#64843 = EDGE_CURVE ( 'NONE', #94991, #6037, #15133, .T. ) ;
#64844 = ORIENTED_EDGE ( 'NONE', *, *, #90348, .F. ) ;
#64845 = VECTOR ( 'NONE', #107102, 1000.000000000000000 ) ;
#64846 = ORIENTED_EDGE ( 'NONE', *, *, #10381, .F. ) ;
#64847 = CARTESIAN_POINT ( 'NONE',  ( 6.049999999999935874, 2.500000000000000000, -6.741600689897077281 ) ) ;
#64848 = CARTESIAN_POINT ( 'NONE',  ( -5.400000000000019895, 2.500000000000000000, 4.230127018922196669 ) ) ;
#64849 = CARTESIAN_POINT ( 'NONE',  ( 4.599999999999938360, 2.500000000000000000, -0.5928203230275541635 ) ) ;
#64850 = CARTESIAN_POINT ( 'NONE',  ( 13.54999999999989768, 2.500000000000000000, -2.511473670974877948 ) ) ;
#64851 = ORIENTED_EDGE ( 'NONE', *, *, #110774, .T. ) ;
#64852 = DIRECTION ( 'NONE',  ( 0.000000000000000000, 0.000000000000000000, 1.000000000000000000 ) ) ;
#64854 = CIRCLE ( 'NONE', #25149, 0.06509327318403745899 ) ;
#64853 = CIRCLE ( 'NONE', #127564, 0.1000000000000000056 ) ;
#64855 = LINE ( 'NONE', #5285, #124731 ) ;
#64856 = ORIENTED_EDGE ( 'NONE', *, *, #124648, .T. ) ;
#64857 = CARTESIAN_POINT ( 'NONE',  ( -13.54999999999998828, 12.50000000000000000, 1.818653347947325472 ) ) ;
#64858 = ORIENTED_EDGE ( 'NONE', *, *, #119965, .F. ) ;
#64859 = FACE_BOUND ( 'NONE', #45914, .T. ) ;
#64860 = FACE_OUTER_BOUND ( 'NONE', #36533, .T. ) ;
#64861 = ORIENTED_EDGE ( 'NONE', *, *, #867, .T. ) ;
#64862 = LINE ( 'NONE', #15094, #111230 ) ;
#64863 = DIRECTION ( 'NONE',  ( 0.000000000000000000, -0.9999939076577903929, 0.003490651415223739937 ) ) ;
#64864 = ORIENTED_EDGE ( 'NONE', *, *, #799, .T. ) ;
#64865 = ORIENTED_EDGE ( 'NONE', *, *, #127445, .T. ) ;
#64866 = CARTESIAN_POINT ( 'NONE',  ( 187.0052083336747444, -6.551208109652278289, 3.782341765624995134 ) ) ;
#64867 = DIRECTION ( 'NONE',  ( 0.000000000000000000, 0.000000000000000000, -1.000000000000000000 ) ) ;
#64868 = CARTESIAN_POINT ( 'NONE',  ( 13.74999999999989342, 12.50000000000000000, -1.472243186433550122 ) ) ;
#64869 = LINE ( 'NONE', #25587, #99637 ) ;
#64870 = CARTESIAN_POINT ( 'NONE',  ( -5.600000000000020073, 2.500000000000000000, 4.676537180435972552 ) ) ;
#64871 = PLANE ( 'NONE',  #64124 ) ;
#64872 = LINE ( 'NONE', #55070, #25481 ) ;
#64873 = AXIS2_PLACEMENT_3D ( 'NONE', #63495, #23562, #34699 ) ;
#64874 = EDGE_CURVE ( 'NONE', #80227, #109551, #3790, .T. ) ;
#64875 = AXIS2_PLACEMENT_3D ( 'NONE', #43083, #12289, #82994 ) ;
#64876 = ORIENTED_EDGE ( 'NONE', *, *, #43106, .T. ) ;
#64877 = ORIENTED_EDGE ( 'NONE', *, *, #91366, .F. ) ;
#64878 = CARTESIAN_POINT ( 'NONE',  ( 8.949999999999915801, 2.500000000000000000, -1.818653347947326138 ) ) ;
#64879 = LINE ( 'NONE', #34155, #126982 ) ;
#64880 = DIRECTION ( 'NONE',  ( 0.000000000000000000, 0.000000000000000000, 1.000000000000000000 ) ) ;
#64881 = CARTESIAN_POINT ( 'NONE',  ( 14.54999999999989591, 12.50000000000000000, 2.165063509461097713 ) ) ;
#64883 = VERTEX_POINT ( 'NONE', #113093 ) ;
#64882 = ORIENTED_EDGE ( 'NONE', *, *, #100325, .T. ) ;
#64884 = EDGE_CURVE ( 'NONE', #27262, #80417, #33273, .T. ) ;
#64885 = FACE_BOUND ( 'NONE', #44666, .T. ) ;
#64886 = ORIENTED_EDGE ( 'NONE', *, *, #96394, .T. ) ;
#64887 = EDGE_CURVE ( 'NONE', #14356, #73692, #27656, .T. ) ;
#64888 = FACE_OUTER_BOUND ( 'NONE', #43030, .T. ) ;
#64889 = DIRECTION ( 'NONE',  ( -0.000000000000000000, -1.000000000000000000, -0.000000000000000000 ) ) ;
#64890 = AXIS2_PLACEMENT_3D ( 'NONE', #66607, #97999, #37172 ) ;
#64891 = VERTEX_POINT ( 'NONE', #61442 ) ;
#64892 = CARTESIAN_POINT ( 'NONE',  ( -10.45000000000000107, 12.50000000000000000, 2.165063509461097713 ) ) ;
#64893 = FACE_OUTER_BOUND ( 'NONE', #82943, .T. ) ;
#64894 = CARTESIAN_POINT ( 'NONE',  ( 0.000000000000000000, 0.000000000000000000, -5.000000000000004441 ) ) ;
#64895 = CARTESIAN_POINT ( 'NONE',  ( 3.549999999999944755, 2.500000000000000000, -2.411473670974877859 ) ) ;
#64896 = EDGE_CURVE ( 'NONE', #17226, #39251, #123546, .T. ) ;
#64897 = CARTESIAN_POINT ( 'NONE',  ( 8.749999999999918288, 12.50000000000000000, -1.472243186433550122 ) ) ;
#64898 = DIRECTION ( 'NONE',  ( -0.000000000000000000, 1.000000000000000000, -0.000000000000000000 ) ) ;
#64899 = CARTESIAN_POINT ( 'NONE',  ( -3.300000000000027800, 2.500000000000000000, -2.276824562219559311E-15 ) ) ;
#64900 = DIRECTION ( 'NONE',  ( 0.000000000000000000, 0.000000000000000000, 1.000000000000000000 ) ) ;
#64901 = ADVANCED_FACE ( 'NONE', ( #52893 ), #56903, .T. ) ;
#64902 = FACE_OUTER_BOUND ( 'NONE', #126896, .T. ) ;
#64903 = AXIS2_PLACEMENT_3D ( 'NONE', #39424, #51163, #58408 ) ;
#64904 = VERTEX_POINT ( 'NONE', #31335 ) ;
#64905 = VERTEX_POINT ( 'NONE', #121617 ) ;
#64906 = CONICAL_SURFACE ( 'NONE', #87880, 0.09999999999999982514, 0.003490658503988666988 ) ;
#64907 = ORIENTED_EDGE ( 'NONE', *, *, #32846, .F. ) ;
#64908 = LINE ( 'NONE', #27548, #5298 ) ;
#64909 = EDGE_LOOP ( 'NONE', ( #96370, #54818 ) ) ;
#64910 = LINE ( 'NONE', #1006, #22695 ) ;
#64912 = ORIENTED_EDGE ( 'NONE', *, *, #51996, .F. ) ;
#64911 = ORIENTED_EDGE ( 'NONE', *, *, #29954, .F. ) ;
#64913 = ORIENTED_EDGE ( 'NONE', *, *, #123464, .F. ) ;
#64914 = DIRECTION ( 'NONE',  ( 0.000000000000000000, 0.000000000000000000, 1.000000000000000000 ) ) ;
#64915 = AXIS2_PLACEMENT_3D ( 'NONE', #39294, #79823, #29445 ) ;
#64916 = CARTESIAN_POINT ( 'NONE',  ( -11.89999999999999680, 2.500000000000000000, -4.676537180435976104 ) ) ;
#64917 = SURFACE_SIDE_STYLE ('',( #54460 ) ) ;
#64918 = CARTESIAN_POINT ( 'NONE',  ( 43.31340625576489600, -2.029328411527076437, -5.113049425671298387 ) ) ;
#64919 = CIRCLE ( 'NONE', #94171, 0.1000000000000002554 ) ;
#64920 = DIRECTION ( 'NONE',  ( 0.000000000000000000, 0.000000000000000000, -1.000000000000000000 ) ) ;
#64921 = CARTESIAN_POINT ( 'NONE',  ( -11.25000000000000000, 2.500000000000000000, -2.857883832488649745 ) ) ;
#64922 = VERTEX_POINT ( 'NONE', #112468 ) ;
#64923 = DIRECTION ( 'NONE',  ( 0.000000000000000000, 0.000000000000000000, -1.000000000000000000 ) ) ;
#64924 = EDGE_LOOP ( 'NONE', ( #53988, #53907, #69953, #32467 ) ) ;
#64925 = EDGE_LOOP ( 'NONE', ( #129563, #6172 ) ) ;
#64926 = VERTEX_POINT ( 'NONE', #23417 ) ;
#64927 = DIRECTION ( 'NONE',  ( 0.000000000000000000, 0.000000000000000000, 1.000000000000000000 ) ) ;
#64928 = ORIENTED_EDGE ( 'NONE', *, *, #126863, .T. ) ;
#64929 = ORIENTED_EDGE ( 'NONE', *, *, #18938, .T. ) ;
#64930 = ORIENTED_EDGE ( 'NONE', *, *, #85385, .T. ) ;
#64931 = FILL_AREA_STYLE ('',( #64299 ) ) ;
#64932 = CARTESIAN_POINT ( 'NONE',  ( 6.849999999999930367, 2.500000000000000000, -6.741600689897078169 ) ) ;
#64933 = DIRECTION ( 'NONE',  ( 0.000000000000000000, 1.000000000000000000, 0.000000000000000000 ) ) ;
#64934 = LINE ( 'NONE', #55773, #365 ) ;
#64935 = CARTESIAN_POINT ( 'NONE',  ( -10.00000000000000533, 12.50000000000000000, 0.6928203230275494784 ) ) ;
#64937 = EDGE_CURVE ( 'NONE', #86749, #92915, #44406, .T. ) ;
#64936 = CIRCLE ( 'NONE', #58696, 0.1000000000000000472 ) ;
#64938 = CARTESIAN_POINT ( 'NONE',  ( -1.850000000000033840, 2.500000000000000000, 6.941600689897073018 ) ) ;
#64939 = VERTEX_POINT ( 'NONE', #120988 ) ;
#64940 = CONICAL_SURFACE ( 'NONE', #8493, 0.1000000000000002554, 0.003490658503988666988 ) ;
#64941 = EDGE_CURVE ( 'NONE', #102506, #59130, #54854, .T. ) ;
#64942 = CIRCLE ( 'NONE', #41977, 0.09999999999999982514 ) ;
#64943 = EDGE_CURVE ( 'NONE', #45085, #33480, #121669, .T. ) ;
#64944 = DIRECTION ( 'NONE',  ( 0.000000000000000000, 0.000000000000000000, 1.000000000000000000 ) ) ;
#64945 = ORIENTED_EDGE ( 'NONE', *, *, #11975, .F. ) ;
#64946 = DIRECTION ( 'NONE',  ( 0.000000000000000000, 0.000000000000000000, 1.000000000000000000 ) ) ;
#64947 = AXIS2_PLACEMENT_3D ( 'NONE', #38118, #55819, #87200 ) ;
#64948 = ORIENTED_EDGE ( 'NONE', *, *, #70364, .F. ) ;
#64949 = DIRECTION ( 'NONE',  ( 0.000000000000000000, 0.000000000000000000, 1.000000000000000000 ) ) ;
#64950 = ADVANCED_FACE ( 'NONE', ( #1209 ), #125865, .T. ) ;
#64951 = EDGE_LOOP ( 'NONE', ( #57013, #78483, #101159, #72125 ) ) ;
#64952 = CONICAL_SURFACE ( 'NONE', #54571, 0.09999999999999982514, 0.003490658503988666988 ) ;
#64953 = ORIENTED_EDGE ( 'NONE', *, *, #117045, .F. ) ;
#64954 = DIRECTION ( 'NONE',  ( 0.000000000000000000, -0.000000000000000000, 1.000000000000000000 ) ) ;
#64955 = FACE_OUTER_BOUND ( 'NONE', #85402, .T. ) ;
#64956 = EDGE_CURVE ( 'NONE', #124385, #40490, #117537, .T. ) ;
#64957 = ADVANCED_FACE ( 'NONE', ( #2480 ), #469, .T. ) ;
#64958 = LINE ( 'NONE', #75423, #38433 ) ;
#64959 = FACE_OUTER_BOUND ( 'NONE', #90982, .T. ) ;
#64960 = ORIENTED_EDGE ( 'NONE', *, *, #8325, .F. ) ;
#64961 = CARTESIAN_POINT ( 'NONE',  ( -9.800000000000006040, 2.500000000000000000, -4.676537180435974328 ) ) ;
#64962 = CARTESIAN_POINT ( 'NONE',  ( 2.500000000000002220, 0.5000000000000002220, -9.999999999999998224 ) ) ;
#64963 = FACE_OUTER_BOUND ( 'NONE', #4561, .T. ) ;
#64964 = DIRECTION ( 'NONE',  ( 0.000000000000000000, -0.9999939076577903929, 0.003490651415223739937 ) ) ;
#64965 = EDGE_CURVE ( 'NONE', #14028, #107104, #107086, .T. ) ;
#64966 = DIRECTION ( 'NONE',  ( 0.000000000000000000, 1.000000000000000000, 0.000000000000000000 ) ) ;
#64967 = EDGE_LOOP ( 'NONE', ( #72702, #70287, #3530, #59994 ) ) ;
#64968 = EDGE_LOOP ( 'NONE', ( #53917, #51008, #57279, #18437 ) ) ;
#64969 = UNCERTAINTY_MEASURE_WITH_UNIT (LENGTH_MEASURE( 1.000000000000000082E-05 ), #129393, 'distance_accuracy_value', 'NONE');
#64970 = ORIENTED_EDGE ( 'NONE', *, *, #69506, .T. ) ;
#64971 = CARTESIAN_POINT ( 'NONE',  ( 6.849999999999927702, 2.500000000000000000, 2.511473670974873507 ) ) ;
#64972 = AXIS2_PLACEMENT_3D ( 'NONE', #81236, #84, #72703 ) ;
#64973 = DIRECTION ( 'NONE',  ( -0.000000000000000000, 1.000000000000000000, -0.000000000000000000 ) ) ;
#64974 = CIRCLE ( 'NONE', #75442, 0.06509327318403745899 ) ;
#64975 = CARTESIAN_POINT ( 'NONE',  ( 184.9218750003414016, 0.000000000000000000, 7.564683531250000925 ) ) ;
#64976 = DIRECTION ( 'NONE',  ( 0.000000000000000000, 0.000000000000000000, -1.000000000000000000 ) ) ;
#64977 = CARTESIAN_POINT ( 'NONE',  ( 11.89999999999990798, 12.50000000000000000, -3.983716857408426293 ) ) ;
#64978 = FACE_OUTER_BOUND ( 'NONE', #51757, .T. ) ;
#64979 = DIRECTION ( 'NONE',  ( 0.000000000000000000, -0.9999939076577903929, 0.003490651415223739937 ) ) ;
#64980 = ORIENTED_EDGE ( 'NONE', *, *, #16257, .T. ) ;
#64981 = CIRCLE ( 'NONE', #90106, 0.06509327318403745899 ) ;
#64982 = FACE_OUTER_BOUND ( 'NONE', #85317, .T. ) ;
#64983 = FACE_OUTER_BOUND ( 'NONE', #24952, .T. ) ;
#64984 = ORIENTED_EDGE ( 'NONE', *, *, #106983, .F. ) ;
#64985 = FACE_OUTER_BOUND ( 'NONE', #5619, .T. ) ;
#64986 = AXIS2_PLACEMENT_3D ( 'NONE', #58886, #73214, #62757 ) ;
#64987 = AXIS2_PLACEMENT_3D ( 'NONE', #52147, #2368, #52781 ) ;
#64988 = ADVANCED_FACE ( 'NONE', ( #35199 ), #21417, .T. ) ;
#64989 = ORIENTED_EDGE ( 'NONE', *, *, #33724, .T. ) ;
#64990 = DIRECTION ( 'NONE',  ( -0.000000000000000000, -1.000000000000000000, -0.000000000000000000 ) ) ;
#64991 = ORIENTED_EDGE ( 'NONE', *, *, #10660, .T. ) ;
#64992 = CARTESIAN_POINT ( 'NONE',  ( -4.150000000000024336, 2.500000000000000000, 2.065063509461097624 ) ) ;
#64993 = DIRECTION ( 'NONE',  ( -0.000000000000000000, -1.000000000000000000, -0.000000000000000000 ) ) ;
#64994 = FACE_OUTER_BOUND ( 'NONE', #21079, .T. ) ;
#64995 = AXIS2_PLACEMENT_3D ( 'NONE', #26069, #44412, #56780 ) ;
#64996 = VERTEX_POINT ( 'NONE', #115662 ) ;
#64997 = DIRECTION ( 'NONE',  ( -0.000000000000000000, -1.000000000000000000, -0.000000000000000000 ) ) ;
#64998 = DIRECTION ( 'NONE',  ( 0.000000000000000000, 1.000000000000000000, 0.000000000000000000 ) ) ;
#64999 = AXIS2_PLACEMENT_3D ( 'NONE', #32398, #63107, #72303 ) ;
#65000 = ORIENTED_EDGE ( 'NONE', *, *, #21037, .T. ) ;
#65001 = PLANE ( 'NONE',  #28549 ) ;
#65002 = VERTEX_POINT ( 'NONE', #65921 ) ;
#65003 = VERTEX_POINT ( 'NONE', #5706 ) ;
#65004 = DIRECTION ( 'NONE',  ( 0.000000000000000000, -0.000000000000000000, 1.000000000000000000 ) ) ;
#65005 = LINE ( 'NONE', #65663, #41677 ) ;
#65006 = ORIENTED_EDGE ( 'NONE', *, *, #37211, .F. ) ;
#65007 = DIRECTION ( 'NONE',  ( -0.000000000000000000, 1.000000000000000000, -0.000000000000000000 ) ) ;
#65008 = LINE ( 'NONE', #36231, #21367 ) ;
#65009 = EDGE_LOOP ( 'NONE', ( #81546, #4011, #36181, #62247 ) ) ;
#65010 = DIRECTION ( 'NONE',  ( 0.000000000000000000, 0.000000000000000000, 1.000000000000000000 ) ) ;
#65011 = FACE_OUTER_BOUND ( 'NONE', #110996, .T. ) ;
#65012 = CIRCLE ( 'NONE', #50460, 0.06509327318403745899 ) ;
#65013 = FACE_OUTER_BOUND ( 'NONE', #41719, .T. ) ;
#65014 = DIRECTION ( 'NONE',  ( 0.000000000000000000, 0.000000000000000000, 1.000000000000000000 ) ) ;
#65015 = AXIS2_PLACEMENT_3D ( 'NONE', #7315, #119217, #127119 ) ;
#65016 = AXIS2_PLACEMENT_3D ( 'NONE', #37593, #108247, #106947 ) ;
#65017 = FACE_OUTER_BOUND ( 'NONE', #112124, .T. ) ;
#65018 = CARTESIAN_POINT ( 'NONE',  ( 185.0312500006828031, 9.429780353434619030E-16, -7.700000000000000178 ) ) ;
#65019 = ADVANCED_FACE ( 'NONE', ( #14237 ), #115381, .T. ) ;
#65020 = ADVANCED_FACE ( 'NONE', ( #16158 ), #103927, .T. ) ;
#65021 = CIRCLE ( 'NONE', #14843, 0.09999999999999982514 ) ;
#65022 = ORIENTED_EDGE ( 'NONE', *, *, #124663, .T. ) ;
#65023 = VERTEX_POINT ( 'NONE', #114376 ) ;
#65024 = ORIENTED_EDGE ( 'NONE', *, *, #3809, .T. ) ;
#65025 = ORIENTED_EDGE ( 'NONE', *, *, #13371, .F. ) ;
#65026 = DIRECTION ( 'NONE',  ( 0.000000000000000000, -1.000000000000000000, -0.000000000000000000 ) ) ;
#65027 = DIRECTION ( 'NONE',  ( -4.274815082592931898E-19, -0.9999939076577903929, -0.003490651415223739937 ) ) ;
#65028 = CIRCLE ( 'NONE', #35813, 2.000000000000000000 ) ;
#65029 = DIRECTION ( 'NONE',  ( -4.274815082592931898E-19, -0.9999939076577903929, -0.003490651415223739937 ) ) ;
#65030 = VERTEX_POINT ( 'NONE', #45660 ) ;
#65031 = EDGE_CURVE ( 'NONE', #120113, #51434, #94570, .T. ) ;
#65032 = FACE_BOUND ( 'NONE', #115837, .T. ) ;
#65033 = EDGE_CURVE ( 'NONE', #103864, #35250, #73639, .T. ) ;
#65034 = FACE_OUTER_BOUND ( 'NONE', #111113, .T. ) ;
#65035 = DIRECTION ( 'NONE',  ( 0.000000000000000000, 0.000000000000000000, 1.000000000000000000 ) ) ;
#65036 = PLANE ( 'NONE',  #67927 ) ;
#65037 = DIRECTION ( 'NONE',  ( 0.000000000000000000, 1.000000000000000000, 0.000000000000000000 ) ) ;
#65038 = PLANE ( 'NONE',  #80537 ) ;
#65039 = ADVANCED_FACE ( 'NONE', ( #66561 ), #55473, .T. ) ;
#65040 = FACE_OUTER_BOUND ( 'NONE', #59898, .T. ) ;
#65041 = EDGE_CURVE ( 'NONE', #124608, #46240, #31893, .T. ) ;
#65042 = CARTESIAN_POINT ( 'NONE',  ( -11.84999999999999787, 2.500000000000000000, -6.841600689897074261 ) ) ;
#65043 = CARTESIAN_POINT ( 'NONE',  ( 3.749999999999942268, 12.50000000000000000, -1.407149913249512663 ) ) ;
#65044 = EDGE_CURVE ( 'NONE', #28259, #46373, #17179, .T. ) ;
#65045 = DIRECTION ( 'NONE',  ( 0.000000000000000000, 0.000000000000000000, 1.000000000000000000 ) ) ;
#65046 = ADVANCED_FACE ( 'NONE', ( #26658 ), #75692, .T. ) ;
#65047 = ADVANCED_FACE ( 'NONE', ( #94103 ), #38147, .T. ) ;
#65048 = DIRECTION ( 'NONE',  ( 0.000000000000000000, 0.000000000000000000, 1.000000000000000000 ) ) ;
#65049 = ORIENTED_EDGE ( 'NONE', *, *, #114417, .F. ) ;
#65050 = ORIENTED_EDGE ( 'NONE', *, *, #98337, .F. ) ;
#65051 = ORIENTED_EDGE ( 'NONE', *, *, #32295, .T. ) ;
#65052 = EDGE_LOOP ( 'NONE', ( #17328, #33323, #114125, #14162 ) ) ;
#65053 = DIRECTION ( 'NONE',  ( 0.000000000000000000, 0.000000000000000000, 1.000000000000000000 ) ) ;
#65054 = ORIENTED_EDGE ( 'NONE', *, *, #85283, .F. ) ;
#65055 = CARTESIAN_POINT ( 'NONE',  ( -3.950000000000028155, 12.50000000000000000, -6.841600689897077814 ) ) ;
#65056 = ORIENTED_EDGE ( 'NONE', *, *, #93158, .F. ) ;
#65057 = EDGE_CURVE ( 'NONE', #112512, #97470, #86191, .T. ) ;
#65058 = ORIENTED_EDGE ( 'NONE', *, *, #57081, .F. ) ;
#65059 = DIRECTION ( 'NONE',  ( 0.000000000000000000, 0.000000000000000000, 1.000000000000000000 ) ) ;
#65060 = AXIS2_PLACEMENT_3D ( 'NONE', #13110, #53064, #23592 ) ;
#65061 = CIRCLE ( 'NONE', #75530, 0.1000000000000002554 ) ;
#65062 = DIRECTION ( 'NONE',  ( 0.000000000000000000, 0.000000000000000000, 1.000000000000000000 ) ) ;
#65063 = DIRECTION ( 'NONE',  ( -4.274815082592931898E-19, -0.9999939076577903929, -0.003490651415223739937 ) ) ;
#65064 = DIRECTION ( 'NONE',  ( 0.000000000000000000, 0.000000000000000000, 1.000000000000000000 ) ) ;
#65065 = CARTESIAN_POINT ( 'NONE',  ( -11.24999999999996447, 12.50000000000000000, -6.430097255199260786 ) ) ;
#65066 = ORIENTED_EDGE ( 'NONE', *, *, #13359, .T. ) ;
#65067 = CONICAL_SURFACE ( 'NONE', #12744, 0.1000000000000002554, 0.003490658503988666988 ) ;
#65068 = AXIS2_PLACEMENT_3D ( 'NONE', #64786, #94250, #86354 ) ;
#65069 = ORIENTED_EDGE ( 'NONE', *, *, #14254, .T. ) ;
#65070 = EDGE_LOOP ( 'NONE', ( #6144, #87032, #58163, #33549 ) ) ;
#65072 = ORIENTED_EDGE ( 'NONE', *, *, #46925, .F. ) ;
#65071 = DIRECTION ( 'NONE',  ( -0.000000000000000000, -1.000000000000000000, -0.000000000000000000 ) ) ;
#65073 = DIRECTION ( 'NONE',  ( 0.000000000000000000, 0.000000000000000000, 1.000000000000000000 ) ) ;
#65074 =( BOUNDED_CURVE ( )  B_SPLINE_CURVE ( 2, ( #59757, #8039, #60398, #38160, #117995, #119942, #9985, #144, #40095, #29619, #28994, #28347, #108173, #99010, #18512, #129145, #58457, #9338, #39474, #30292, #79381, #100307, #98349, #119285, #4018, #70836, #100928, #21746, #72774, #21086, #1445, #43328, #63604, #43965, #33508, #110751, #61678, #61009, #83868, #11910, #12547, #121868, #53137, #52476, #93069, #73405, #11263, #92400, #113331, #30931, #2729, #23671, #32225, #72135, #41398, #42695, #82603, #112058, #51853, #103525, #13837, #51215, #2081, #111386, #91124, #101592, #91764, #22402, #81309, #3381, #53771, #121224, #42026, #93700, #31563, #62320, #83249, #122520, #123166, #71470, #81931, #102239, #32870, #62947, #112703 ),
 .UNSPECIFIED., .F., .F. ) 
 B_SPLINE_CURVE_WITH_KNOTS ( ( 3, 2, 2, 2, 2, 2, 2, 2, 2, 2, 2, 2, 2, 2, 2, 2, 2, 2, 2, 2, 2, 2, 2, 2, 2, 2, 2, 2, 2, 2, 2, 2, 2, 2, 2, 2, 2, 2, 2, 2, 2, 2, 3 ),
 ( 0.000000000000000000, 0.02380952380952380820, 0.04761904761904761640, 0.07142857142857142461, 0.09523809523809523281, 0.1190476190476190410, 0.1428571428571428492, 0.1666666666666666574, 0.1904761904761904656, 0.2142857142857142738, 0.2380952380952380820, 0.2619047619047619180, 0.2857142857142856984, 0.3095238095238095344, 0.3333333333333333148, 0.3571428571428571508, 0.3809523809523809312, 0.4047619047619047672, 0.4285714285714285476, 0.4523809523809523836, 0.4761904761904761640, 0.5000000000000000000, 0.5238095238095238360, 0.5476190476190476719, 0.5714285714285713969, 0.5952380952380952328, 0.6190476190476190688, 0.6428571428571429047, 0.6666666666666666297, 0.6904761904761904656, 0.7142857142857143016, 0.7380952380952381375, 0.7619047619047618625, 0.7857142857142856984, 0.8095238095238095344, 0.8333333333333333703, 0.8571428571428570953, 0.8809523809523809312, 0.9047619047619047672, 0.9285714285714286031, 0.9523809523809523281, 0.9761904761904761640, 1.000000000000000000 ),
 .UNSPECIFIED. ) 
 CURVE ( )  GEOMETRIC_REPRESENTATION_ITEM ( )  RATIONAL_B_SPLINE_CURVE ( ( 1.000000000000000000, 0.8660254037844387076, 1.000000000000000000, 0.8660254037844387076, 1.000000000000000000, 0.8660254037844387076, 1.000000000000000000, 0.8660254037844387076, 1.000000000000000000, 0.8660254037844387076, 1.000000000000000000, 0.8660254037844387076, 1.000000000000000000, 0.8660254037844387076, 1.000000000000000000, 0.8660254037844387076, 1.000000000000000000, 0.8660254037844387076, 1.000000000000000000, 0.8660254037844387076, 1.000000000000000000, 0.8660254037844387076, 1.000000000000000000, 0.8660254037844387076, 1.000000000000000000, 0.8660254037844387076, 1.000000000000000000, 0.8660254037844387076, 1.000000000000000000, 0.8660254037844387076, 1.000000000000000000, 0.8660254037844387076, 1.000000000000000000, 0.8660254037844387076, 1.000000000000000000, 0.8660254037844387076, 1.000000000000000000, 0.8660254037844387076, 1.000000000000000000, 0.8660254037844387076, 1.000000000000000000, 0.8660254037844387076, 1.000000000000000000, 0.8660254037844387076, 1.000000000000000000, 0.8660254037844387076, 1.000000000000000000, 0.8660254037844387076, 1.000000000000000000, 0.8660254037844387076, 1.000000000000000000, 0.8660254037844387076, 1.000000000000000000, 0.8660254037844387076, 1.000000000000000000, 0.8660254037844387076, 1.000000000000000000, 0.8660254037844387076, 1.000000000000000000, 0.8660254037844387076, 1.000000000000000000, 0.8660254037844387076, 1.000000000000000000, 0.8660254037844387076, 1.000000000000000000, 0.8660254037844387076, 1.000000000000000000, 0.8660254037844387076, 1.000000000000000000, 0.8660254037844387076, 1.000000000000000000, 0.8660254037844387076, 1.000000000000000000, 0.8660254037844387076, 1.000000000000000000, 0.8660254037844387076, 1.000000000000000000, 0.8660254037844387076, 1.000000000000000000, 0.8660254037844387076, 1.000000000000000000, 0.8660254037844387076, 1.000000000000000000, 0.8660254037844387076, 1.000000000000000000 ) ) 
 REPRESENTATION_ITEM ( '' )  );
#65075 = ORIENTED_EDGE ( 'NONE', *, *, #8066, .T. ) ;
#65076 = VERTEX_POINT ( 'NONE', #86854 ) ;
#65077 = VECTOR ( 'NONE', #44390, 1000.000000000000000 ) ;
#65078 = FACE_OUTER_BOUND ( 'NONE', #81454, .T. ) ;
#65079 = AXIS2_PLACEMENT_3D ( 'NONE', #16699, #76294, #116203 ) ;
#65080 = CARTESIAN_POINT ( 'NONE',  ( -8.150000000000009237, 12.50000000000000000, 6.841600689897072485 ) ) ;
#65081 = FACE_OUTER_BOUND ( 'NONE', #62897, .T. ) ;
#65082 = CARTESIAN_POINT ( 'NONE',  ( -0.6500000000000403233, 2.500000000000000000, 1.818653347947321475 ) ) ;
#65083 = AXIS2_PLACEMENT_3D ( 'NONE', #102504, #11538, #61944 ) ;
#65084 = DIRECTION ( 'NONE',  ( -0.000000000000000000, 1.000000000000000000, -0.000000000000000000 ) ) ;
#65085 = EDGE_CURVE ( 'NONE', #88607, #106514, #109138, .T. ) ;
#65086 = CONICAL_SURFACE ( 'NONE', #104792, 0.1000000000000000472, 0.003490658503988666988 ) ;
#65087 = VERTEX_POINT ( 'NONE', #84275 ) ;
#65088 = EDGE_CURVE ( 'NONE', #46379, #69366, #34563, .T. ) ;
#65089 = DIRECTION ( 'NONE',  ( -0.000000000000000000, -1.000000000000000000, -0.000000000000000000 ) ) ;
#65090 = ORIENTED_EDGE ( 'NONE', *, *, #48109, .F. ) ;
#65092 = EDGE_CURVE ( 'NONE', #11512, #107667, #64638, .T. ) ;
#65091 = CARTESIAN_POINT ( 'NONE',  ( 2.899999999999945732, 2.500000000000000000, -4.430127018922202176 ) ) ;
#65093 = VERTEX_POINT ( 'NONE', #94738 ) ;
#65094 = FACE_OUTER_BOUND ( 'NONE', #73151, .T. ) ;
#65095 = VECTOR ( 'NONE', #56082, 1000.000000000000000 ) ;
#65096 = DIRECTION ( 'NONE',  ( 0.000000000000000000, -0.000000000000000000, 1.000000000000000000 ) ) ;
#65097 = CARTESIAN_POINT ( 'NONE',  ( -8.550000000000013145, 2.500000000000000000, -6.841600689897073373 ) ) ;
#65098 = EDGE_CURVE ( 'NONE', #60150, #97364, #48721, .T. ) ;
#65099 = CARTESIAN_POINT ( 'NONE',  ( 4.999999999999935163, 2.500000000000000000, 0.6928203230275494784 ) ) ;
#65100 = EDGE_LOOP ( 'NONE', ( #119220, #57955, #114407, #128121 ) ) ;
#65101 = EDGE_CURVE ( 'NONE', #84066, #99278, #100915, .T. ) ;
#65102 = DIRECTION ( 'NONE',  ( -0.000000000000000000, -1.000000000000000000, -0.000000000000000000 ) ) ;
#65103 = ADVANCED_FACE ( 'NONE', ( #118898 ), #27766, .T. ) ;
#65104 = ADVANCED_FACE ( 'NONE', ( #39077 ), #90446, .T. ) ;
#65105 = DIRECTION ( 'NONE',  ( 0.000000000000000000, -0.000000000000000000, 1.000000000000000000 ) ) ;
#65106 = ORIENTED_EDGE ( 'NONE', *, *, #9825, .F. ) ;
#65107 = ORIENTED_EDGE ( 'NONE', *, *, #70254, .T. ) ;
#65108 = ORIENTED_EDGE ( 'NONE', *, *, #59030, .T. ) ;
#65109 = DIRECTION ( 'NONE',  ( 0.000000000000000000, 1.000000000000000000, 0.000000000000000000 ) ) ;
#65110 = DIRECTION ( 'NONE',  ( 0.000000000000000000, 1.000000000000000000, 0.000000000000000000 ) ) ;
#65111 = CARTESIAN_POINT ( 'NONE',  ( 185.6927083336747160, 6.551208109652275624, -3.782341765624998686 ) ) ;
#65112 = DIRECTION ( 'NONE',  ( 0.000000000000000000, 0.000000000000000000, -1.000000000000000000 ) ) ;
#65113 = ADVANCED_FACE ( 'NONE', ( #28592 ), #88794, .T. ) ;
#65114 = FACE_OUTER_BOUND ( 'NONE', #11969, .T. ) ;
#65115 = DIRECTION ( 'NONE',  ( -0.000000000000000000, 1.000000000000000000, -0.000000000000000000 ) ) ;
#65116 = CIRCLE ( 'NONE', #127821, 0.1000000000000002554 ) ;
#65117 = AXIS2_PLACEMENT_3D ( 'NONE', #96040, #5072, #6336 ) ;
#65118 = CONICAL_SURFACE ( 'NONE', #102775, 0.1000000000000002554, 0.003490658503988666988 ) ;
#65119 = ORIENTED_EDGE ( 'NONE', *, *, #27273, .F. ) ;
#65120 = FACE_OUTER_BOUND ( 'NONE', #28626, .T. ) ;
#65121 = AXIS2_PLACEMENT_3D ( 'NONE', #76361, #58655, #107085 ) ;
#65122 = ORIENTED_EDGE ( 'NONE', *, *, #6599, .F. ) ;
#65123 = CIRCLE ( 'NONE', #40111, 0.06509327318403745899 ) ;
#65124 = CARTESIAN_POINT ( 'NONE',  ( 7.699999999999925571, 2.500000000000000000, 3.883716857408420431 ) ) ;
#65125 = EDGE_CURVE ( 'NONE', #17389, #104949, #19350, .T. ) ;
#65126 = CARTESIAN_POINT ( 'NONE',  ( 5.449999999999936229, 2.500000000000000000, -2.065063509461102065 ) ) ;
#65127 = DIRECTION ( 'NONE',  ( 0.000000000000000000, 0.000000000000000000, -1.000000000000000000 ) ) ;
#65128 = ORIENTED_EDGE ( 'NONE', *, *, #38799, .T. ) ;
#65129 = CIRCLE ( 'NONE', #23369, 0.06509327318403745899 ) ;
#65130 = CARTESIAN_POINT ( 'NONE',  ( -11.84999999999999787, 2.500000000000000000, -1.718653347947321830 ) ) ;
#65131 = CARTESIAN_POINT ( 'NONE',  ( 1.449999999999952216, 2.500000000000000000, -2.511473670974877948 ) ) ;
#65132 = VERTEX_POINT ( 'NONE', #58059 ) ;
#65133 = CARTESIAN_POINT ( 'NONE',  ( -15.79999999999998117, 12.50000000000000000, -0.06509327318403743123 ) ) ;
#65134 = ADVANCED_FACE ( 'NONE', ( #127439 ), #128128, .T. ) ;
#65135 = ORIENTED_EDGE ( 'NONE', *, *, #106873, .F. ) ;
#65136 = VERTEX_POINT ( 'NONE', #118250 ) ;
#65137 = DIRECTION ( 'NONE',  ( 0.000000000000000000, 0.000000000000000000, 1.000000000000000000 ) ) ;
#65138 = VERTEX_POINT ( 'NONE', #68502 ) ;
#65139 = DIRECTION ( 'NONE',  ( 0.000000000000000000, -0.000000000000000000, 1.000000000000000000 ) ) ;
#65140 = DIRECTION ( 'NONE',  ( 0.000000000000000000, 0.000000000000000000, -1.000000000000000000 ) ) ;
#65141 = LINE ( 'NONE', #27814, #96082 ) ;
#65142 = AXIS2_PLACEMENT_3D ( 'NONE', #34577, #25356, #83026 ) ;
#65143 = ORIENTED_EDGE ( 'NONE', *, *, #867, .F. ) ;
#65144 = AXIS2_PLACEMENT_3D ( 'NONE', #32950, #82686, #24395 ) ;
#65145 = FACE_BOUND ( 'NONE', #25145, .T. ) ;
#65147 = ORIENTED_EDGE ( 'NONE', *, *, #82727, .T. ) ;
#65146 = CARTESIAN_POINT ( 'NONE',  ( -7.300000000000016698, 2.500000000000000000, -4.776537180435978414 ) ) ;
#65148 = CARTESIAN_POINT ( 'NONE',  ( 7.699999999999925571, 2.500000000000000000, -4.676537180435978769 ) ) ;
#65149 = EDGE_CURVE ( 'NONE', #15822, #16690, #121853, .T. ) ;
#65150 = DIRECTION ( 'NONE',  ( 0.000000000000000000, 0.000000000000000000, 1.000000000000000000 ) ) ;
#65151 = EDGE_LOOP ( 'NONE', ( #35630, #40820 ) ) ;
#65152 = AXIS2_PLACEMENT_3D ( 'NONE', #72989, #25824, #104382 ) ;
#65153 = VECTOR ( 'NONE', #99325, 1000.000000000000000 ) ;
#65154 = ORIENTED_EDGE ( 'NONE', *, *, #30584, .F. ) ;
#65155 = CONICAL_SURFACE ( 'NONE', #8730, 0.1000000000000002554, 0.003490658503988666988 ) ;
#65156 = VERTEX_POINT ( 'NONE', #69799 ) ;
#65157 = CARTESIAN_POINT ( 'NONE',  ( -3.550000000000028244, 12.50000000000000000, -1.753560074763288679 ) ) ;
#65158 = FACE_OUTER_BOUND ( 'NONE', #50418, .T. ) ;
#65159 = DIRECTION ( 'NONE',  ( -0.000000000000000000, 1.000000000000000000, -0.000000000000000000 ) ) ;
#65160 = FACE_BOUND ( 'NONE', #96811, .T. ) ;
#65161 = ORIENTED_EDGE ( 'NONE', *, *, #80300, .F. ) ;
#65162 = CARTESIAN_POINT ( 'NONE',  ( 186.0677083336747444, -4.367472073101514418, -7.564683531250002702 ) ) ;
#65163 = CARTESIAN_POINT ( 'NONE',  ( -4.600000000000025402, 12.50000000000000000, 4.395220292106234439 ) ) ;
#65164 = CARTESIAN_POINT ( 'NONE',  ( -1.450000000000036371, 12.50000000000000000, 6.776507416713035248 ) ) ;
#65165 = AXIS2_PLACEMENT_3D ( 'NONE', #118778, #29130, #69023 ) ;
#65166 = AXIS2_PLACEMENT_3D ( 'NONE', #25743, #44095, #104311 ) ;
#65167 = LINE ( 'NONE', #56004, #63794 ) ;
#65168 = AXIS2_PLACEMENT_3D ( 'NONE', #76149, #56491, #57146 ) ;
#65169 = VECTOR ( 'NONE', #51283, 1000.000000000000000 ) ;
#65170 = CIRCLE ( 'NONE', #86099, 0.06509327318403745899 ) ;
#65171 = DIRECTION ( 'NONE',  ( 0.000000000000000000, 0.000000000000000000, 1.000000000000000000 ) ) ;
#65172 = DIRECTION ( 'NONE',  ( -0.000000000000000000, -1.000000000000000000, -0.000000000000000000 ) ) ;
#65173 = DIRECTION ( 'NONE',  ( -0.000000000000000000, -1.000000000000000000, -0.000000000000000000 ) ) ;
#65174 = CARTESIAN_POINT ( 'NONE',  ( 0.6499999999999543920, 2.500000000000000000, 6.048780366869521252 ) ) ;
#65175 = DIRECTION ( 'NONE',  ( 0.000000000000000000, 0.000000000000000000, 1.000000000000000000 ) ) ;
#65176 = EDGE_CURVE ( 'NONE', #30638, #61247, #65419, .T. ) ;
#65177 = VERTEX_POINT ( 'NONE', #88114 ) ;
#65178 = AXIS2_PLACEMENT_3D ( 'NONE', #120589, #21092, #112063 ) ;
#65179 = ORIENTED_EDGE ( 'NONE', *, *, #62771, .T. ) ;
#65180 = ORIENTED_EDGE ( 'NONE', *, *, #127946, .T. ) ;
#65181 = ORIENTED_EDGE ( 'NONE', *, *, #105170, .F. ) ;
#65182 = EDGE_LOOP ( 'NONE', ( #43005, #118966 ) ) ;
#65183 = CARTESIAN_POINT ( 'NONE',  ( 0.5999999999999560130, 12.50000000000000000, -3.918623584224389056 ) ) ;
#65184 = CARTESIAN_POINT ( 'NONE',  ( 7.949999999999922018, 2.500000000000000000, -2.165063509461101710 ) ) ;
#65185 = ORIENTED_EDGE ( 'NONE', *, *, #4742, .F. ) ;
#65186 = FACE_BOUND ( 'NONE', #63732, .T. ) ;
#65187 = DIRECTION ( 'NONE',  ( 0.000000000000000000, 0.000000000000000000, 1.000000000000000000 ) ) ;
#65188 = DIRECTION ( 'NONE',  ( 0.000000000000000000, 0.000000000000000000, 1.000000000000000000 ) ) ;
#65189 = VERTEX_POINT ( 'NONE', #108426 ) ;
#65190 = ADVANCED_FACE ( 'NONE', ( #109729 ), #59080, .T. ) ;
#65191 = CARTESIAN_POINT ( 'NONE',  ( -13.29999999999998828, 12.50000000000000000, 4.330127018922196314 ) ) ;
#65192 = ADVANCED_FACE ( 'NONE', ( #107128 ), #15228, .T. ) ;
#65193 = DIRECTION ( 'NONE',  ( -0.000000000000000000, -1.000000000000000000, -0.000000000000000000 ) ) ;
#65194 = ADVANCED_FACE ( 'NONE', ( #20067 ), #37761, .T. ) ;
#65195 = LINE ( 'NONE', #94671, #85136 ) ;
#65196 = ADVANCED_FACE ( 'NONE', ( #39726 ), #25608, .T. ) ;
#65197 = ORIENTED_EDGE ( 'NONE', *, *, #54598, .F. ) ;
#65198 = FACE_OUTER_BOUND ( 'NONE', #43457, .T. ) ;
#65199 = ORIENTED_EDGE ( 'NONE', *, *, #29947, .F. ) ;
#65200 = EDGE_CURVE ( 'NONE', #128448, #110183, #79998, .T. ) ;
#65201 = EDGE_LOOP ( 'NONE', ( #120507, #124427 ) ) ;
#65202 = CONICAL_SURFACE ( 'NONE', #2506, 0.1000000000000002554, 0.003490658503988666988 ) ;
#65203 = ORIENTED_EDGE ( 'NONE', *, *, #9284, .F. ) ;
#65204 = CIRCLE ( 'NONE', #92405, 0.06509327318403745899 ) ;
#65205 = CARTESIAN_POINT ( 'NONE',  ( 2.049999999999950084, 12.50000000000000000, -2.165063509461101710 ) ) ;
#65206 = CIRCLE ( 'NONE', #54746, 0.06509327318403745899 ) ;
#65207 = DIRECTION ( 'NONE',  ( -4.274815082592931898E-19, -0.9999939076577903929, -0.003490651415223739937 ) ) ;
#65208 = DIRECTION ( 'NONE',  ( 0.000000000000000000, -1.846105847067148515E-16, -1.000000000000000000 ) ) ;
#65209 = ORIENTED_EDGE ( 'NONE', *, *, #122767, .F. ) ;
#65210 = EDGE_CURVE ( 'NONE', #80531, #125538, #117627, .T. ) ;
#65211 = CARTESIAN_POINT ( 'NONE',  ( 13.39473262194674774, 2.500000000000000000, -7.044698189560237189 ) ) ;
#65212 = EDGE_CURVE ( 'NONE', #78931, #36319, #17280, .T. ) ;
#65213 = DIRECTION ( 'NONE',  ( -0.000000000000000000, -1.000000000000000000, -0.000000000000000000 ) ) ;
#65215 = ADVANCED_FACE ( 'NONE', ( #12154 ), #32485, .T. ) ;
#65214 = TOROIDAL_SURFACE ( 'NONE', #96604, 4.500000000000003553, 0.5000000000000000000 ) ;
#65216 = VECTOR ( 'NONE', #26829, 1000.000000000000000 ) ;
#65217 = CIRCLE ( 'NONE', #117428, 0.06509327318403745899 ) ;
#65218 = FACE_OUTER_BOUND ( 'NONE', #75385, .T. ) ;
#65219 = CARTESIAN_POINT ( 'NONE',  ( 187.1927083336747160, 6.551208109652275624, -3.782341765624998686 ) ) ;
#65220 = DIRECTION ( 'NONE',  ( 0.000000000000000000, 1.000000000000000000, 0.000000000000000000 ) ) ;
#65221 = AXIS2_PLACEMENT_3D ( 'NONE', #114183, #23879, #103727 ) ;
#65222 = AXIS2_PLACEMENT_3D ( 'NONE', #85280, #106219, #104904 ) ;
#65223 = PLANE ( 'NONE',  #93406 ) ;
#65224 = ADVANCED_FACE ( 'NONE', ( #52099 ), #33119, .T. ) ;
#65225 = ORIENTED_EDGE ( 'NONE', *, *, #38522, .T. ) ;
#65226 = CARTESIAN_POINT ( 'NONE',  ( 5.849999999999933031, 12.50000000000000000, -1.472243186433550122 ) ) ;
#65227 = AXIS2_PLACEMENT_3D ( 'NONE', #21496, #11012, #93461 ) ;
#65228 = ORIENTED_EDGE ( 'NONE', *, *, #81147, .F. ) ;
#65229 = ORIENTED_EDGE ( 'NONE', *, *, #38145, .T. ) ;
#65230 = PLANE ( 'NONE',  #24176 ) ;
#65231 = DIRECTION ( 'NONE',  ( -0.000000000000000000, -1.000000000000000000, -0.000000000000000000 ) ) ;
#65232 = CARTESIAN_POINT ( 'NONE',  ( -9.150000000000009237, 2.500000000000000000, 1.472243186433545459 ) ) ;
#65233 = CARTESIAN_POINT ( 'NONE',  ( 12.29999999999990479, 12.50000000000000000, 4.611443907251934426 ) ) ;
#65234 = CARTESIAN_POINT ( 'NONE',  ( 4.349999999999936584, 2.500000000000000000, 6.248780366869520542 ) ) ;
#65235 = ORIENTED_EDGE ( 'NONE', *, *, #99264, .T. ) ;
#65236 = VERTEX_POINT ( 'NONE', #21336 ) ;
#65237 = DIRECTION ( 'NONE',  ( 0.000000000000000000, 0.000000000000000000, -1.000000000000000000 ) ) ;
#65238 = CARTESIAN_POINT ( 'NONE',  ( 8.099999999999921485, 2.500000000000000000, 0.3464101615137735735 ) ) ;
#65239 = FACE_OUTER_BOUND ( 'NONE', #14534, .T. ) ;
#65240 = ORIENTED_EDGE ( 'NONE', *, *, #33586, .T. ) ;
#65241 = ORIENTED_EDGE ( 'NONE', *, *, #41637, .T. ) ;
#65242 = LINE ( 'NONE', #114355, #8088 ) ;
#65244 = EDGE_LOOP ( 'NONE', ( #92003, #81114 ) ) ;
#65243 = AXIS2_PLACEMENT_3D ( 'NONE', #16178, #16812, #35845 ) ;
#65245 = FACE_OUTER_BOUND ( 'NONE', #61304, .T. ) ;
#65246 = FACE_OUTER_BOUND ( 'NONE', #30287, .T. ) ;
#65247 = VERTEX_POINT ( 'NONE', #61277 ) ;
#65248 = LINE ( 'NONE', #67165, #102538 ) ;
#65249 = CARTESIAN_POINT ( 'NONE',  ( -5.000000000000022204, 2.500000000000000000, 3.637306695894644726 ) ) ;
#65250 = FACE_OUTER_BOUND ( 'NONE', #72966, .T. ) ;
#65252 = AXIS2_PLACEMENT_3D ( 'NONE', #9632, #99951, #10281 ) ;
#65251 = FACE_OUTER_BOUND ( 'NONE', #88076, .T. ) ;
#65253 = ORIENTED_EDGE ( 'NONE', *, *, #61499, .F. ) ;
#65254 = AXIS2_PLACEMENT_3D ( 'NONE', #81386, #31629, #71540 ) ;
#65255 = ADVANCED_FACE ( 'NONE', ( #60642 ), #98776, .T. ) ;
#65256 = VECTOR ( 'NONE', #63038, 1000.000000000000000 ) ;
#65257 = FACE_OUTER_BOUND ( 'NONE', #91695, .T. ) ;
#65258 = AXIS2_PLACEMENT_3D ( 'NONE', #47290, #54037, #27002 ) ;
#65260 = EDGE_CURVE ( 'NONE', #121148, #24001, #121762, .T. ) ;
#65259 = DIRECTION ( 'NONE',  ( 0.000000000000000000, 0.000000000000000000, -1.000000000000000000 ) ) ;
#65261 = ORIENTED_EDGE ( 'NONE', *, *, #59904, .F. ) ;
#65262 = ORIENTED_EDGE ( 'NONE', *, *, #11742, .T. ) ;
#65263 = CARTESIAN_POINT ( 'NONE',  ( -5.600000000000020073, 12.50000000000000000, 0.3464101615137736845 ) ) ;
#65264 = PLANE ( 'NONE',  #103448 ) ;
#65265 = FACE_OUTER_BOUND ( 'NONE', #10870, .T. ) ;
#65266 = DIRECTION ( 'NONE',  ( -0.000000000000000000, 1.000000000000000000, -0.000000000000000000 ) ) ;
#65267 = CONICAL_SURFACE ( 'NONE', #82005, 0.1000000000000002554, 0.003490658503988666988 ) ;
#65268 = LINE ( 'NONE', #95392, #113801 ) ;
#65269 = EDGE_CURVE ( 'NONE', #54407, #14513, #105127, .T. ) ;
#65270 = DIRECTION ( 'NONE',  ( 0.000000000000000000, 0.000000000000000000, 1.000000000000000000 ) ) ;
#65271 = CIRCLE ( 'NONE', #52754, 0.06509327318403745899 ) ;
#65272 = DIRECTION ( 'NONE',  ( -4.274815082592931898E-19, -0.9999939076577903929, -0.003490651415223739937 ) ) ;
#65273 = VECTOR ( 'NONE', #32771, 1000.000000000000000 ) ;
#65274 = DIRECTION ( 'NONE',  ( -0.000000000000000000, -1.000000000000000000, -0.000000000000000000 ) ) ;
#65275 = CIRCLE ( 'NONE', #25556, 0.06509327318403745899 ) ;
#65276 = CARTESIAN_POINT ( 'NONE',  ( 8.149999999999923972, 2.500000000000000000, 1.718653347947321386 ) ) ;
#65277 = CIRCLE ( 'NONE', #10880, 0.1000000000000000056 ) ;
#65278 = CARTESIAN_POINT ( 'NONE',  ( 4.599999999999938360, 2.500000000000000000, -0.6928203230275541413 ) ) ;
#65279 = AXIS2_PLACEMENT_3D ( 'NONE', #57636, #68732, #98832 ) ;
#65280 = CARTESIAN_POINT ( 'NONE',  ( 12.09999999999990550, 2.500000000000000000, 5.122947341949749323 ) ) ;
#65281 = VERTEX_POINT ( 'NONE', #112309 ) ;
#65282 = AXIS2_PLACEMENT_3D ( 'NONE', #56191, #35916, #43831 ) ;
#65283 = ORIENTED_EDGE ( 'NONE', *, *, #39284, .T. ) ;
#65284 = ORIENTED_EDGE ( 'NONE', *, *, #36588, .F. ) ;
#65285 = DIRECTION ( 'NONE',  ( 0.000000000000000000, 0.000000000000000000, 1.000000000000000000 ) ) ;
#65286 = DIRECTION ( 'NONE',  ( 0.000000000000000000, 1.000000000000000000, 0.000000000000000000 ) ) ;
#65287 = DIRECTION ( 'NONE',  ( 0.000000000000000000, 1.000000000000000000, 0.000000000000000000 ) ) ;
#65288 = ORIENTED_EDGE ( 'NONE', *, *, #51657, .T. ) ;
#65289 = CARTESIAN_POINT ( 'NONE',  ( 18.09027855933934603, -2.526462839860887488, -2.685672775344543961 ) ) ;
#65290 = CARTESIAN_POINT ( 'NONE',  ( 11.44999999999990870, 12.50000000000000000, 6.906693963081109722 ) ) ;
#65292 = ORIENTED_EDGE ( 'NONE', *, *, #109740, .F. ) ;
#65291 = DIRECTION ( 'NONE',  ( 0.000000000000000000, 0.000000000000000000, -1.000000000000000000 ) ) ;
#65293 = DIRECTION ( 'NONE',  ( -0.000000000000000000, -1.000000000000000000, -0.000000000000000000 ) ) ;
#65294 = EDGE_LOOP ( 'NONE', ( #56545, #55188, #126323, #54785 ) ) ;
#65295 = ORIENTED_EDGE ( 'NONE', *, *, #19444, .T. ) ;
#65296 = VERTEX_POINT ( 'NONE', #31184 ) ;
#65297 = CIRCLE ( 'NONE', #73709, 0.06509327318403745899 ) ;
#65298 = ORIENTED_EDGE ( 'NONE', *, *, #87831, .F. ) ;
#65299 = CARTESIAN_POINT ( 'NONE',  ( 5.449999999999936229, 2.500000000000000000, -2.265063509461101798 ) ) ;
#65300 = AXIS2_PLACEMENT_3D ( 'NONE', #4512, #53012, #3264 ) ;
#65301 = CIRCLE ( 'NONE', #40289, 0.09999999999999999167 ) ;
#65302 = DIRECTION ( 'NONE',  ( 0.000000000000000000, 0.000000000000000000, 1.000000000000000000 ) ) ;
#65303 = CARTESIAN_POINT ( 'NONE',  ( 5.599999999999933031, 12.50000000000000000, -0.3464101615137783474 ) ) ;
#65304 = CARTESIAN_POINT ( 'NONE',  ( 3.549999999999944755, 12.50000000000000000, -6.841600689897077814 ) ) ;
#65306 = VERTEX_POINT ( 'NONE', #92016 ) ;
#65305 = CONICAL_SURFACE ( 'NONE', #38136, 0.1000000000000002554, 0.003490658503988666988 ) ;
#65307 = CIRCLE ( 'NONE', #111270, 0.09999999999999982514 ) ;
#65308 = AXIS2_PLACEMENT_3D ( 'NONE', #91654, #82497, #81824 ) ;
#65309 = DIRECTION ( 'NONE',  ( 0.000000000000000000, 0.000000000000000000, 1.000000000000000000 ) ) ;
#65312 = ORIENTED_EDGE ( 'NONE', *, *, #99833, .T. ) ;
#65311 = EDGE_CURVE ( 'NONE', #27245, #125732, #75787, .T. ) ;
#65310 = CIRCLE ( 'NONE', #46531, 0.1000000000000000056 ) ;
#65313 = CARTESIAN_POINT ( 'NONE',  ( 87.50000000000001421, -3.974992050023849810, -6.359987280038161828 ) ) ;
#65314 = DIRECTION ( 'NONE',  ( -0.000000000000000000, -1.000000000000000000, -0.000000000000000000 ) ) ;
#65315 = VECTOR ( 'NONE', #24850, 1000.000000000000000 ) ;
#65316 = CARTESIAN_POINT ( 'NONE',  ( 8.349999999999919709, 12.50000000000000000, 6.560283801567334372 ) ) ;
#65317 = CARTESIAN_POINT ( 'NONE',  ( 17.29982614914667849, -2.489966891809442195, 2.989943721779569241 ) ) ;
#65318 = EDGE_CURVE ( 'NONE', #24755, #115443, #41656, .T. ) ;
#65319 = AXIS2_PLACEMENT_3D ( 'NONE', #70447, #11520, #2998 ) ;
#65320 = ORIENTED_EDGE ( 'NONE', *, *, #15271, .T. ) ;
#65321 = ORIENTED_EDGE ( 'NONE', *, *, #13755, .T. ) ;
#65322 = ORIENTED_EDGE ( 'NONE', *, *, #72214, .T. ) ;
#65323 = CARTESIAN_POINT ( 'NONE',  ( -5.000000000000022204, 2.500000000000000000, 3.737306695894644371 ) ) ;
#65324 = PLANE ( 'NONE',  #39445 ) ;
#65325 = EDGE_CURVE ( 'NONE', #93435, #65003, #13083, .T. ) ;
#65326 = CARTESIAN_POINT ( 'NONE',  ( 10.19999999999991225, 12.50000000000000000, 3.983716857408420076 ) ) ;
#65327 = FACE_BOUND ( 'NONE', #64112, .T. ) ;
#65328 = LINE ( 'NONE', #85623, #26406 ) ;
#65329 = DIRECTION ( 'NONE',  ( 0.000000000000000000, 1.000000000000000000, 0.000000000000000000 ) ) ;
#65330 = DIRECTION ( 'NONE',  ( -0.000000000000000000, -1.000000000000000000, -0.000000000000000000 ) ) ;
#65331 = CARTESIAN_POINT ( 'NONE',  ( -13.14999999999999147, 2.500000000000000000, -1.918653347947324006 ) ) ;
#65332 = AXIS2_PLACEMENT_3D ( 'NONE', #55978, #76277, #67066 ) ;
#65333 = CARTESIAN_POINT ( 'NONE',  ( 187.3802083336747444, 4.367472073101515306, 7.564683531250000925 ) ) ;
#65334 = CARTESIAN_POINT ( 'NONE',  ( 14.79999999999989235, 12.50000000000000000, 0.4115034346978109769 ) ) ;
#65335 = LINE ( 'NONE', #66630, #78451 ) ;
#65336 = AXIS2_PLACEMENT_3D ( 'NONE', #106358, #115512, #27788 ) ;
#65337 = CIRCLE ( 'NONE', #96730, 0.06509327318403745899 ) ;
#65338 = VECTOR ( 'NONE', #2742, 1000.000000000000000 ) ;
#65339 = DIRECTION ( 'NONE',  ( 0.000000000000000000, 0.000000000000000000, 1.000000000000000000 ) ) ;
#65340 = EDGE_CURVE ( 'NONE', #46062, #29998, #100539, .T. ) ;
#65341 = ORIENTED_EDGE ( 'NONE', *, *, #22528, .T. ) ;
#65342 = ORIENTED_EDGE ( 'NONE', *, *, #122220, .F. ) ;
#65343 = ORIENTED_EDGE ( 'NONE', *, *, #52322, .F. ) ;
#65344 = ORIENTED_EDGE ( 'NONE', *, *, #121057, .F. ) ;
#65345 = DIRECTION ( 'NONE',  ( 0.000000000000000000, 1.000000000000000000, 0.000000000000000000 ) ) ;
#65346 = FACE_BOUND ( 'NONE', #82000, .T. ) ;
#65347 = CIRCLE ( 'NONE', #52743, 0.06509327318403745899 ) ;
#65348 = CARTESIAN_POINT ( 'NONE',  ( -13.29999999999999005, 12.50000000000000000, 1.843143693225357538E-15 ) ) ;
#65350 = EDGE_CURVE ( 'NONE', #7100, #60983, #109234, .T. ) ;
#65349 = AXIS2_PLACEMENT_3D ( 'NONE', #53797, #24985, #112733 ) ;
#65351 = ORIENTED_EDGE ( 'NONE', *, *, #55916, .T. ) ;
#65352 = EDGE_CURVE ( 'NONE', #60457, #26852, #86243, .T. ) ;
#65353 = CARTESIAN_POINT ( 'NONE',  ( 43.31961220463728068, 2.029667686321675824, 5.113275312219439428 ) ) ;
#65354 = EDGE_CURVE ( 'NONE', #42353, #40264, #40355, .T. ) ;
#65355 = CARTESIAN_POINT ( 'NONE',  ( -9.999999999999969802, 12.50000000000000000, 4.330127018922196314 ) ) ;
#65356 = EDGE_CURVE ( 'NONE', #120673, #9996, #12789, .T. ) ;
#65357 = ADVANCED_FACE ( 'NONE', ( #1054 ), #107181, .T. ) ;
#65358 = ORIENTED_EDGE ( 'NONE', *, *, #110647, .T. ) ;
#65359 = CARTESIAN_POINT ( 'NONE',  ( 5.849999999999934808, 2.500000000000000000, -5.702370205355749455 ) ) ;
#65360 = DIRECTION ( 'NONE',  ( -4.274815082592931898E-19, -0.9999939076577903929, -0.003490651415223739937 ) ) ;
#65361 = AXIS2_PLACEMENT_3D ( 'NONE', #75980, #28833, #119774 ) ;
#65362 = AXIS2_PLACEMENT_3D ( 'NONE', #18890, #128886, #107922 ) ;
#65363 = AXIS2_PLACEMENT_3D ( 'NONE', #117089, #27424, #7793 ) ;
#65364 = CIRCLE ( 'NONE', #92567, 0.06509327318403745899 ) ;
#65365 = ADVANCED_FACE ( 'NONE', ( #80271 ), #67448, .T. ) ;
#65366 = ORIENTED_EDGE ( 'NONE', *, *, #21182, .T. ) ;
#65367 = FACE_OUTER_BOUND ( 'NONE', #48200, .T. ) ;
#65368 = EDGE_CURVE ( 'NONE', #111104, #17511, #123911, .T. ) ;
#65369 = LINE ( 'NONE', #105310, #1545 ) ;
#65370 = VECTOR ( 'NONE', #123622, 1000.000000000000000 ) ;
#65371 = ADVANCED_FACE ( 'NONE', ( #110988 ), #23660, .T. ) ;
#65372 = EDGE_LOOP ( 'NONE', ( #4731, #61921, #125451, #38658 ) ) ;
#65373 = DIRECTION ( 'NONE',  ( -0.000000000000000000, 1.000000000000000000, -0.000000000000000000 ) ) ;
#65374 = EDGE_CURVE ( 'NONE', #91777, #41716, #98866, .T. ) ;
#65375 = CIRCLE ( 'NONE', #92579, 0.06509327318403745899 ) ;
#65376 = CARTESIAN_POINT ( 'NONE',  ( 11.64999999999990798, 12.50000000000000000, 7.122917578226811486 ) ) ;
#65377 = CARTESIAN_POINT ( 'NONE',  ( -10.85000000000000142, 2.500000000000000000, -2.165063509461097713 ) ) ;
#65378 = ORIENTED_EDGE ( 'NONE', *, *, #10791, .F. ) ;
#65379 = VERTEX_POINT ( 'NONE', #76724 ) ;
#65380 = CARTESIAN_POINT ( 'NONE',  ( 5.649999999999936406, 2.500000000000000000, -6.148780366869526226 ) ) ;
#65381 = EDGE_CURVE ( 'NONE', #78182, #126113, #34134, .T. ) ;
#65383 = EDGE_CURVE ( 'NONE', #59971, #84059, #103082, .T. ) ;
#65382 = VERTEX_POINT ( 'NONE', #125185 ) ;
#65384 = CARTESIAN_POINT ( 'NONE',  ( 13.94999999999989448, 2.500000000000000000, -2.511473670974877948 ) ) ;
#65385 = DIRECTION ( 'NONE',  ( 0.000000000000000000, 1.000000000000000000, 0.000000000000000000 ) ) ;
#65386 = EDGE_LOOP ( 'NONE', ( #78873, #9570, #92639, #105057 ) ) ;
#65387 = LINE ( 'NONE', #6438, #58055 ) ;
#65388 = CARTESIAN_POINT ( 'NONE',  ( -9.200000000000009948, 2.500000000000000000, -4.330127018922197202 ) ) ;
#65389 = CARTESIAN_POINT ( 'NONE',  ( -4.550000000000026468, 12.50000000000000000, -6.495190528383302464 ) ) ;
#65390 = AXIS2_PLACEMENT_3D ( 'NONE', #63498, #112604, #62850 ) ;
#65391 = CARTESIAN_POINT ( 'NONE',  ( 8.749999999999920064, 2.500000000000000000, -2.857883832488653741 ) ) ;
#65392 = AXIS2_PLACEMENT_3D ( 'NONE', #108605, #28774, #7818 ) ;
#65393 = CARTESIAN_POINT ( 'NONE',  ( 6.249999999999930722, 12.50000000000000000, -1.472243186433550122 ) ) ;
#65394 = ORIENTED_EDGE ( 'NONE', *, *, #37784, .F. ) ;
#65395 = EDGE_LOOP ( 'NONE', ( #31144, #32101 ) ) ;
#65396 = CARTESIAN_POINT ( 'NONE',  ( 7.899999999999924860, 2.500000000000000000, -4.330127018922201643 ) ) ;
#65397 = AXIS2_PLACEMENT_3D ( 'NONE', #26684, #96689, #56758 ) ;
#65398 = CARTESIAN_POINT ( 'NONE',  ( 19.09982477502536113, -0.5559300837585569033, 4.454172625795894014 ) ) ;
#65399 = CIRCLE ( 'NONE', #109319, 0.1000000000000002554 ) ;
#65401 = DIRECTION ( 'NONE',  ( -0.000000000000000000, 1.000000000000000000, -0.000000000000000000 ) ) ;
#65400 = VECTOR ( 'NONE', #68987, 1000.000000000000000 ) ;
#65403 = ORIENTED_EDGE ( 'NONE', *, *, #102791, .T. ) ;
#65402 = ORIENTED_EDGE ( 'NONE', *, *, #110090, .F. ) ;
#65404 = VERTEX_POINT ( 'NONE', #56428 ) ;
#65405 = DIRECTION ( 'NONE',  ( 0.000000000000000000, 0.000000000000000000, 1.000000000000000000 ) ) ;
#65406 = DIRECTION ( 'NONE',  ( -0.000000000000000000, -1.000000000000000000, -0.000000000000000000 ) ) ;
#65407 = CIRCLE ( 'NONE', #98852, 0.09999999999999982514 ) ;
#65409 = LINE ( 'NONE', #45792, #110448 ) ;
#65408 = CONICAL_SURFACE ( 'NONE', #84288, 0.1000000000000002554, 0.003490658503988666988 ) ;
#65410 = CIRCLE ( 'NONE', #36190, 0.06509327318403745899 ) ;
#65411 = CARTESIAN_POINT ( 'NONE',  ( 2.899999999999945732, 2.500000000000000000, -4.330127018922201643 ) ) ;
#65412 = CARTESIAN_POINT ( 'NONE',  ( -6.250000000000017764, 2.500000000000000000, 2.857883832488649301 ) ) ;
#65413 = CARTESIAN_POINT ( 'NONE',  ( 184.5000000000000000, 9.429780353434619030E-16, 7.699999999999999289 ) ) ;
#65414 = CIRCLE ( 'NONE', #121758, 0.1000000000000002554 ) ;
#65415 = DIRECTION ( 'NONE',  ( -0.000000000000000000, -1.000000000000000000, -0.000000000000000000 ) ) ;
#65416 = FACE_OUTER_BOUND ( 'NONE', #125707, .T. ) ;
#65417 = AXIS2_PLACEMENT_3D ( 'NONE', #63333, #101333, #111114 ) ;
#65418 = DIRECTION ( 'NONE',  ( -4.274815082592931898E-19, -0.9999939076577903929, -0.003490651415223739937 ) ) ;
#65419 = CIRCLE ( 'NONE', #8886, 0.06509327318403745899 ) ;
#65420 = ORIENTED_EDGE ( 'NONE', *, *, #62783, .F. ) ;
#65421 = EDGE_CURVE ( 'NONE', #65795, #117086, #4864, .T. ) ;
#65422 = ADVANCED_FACE ( 'NONE', ( #68178 ), #6906, .T. ) ;
#65423 = CARTESIAN_POINT ( 'NONE',  ( -0.8000000000000376810, 2.500000000000000000, -4.230127018922201998 ) ) ;
#65424 = VERTEX_POINT ( 'NONE', #116640 ) ;
#65425 = ORIENTED_EDGE ( 'NONE', *, *, #37059, .T. ) ;
#65426 = DIRECTION ( 'NONE',  ( 0.000000000000000000, 0.000000000000000000, 1.000000000000000000 ) ) ;
#65427 = CARTESIAN_POINT ( 'NONE',  ( 8.099999999999923261, 12.50000000000000000, -4.676537180435978769 ) ) ;
#65428 = DIRECTION ( 'NONE',  ( 0.000000000000000000, 0.000000000000000000, 1.000000000000000000 ) ) ;
#65429 = AXIS2_PLACEMENT_3D ( 'NONE', #10580, #39452, #50518 ) ;
#65430 = DIRECTION ( 'NONE',  ( -0.000000000000000000, 1.000000000000000000, -0.000000000000000000 ) ) ;
#65431 = CARTESIAN_POINT ( 'NONE',  ( -10.65000000000000213, 12.50000000000000000, 1.883746621131358934 ) ) ;
#65432 = DIRECTION ( 'NONE',  ( 0.000000000000000000, -0.000000000000000000, 1.000000000000000000 ) ) ;
#65433 = DIRECTION ( 'NONE',  ( 0.000000000000000000, 0.000000000000000000, 1.000000000000000000 ) ) ;
#65434 = ORIENTED_EDGE ( 'NONE', *, *, #78900, .F. ) ;
#65435 = CARTESIAN_POINT ( 'NONE',  ( -1.650000000000034772, 2.500000000000000000, 5.802370205355744659 ) ) ;
#65436 = CIRCLE ( 'NONE', #40328, 0.1000000000000002554 ) ;
#65437 = CARTESIAN_POINT ( 'NONE',  ( -7.100000000000017408, 2.500000000000000000, 0.6928203230275494784 ) ) ;
#65438 = VERTEX_POINT ( 'NONE', #108110 ) ;
#65439 = CONICAL_SURFACE ( 'NONE', #54977, 0.09999999999999982514, 0.003490658503988666988 ) ;
#65440 = ORIENTED_EDGE ( 'NONE', *, *, #101270, .T. ) ;
#65441 = ORIENTED_EDGE ( 'NONE', *, *, #55319, .F. ) ;
#65442 = VERTEX_POINT ( 'NONE', #86538 ) ;
#65443 = CONICAL_SURFACE ( 'NONE', #61263, 0.09999999999999999167, 0.003490658503988666988 ) ;
#65444 = DIRECTION ( 'NONE',  ( 0.000000000000000000, 1.000000000000000000, 0.000000000000000000 ) ) ;
#65445 = DIRECTION ( 'NONE',  ( -0.000000000000000000, -1.000000000000000000, -0.000000000000000000 ) ) ;
#65446 = AXIS2_PLACEMENT_3D ( 'NONE', #45649, #124198, #126780 ) ;
#65447 = AXIS2_PLACEMENT_3D ( 'NONE', #29500, #20324, #81176 ) ;
#65448 = LINE ( 'NONE', #105385, #86136 ) ;
#65449 = CARTESIAN_POINT ( 'NONE',  ( -3.350000000000028955, 12.50000000000000000, -2.165063509461101710 ) ) ;
#65450 = CARTESIAN_POINT ( 'NONE',  ( 10.39999999999991331, 12.50000000000000000, -2.385244779468109755E-15 ) ) ;
#65451 = EDGE_LOOP ( 'NONE', ( #70241, #23678, #66662, #69218 ) ) ;
#65452 = CARTESIAN_POINT ( 'NONE',  ( 2.899999999999946620, 12.50000000000000000, -5.088040615133791356 ) ) ;
#65453 = CARTESIAN_POINT ( 'NONE',  ( -3.749999999999991118, 2.500000000000000000, 2.165063509461097713 ) ) ;
#65454 = CIRCLE ( 'NONE', #42208, 0.1000000000000002554 ) ;
#65455 = DIRECTION ( 'NONE',  ( -0.000000000000000000, 1.000000000000000000, -0.000000000000000000 ) ) ;
#65456 = EDGE_CURVE ( 'NONE', #117955, #30611, #6652, .T. ) ;
#65457 = VERTEX_POINT ( 'NONE', #36811 ) ;
#65458 = CIRCLE ( 'NONE', #94809, 0.06509327318403745899 ) ;
#65459 = CIRCLE ( 'NONE', #55107, 0.1000000000000002554 ) ;
#65460 = AXIS2_PLACEMENT_3D ( 'NONE', #122889, #11635, #50931 ) ;
#65461 = ORIENTED_EDGE ( 'NONE', *, *, #44535, .F. ) ;
#65462 = EDGE_LOOP ( 'NONE', ( #65515, #68371 ) ) ;
#65463 = CARTESIAN_POINT ( 'NONE',  ( -3.750000000000027978, 2.500000000000000000, 7.288010851410849256 ) ) ;
#65464 = CIRCLE ( 'NONE', #52963, 0.06509327318403745899 ) ;
#65465 = CARTESIAN_POINT ( 'NONE',  ( 0.4499999999999569344, 2.500000000000000000, -2.165063509461101710 ) ) ;
#65466 = FACE_OUTER_BOUND ( 'NONE', #74177, .T. ) ;
#65467 = CIRCLE ( 'NONE', #121625, 0.06509327318403745899 ) ;
#65469 = ORIENTED_EDGE ( 'NONE', *, *, #82750, .F. ) ;
#65468 = EDGE_CURVE ( 'NONE', #125450, #120640, #46650, .T. ) ;
#65470 = DIRECTION ( 'NONE',  ( 0.000000000000000000, 0.000000000000000000, 1.000000000000000000 ) ) ;
#65471 = CARTESIAN_POINT ( 'NONE',  ( -9.600000000000006750, 2.500000000000000000, 4.922947341949748257 ) ) ;
#65472 = DIRECTION ( 'NONE',  ( 0.000000000000000000, 1.000000000000000000, 0.000000000000000000 ) ) ;
#65473 = DIRECTION ( 'NONE',  ( -0.000000000000000000, 1.000000000000000000, -0.000000000000000000 ) ) ;
#65474 = EDGE_CURVE ( 'NONE', #60587, #102800, #50855, .T. ) ;
#65475 = CARTESIAN_POINT ( 'NONE',  ( -3.550000000000031797, 12.50000000000000000, -6.148780366869526226 ) ) ;
#65476 = ORIENTED_EDGE ( 'NONE', *, *, #71560, .F. ) ;
#65477 = DIRECTION ( 'NONE',  ( 0.000000000000000000, 0.000000000000000000, 1.000000000000000000 ) ) ;
#65478 = EDGE_LOOP ( 'NONE', ( #65378, #284, #50462, #61048 ) ) ;
#65479 = VERTEX_POINT ( 'NONE', #75422 ) ;
#65480 = CONICAL_SURFACE ( 'NONE', #4837, 0.09999999999999982514, 0.003490658503988666988 ) ;
#65481 = ORIENTED_EDGE ( 'NONE', *, *, #56849, .T. ) ;
#65482 = AXIS2_PLACEMENT_3D ( 'NONE', #40622, #32729, #92928 ) ;
#65483 = EDGE_CURVE ( 'NONE', #17533, #117178, #99509, .T. ) ;
#65484 = DIRECTION ( 'NONE',  ( 0.000000000000000000, 0.000000000000000000, -1.000000000000000000 ) ) ;
#65485 = FACE_BOUND ( 'NONE', #8722, .T. ) ;
#65486 = CARTESIAN_POINT ( 'NONE',  ( 4.599999999999939249, 2.500000000000000000, -3.737306695894649700 ) ) ;
#65487 = FACE_OUTER_BOUND ( 'NONE', #109839, .T. ) ;
#65488 = DIRECTION ( 'NONE',  ( -4.274815082592931898E-19, -0.9999939076577903929, -0.003490651415223739937 ) ) ;
#65489 = AXIS2_PLACEMENT_3D ( 'NONE', #37838, #108510, #116390 ) ;
#65490 = AXIS2_PLACEMENT_3D ( 'NONE', #82697, #102326, #92490 ) ;
#65491 = ORIENTED_EDGE ( 'NONE', *, *, #3758, .T. ) ;
#65492 = DIRECTION ( 'NONE',  ( 0.000000000000000000, 1.000000000000000000, 0.000000000000000000 ) ) ;
#65493 = CARTESIAN_POINT ( 'NONE',  ( 13.74999999999993072, 2.500000000000000000, -2.265063509461101798 ) ) ;
#65494 = DIRECTION ( 'NONE',  ( -0.000000000000000000, -1.000000000000000000, -0.000000000000000000 ) ) ;
#65495 = CARTESIAN_POINT ( 'NONE',  ( 7.099999999999926814, 12.50000000000000000, -0.6928203230275541413 ) ) ;
#65496 = ORIENTED_EDGE ( 'NONE', *, *, #73953, .T. ) ;
#65498 = CARTESIAN_POINT ( 'NONE',  ( 175.5000000000000000, 0.000000000000000000, -2.500000000000000000 ) ) ;
#65497 = AXIS2_PLACEMENT_3D ( 'NONE', #73350, #92343, #23616 ) ;
#65499 = AXIS2_PLACEMENT_3D ( 'NONE', #120631, #88593, #40141 ) ;
#65500 = AXIS2_PLACEMENT_3D ( 'NONE', #122034, #121372, #12065 ) ;
#65501 = FACE_OUTER_BOUND ( 'NONE', #95545, .T. ) ;
#65502 = VECTOR ( 'NONE', #42398, 1000.000000000000000 ) ;
#65503 = VERTEX_POINT ( 'NONE', #57069 ) ;
#65504 = CONICAL_SURFACE ( 'NONE', #44588, 0.1000000000000002554, 0.003490658503988666988 ) ;
#65505 = DIRECTION ( 'NONE',  ( -4.274815082592931898E-19, -0.9999939076577903929, -0.003490651415223739937 ) ) ;
#65506 = ORIENTED_EDGE ( 'NONE', *, *, #39437, .F. ) ;
#65507 = FACE_BOUND ( 'NONE', #70545, .T. ) ;
#65508 = AXIS2_PLACEMENT_3D ( 'NONE', #39406, #41331, #111310 ) ;
#65509 = DIRECTION ( 'NONE',  ( 0.000000000000000000, 0.000000000000000000, -1.000000000000000000 ) ) ;
#65510 = ADVANCED_FACE ( 'NONE', ( #97648 ), #42462, .T. ) ;
#65511 = VERTEX_POINT ( 'NONE', #27600 ) ;
#65512 = CARTESIAN_POINT ( 'NONE',  ( 9.599999999999914380, 12.50000000000000000, 3.637306695894644726 ) ) ;
#65513 = DIRECTION ( 'NONE',  ( 0.000000000000000000, 0.000000000000000000, 1.000000000000000000 ) ) ;
#65514 = EDGE_LOOP ( 'NONE', ( #12394, #115274 ) ) ;
#65515 = ORIENTED_EDGE ( 'NONE', *, *, #116206, .F. ) ;
#65516 = EDGE_CURVE ( 'NONE', #49071, #104330, #97005, .T. ) ;
#65517 = CARTESIAN_POINT ( 'NONE',  ( 185.9635416670080872, -4.367472073101519747, 7.564683531249999149 ) ) ;
#65518 = EDGE_CURVE ( 'NONE', #55213, #23957, #57107, .T. ) ;
#65519 = ORIENTED_EDGE ( 'NONE', *, *, #20204, .F. ) ;
#65520 = CARTESIAN_POINT ( 'NONE',  ( 185.2552083336747444, 6.551208109652275624, -3.782341765624998686 ) ) ;
#65521 = LINE ( 'NONE', #15769, #21932 ) ;
#65522 = FACE_OUTER_BOUND ( 'NONE', #36960, .T. ) ;
#65523 = DIRECTION ( 'NONE',  ( -4.274815082592931898E-19, -0.9999939076577903929, -0.003490651415223739937 ) ) ;
#65524 = ADVANCED_FACE ( 'NONE', ( #95728 ), #127129, .T. ) ;
#65525 = ADVANCED_FACE ( 'NONE', ( #105547 ), #15856, .T. ) ;
#65526 = DIRECTION ( 'NONE',  ( 0.000000000000000000, 1.000000000000000000, 0.000000000000000000 ) ) ;
#65527 = ADVANCED_FACE ( 'NONE', ( #76083 ), #73834, .T. ) ;
#65528 = AXIS2_PLACEMENT_3D ( 'NONE', #112061, #82609, #70201 ) ;
#65529 = AXIS2_PLACEMENT_3D ( 'NONE', #106384, #44904, #65150 ) ;
#65530 = ORIENTED_EDGE ( 'NONE', *, *, #57183, .F. ) ;
#65531 = ORIENTED_EDGE ( 'NONE', *, *, #106005, .F. ) ;
#65532 = FACE_OUTER_BOUND ( 'NONE', #123982, .T. ) ;
#65533 = EDGE_CURVE ( 'NONE', #43052, #74901, #115582, .T. ) ;
#65534 = DIRECTION ( 'NONE',  ( -4.274815082592931898E-19, -0.9999939076577903929, -0.003490651415223739937 ) ) ;
#65535 = CARTESIAN_POINT ( 'NONE',  ( -7.900000000000011013, 2.500000000000000000, 4.330127018922196314 ) ) ;
#65536 = DIRECTION ( 'NONE',  ( -0.000000000000000000, 1.000000000000000000, -0.000000000000000000 ) ) ;
#65538 = VERTEX_POINT ( 'NONE', #118569 ) ;
#65537 = ORIENTED_EDGE ( 'NONE', *, *, #117578, .T. ) ;
#65539 = FACE_BOUND ( 'NONE', #30419, .T. ) ;
#65540 = ORIENTED_EDGE ( 'NONE', *, *, #9480, .F. ) ;
#65541 = CIRCLE ( 'NONE', #67584, 0.06509327318403745899 ) ;
#65542 = DIRECTION ( 'NONE',  ( -0.000000000000000000, -1.000000000000000000, -0.000000000000000000 ) ) ;
#65543 = DIRECTION ( 'NONE',  ( 0.000000000000000000, -0.9999939076577903929, 0.003490651415223739937 ) ) ;
#65544 = AXIS2_PLACEMENT_3D ( 'NONE', #51455, #100525, #2312 ) ;
#65545 = EDGE_CURVE ( 'NONE', #72858, #102123, #28928, .T. ) ;
#65546 = ORIENTED_EDGE ( 'NONE', *, *, #58044, .F. ) ;
#65547 = PLANE ( 'NONE',  #24210 ) ;
#65548 = DIRECTION ( 'NONE',  ( -4.274815082592931898E-19, -0.9999939076577903929, -0.003490651415223739937 ) ) ;
#65549 = AXIS2_PLACEMENT_3D ( 'NONE', #68528, #58084, #106045 ) ;
#65550 = LINE ( 'NONE', #123813, #22136 ) ;
#65551 = DIRECTION ( 'NONE',  ( 0.000000000000000000, 0.000000000000000000, -1.000000000000000000 ) ) ;
#65552 = DIRECTION ( 'NONE',  ( -0.000000000000000000, 1.000000000000000000, -0.000000000000000000 ) ) ;
#65553 = CARTESIAN_POINT ( 'NONE',  ( -9.550000000000002487, 2.500000000000000000, 6.495190528383297135 ) ) ;
#65554 = CARTESIAN_POINT ( 'NONE',  ( 186.3593750003414016, 0.000000000000000000, 7.564683531250000925 ) ) ;
#65555 = FACE_OUTER_BOUND ( 'NONE', #63706, .T. ) ;
#65556 = DIRECTION ( 'NONE',  ( 0.000000000000000000, 1.000000000000000000, 0.000000000000000000 ) ) ;
#65557 = EDGE_LOOP ( 'NONE', ( #55635, #80282 ) ) ;
#65558 = ORIENTED_EDGE ( 'NONE', *, *, #43878, .F. ) ;
#65559 = CARTESIAN_POINT ( 'NONE',  ( -12.49999999999999289, 2.500000000000000000, 3.537306695894645081 ) ) ;
#65561 = EDGE_LOOP ( 'NONE', ( #86771, #28666, #33601, #92035 ) ) ;
#65560 = AXIS2_PLACEMENT_3D ( 'NONE', #963, #40923, #80829 ) ;
#65562 = CONICAL_SURFACE ( 'NONE', #113687, 0.1000000000000002554, 0.003490658503988666988 ) ;
#65563 = DIRECTION ( 'NONE',  ( 0.000000000000000000, -0.9999939076577903929, 0.003490651415223739937 ) ) ;
#65565 = VERTEX_POINT ( 'NONE', #728 ) ;
#65564 = VERTEX_POINT ( 'NONE', #120518 ) ;
#65566 = EDGE_LOOP ( 'NONE', ( #42195, #105537 ) ) ;
#65567 = AXIS2_PLACEMENT_3D ( 'NONE', #28516, #118819, #108348 ) ;
#65568 = CARTESIAN_POINT ( 'NONE',  ( 12.09999999999990550, 12.50000000000000000, 5.022947341949748790 ) ) ;
#65569 = CONICAL_SURFACE ( 'NONE', #88544, 0.09999999999999982514, 0.003490658503988666988 ) ;
#65570 = PLANE ( 'NONE',  #853 ) ;
#65571 = CARTESIAN_POINT ( 'NONE',  ( 5.599999999999931255, 2.500000000000000000, 4.676537180435972552 ) ) ;
#65572 = DIRECTION ( 'NONE',  ( 0.000000000000000000, 0.000000000000000000, 1.000000000000000000 ) ) ;
#65573 = PLANE ( 'NONE',  #12031 ) ;
#65574 = ORIENTED_EDGE ( 'NONE', *, *, #102644, .T. ) ;
#65575 = DIRECTION ( 'NONE',  ( -0.000000000000000000, -1.000000000000000000, -0.000000000000000000 ) ) ;
#65576 = ORIENTED_EDGE ( 'NONE', *, *, #101620, .F. ) ;
#65577 = VERTEX_POINT ( 'NONE', #48559 ) ;
#65578 = ORIENTED_EDGE ( 'NONE', *, *, #87524, .T. ) ;
#65579 = EDGE_CURVE ( 'NONE', #93847, #87716, #75889, .T. ) ;
#65580 = VERTEX_POINT ( 'NONE', #81241 ) ;
#65581 = DIRECTION ( 'NONE',  ( 0.000000000000000000, 0.000000000000000000, -1.000000000000000000 ) ) ;
#65582 = AXIS2_PLACEMENT_3D ( 'NONE', #51602, #33870, #31959 ) ;
#65583 = CIRCLE ( 'NONE', #9150, 0.1000000000000002554 ) ;
#65584 = ORIENTED_EDGE ( 'NONE', *, *, #66726, .F. ) ;
#65585 = ORIENTED_EDGE ( 'NONE', *, *, #73783, .T. ) ;
#65586 = FACE_OUTER_BOUND ( 'NONE', #61873, .T. ) ;
#65587 = ADVANCED_FACE ( 'NONE', ( #30864 ), #109398, .T. ) ;
#65588 = CARTESIAN_POINT ( 'NONE',  ( 0.6499999999999561684, 2.500000000000000000, 1.918653347947321564 ) ) ;
#65589 = CIRCLE ( 'NONE', #111559, 0.06509327318403745899 ) ;
#65590 = FACE_OUTER_BOUND ( 'NONE', #20786, .T. ) ;
#65592 = DIRECTION ( 'NONE',  ( 0.000000000000000000, 0.000000000000000000, 1.000000000000000000 ) ) ;
#65591 = CIRCLE ( 'NONE', #124177, 0.1000000000000000472 ) ;
#65593 = CARTESIAN_POINT ( 'NONE',  ( -4.800000000000028244, 12.50000000000000000, -4.048810130592463530 ) ) ;
#65594 = AXIS2_PLACEMENT_3D ( 'NONE', #109399, #97006, #98285 ) ;
#65595 = CARTESIAN_POINT ( 'NONE',  ( -1.450000000000035927, 2.500000000000000000, -1.918653347947326004 ) ) ;
#65596 = ORIENTED_EDGE ( 'NONE', *, *, #39230, .T. ) ;
#65597 = DIRECTION ( 'NONE',  ( 0.000000000000000000, 0.000000000000000000, -1.000000000000000000 ) ) ;
#65598 = VECTOR ( 'NONE', #3189, 1000.000000000000000 ) ;
#65600 = ORIENTED_EDGE ( 'NONE', *, *, #113424, .F. ) ;
#65599 = CIRCLE ( 'NONE', #25893, 0.1000000000000000472 ) ;
#65601 = DIRECTION ( 'NONE',  ( -4.274815082592931898E-19, -0.9999939076577903929, -0.003490651415223739937 ) ) ;
#65602 = EDGE_LOOP ( 'NONE', ( #92384, #29594 ) ) ;
#65603 = PLANE ( 'NONE',  #104643 ) ;
#65604 = ORIENTED_EDGE ( 'NONE', *, *, #15385, .T. ) ;
#65605 = AXIS2_PLACEMENT_3D ( 'NONE', #79300, #40016, #60928 ) ;
#65606 = ORIENTED_EDGE ( 'NONE', *, *, #50425, .T. ) ;
#65607 = CARTESIAN_POINT ( 'NONE',  ( -0.8500000000000386136, 2.500000000000000000, 2.757883832488649656 ) ) ;
#65608 = DIRECTION ( 'NONE',  ( 0.000000000000000000, 0.000000000000000000, -1.000000000000000000 ) ) ;
#65609 = DIRECTION ( 'NONE',  ( 0.000000000000000000, 0.000000000000000000, 1.000000000000000000 ) ) ;
#65610 = CARTESIAN_POINT ( 'NONE',  ( -13.14999999999999147, 2.500000000000000000, 2.511473670974877503 ) ) ;
#65611 = CARTESIAN_POINT ( 'NONE',  ( -13.29999999999999005, 2.500000000000000000, -4.430127018922199511 ) ) ;
#65612 = ORIENTED_EDGE ( 'NONE', *, *, #28602, .T. ) ;
#65613 = CARTESIAN_POINT ( 'NONE',  ( -1.250000000000035749, 2.500000000000000000, -2.957883832488653830 ) ) ;
#65614 = CARTESIAN_POINT ( 'NONE',  ( 6.049999999999934097, 2.500000000000000000, -2.511473670974877948 ) ) ;
#65615 = FACE_OUTER_BOUND ( 'NONE', #41756, .T. ) ;
#65616 = DIRECTION ( 'NONE',  ( 0.000000000000000000, 0.000000000000000000, -1.000000000000000000 ) ) ;
#65617 = AXIS2_PLACEMENT_3D ( 'NONE', #129117, #108788, #8645 ) ;
#65618 = CARTESIAN_POINT ( 'NONE',  ( -10.40000000000000213, 2.500000000000000000, 4.330127018922196314 ) ) ;
#65619 = ADVANCED_FACE ( 'NONE', ( #59019 ), #666, .T. ) ;
#65620 = EDGE_LOOP ( 'NONE', ( #35308, #67285 ) ) ;
#65621 = EDGE_LOOP ( 'NONE', ( #67465, #84148 ) ) ;
#65622 = ORIENTED_EDGE ( 'NONE', *, *, #64965, .T. ) ;
#65623 = AXIS2_PLACEMENT_3D ( 'NONE', #13188, #95001, #115915 ) ;
#65624 = DIRECTION ( 'NONE',  ( -0.000000000000000000, 1.000000000000000000, -0.000000000000000000 ) ) ;
#65626 = EDGE_CURVE ( 'NONE', #32850, #56986, #82159, .T. ) ;
#65625 = DIRECTION ( 'NONE',  ( 0.000000000000000000, 0.000000000000000000, -1.000000000000000000 ) ) ;
#65627 = CIRCLE ( 'NONE', #99094, 0.06509327318403743123 ) ;
#65628 = EDGE_CURVE ( 'NONE', #35861, #121566, #119223, .T. ) ;
#65629 = CARTESIAN_POINT ( 'NONE',  ( 187.3750000000000000, 8.891194145520236347, 5.444286225454521982E-16 ) ) ;
#65630 = PLANE ( 'NONE',  #92892 ) ;
#65631 = CARTESIAN_POINT ( 'NONE',  ( -9.200000000000006395, 12.50000000000000000, -0.06509327318403980434 ) ) ;
#65632 = DIRECTION ( 'NONE',  ( 0.000000000000000000, 1.000000000000000000, 0.000000000000000000 ) ) ;
#65633 = EDGE_CURVE ( 'NONE', #73190, #60441, #21677, .T. ) ;
#65634 = DIRECTION ( 'NONE',  ( -1.000000000000000000, -0.000000000000000000, -0.000000000000000000 ) ) ;
#65635 = ORIENTED_EDGE ( 'NONE', *, *, #46632, .T. ) ;
#65636 = AXIS2_PLACEMENT_3D ( 'NONE', #15966, #44154, #83454 ) ;
#65637 = VECTOR ( 'NONE', #20730, 1000.000000000000000 ) ;
#65638 = DIRECTION ( 'NONE',  ( 0.000000000000000000, 0.000000000000000000, -1.000000000000000000 ) ) ;
#65639 = CARTESIAN_POINT ( 'NONE',  ( 8.099999999999923261, 2.500000000000000000, 4.776537180435972196 ) ) ;
#65640 = EDGE_CURVE ( 'NONE', #7221, #36118, #92619, .T. ) ;
#65641 = ORIENTED_EDGE ( 'NONE', *, *, #110875, .F. ) ;
#65642 = EDGE_CURVE ( 'NONE', #74504, #59695, #27867, .T. ) ;
#65643 = DIRECTION ( 'NONE',  ( 0.000000000000000000, 1.000000000000000000, 0.000000000000000000 ) ) ;
#65644 = DIRECTION ( 'NONE',  ( 0.000000000000000000, 0.000000000000000000, -1.000000000000000000 ) ) ;
#65645 = DIRECTION ( 'NONE',  ( 0.000000000000000000, 0.000000000000000000, 1.000000000000000000 ) ) ;
#65646 = ORIENTED_EDGE ( 'NONE', *, *, #76209, .F. ) ;
#65647 = VECTOR ( 'NONE', #28323, 1000.000000000000000 ) ;
#65648 = AXIS2_PLACEMENT_3D ( 'NONE', #33994, #32724, #73911 ) ;
#65649 = LINE ( 'NONE', #28313, #59450 ) ;
#65650 = B_SPLINE_CURVE_WITH_KNOTS ( 'NONE', 3,
 ( #4364, #84232, #34524, #113712, #124824, #52856, #2444, #44981, #52217, #24048 ),
 .UNSPECIFIED., .F., .F.,
 ( 4, 2, 2, 2, 4 ),
 ( 1.339801017408199283E-15, 0.001880205780637580646, 0.003760411561273821219, 0.005640617341910062442, 0.007520823122546303231 ),
 .UNSPECIFIED. ) ;
#65652 = ORIENTED_EDGE ( 'NONE', *, *, #85886, .T. ) ;
#65651 = AXIS2_PLACEMENT_3D ( 'NONE', #75505, #105631, #74879 ) ;
#65653 = LINE ( 'NONE', #96388, #73053 ) ;
#65654 = DIRECTION ( 'NONE',  ( 0.000000000000000000, -0.9999939076577903929, 0.003490651415223739937 ) ) ;
#65655 = VERTEX_POINT ( 'NONE', #70768 ) ;
#65656 = DIRECTION ( 'NONE',  ( 0.000000000000000000, 1.000000000000000000, 0.000000000000000000 ) ) ;
#65657 = CARTESIAN_POINT ( 'NONE',  ( -2.950000000000030376, 2.500000000000000000, 6.495190528383297135 ) ) ;
#65658 = ORIENTED_EDGE ( 'NONE', *, *, #108769, .F. ) ;
#65659 = CARTESIAN_POINT ( 'NONE',  ( -5.850000000000018296, 2.500000000000000000, 7.088010851410848190 ) ) ;
#65660 = ORIENTED_EDGE ( 'NONE', *, *, #15713, .T. ) ;
#65661 = ORIENTED_EDGE ( 'NONE', *, *, #95416, .F. ) ;
#65662 = CARTESIAN_POINT ( 'NONE',  ( 3.749999999999940492, 2.500000000000000000, 2.957883832488649389 ) ) ;
#65663 = CARTESIAN_POINT ( 'NONE',  ( 11.84999999999990372, 2.500000000000000000, 1.918653347947321564 ) ) ;
#65664 = AXIS2_PLACEMENT_3D ( 'NONE', #35829, #14861, #94737 ) ;
#65665 = AXIS2_PLACEMENT_3D ( 'NONE', #99895, #10220, #90052 ) ;
#65666 = VERTEX_POINT ( 'NONE', #110684 ) ;
#65667 = DIRECTION ( 'NONE',  ( 0.000000000000000000, 1.000000000000000000, 0.000000000000000000 ) ) ;
#65668 = DIRECTION ( 'NONE',  ( 0.000000000000000000, 0.000000000000000000, -1.000000000000000000 ) ) ;
#65669 = ORIENTED_EDGE ( 'NONE', *, *, #16984, .F. ) ;
#65670 = EDGE_CURVE ( 'NONE', #126920, #56076, #78041, .T. ) ;
#65671 = CARTESIAN_POINT ( 'NONE',  ( 8.149999999999923972, 2.500000000000000000, 1.818653347947321475 ) ) ;
#65672 = DIRECTION ( 'NONE',  ( 0.000000000000000000, 0.000000000000000000, -1.000000000000000000 ) ) ;
#65673 = CIRCLE ( 'NONE', #88668, 0.09999999999999982514 ) ;
#65674 = VECTOR ( 'NONE', #111067, 1000.000000000000000 ) ;
#65675 = CIRCLE ( 'NONE', #99054, 0.06509327318403745899 ) ;
#65676 = EDGE_CURVE ( 'NONE', #24152, #79929, #21606, .T. ) ;
#65677 = DIRECTION ( 'NONE',  ( 0.000000000000000000, -0.000000000000000000, 1.000000000000000000 ) ) ;
#65678 = LINE ( 'NONE', #125878, #78057 ) ;
#65679 = ADVANCED_FACE ( 'NONE', ( #40030 ), #48812, .T. ) ;
#65680 = CARTESIAN_POINT ( 'NONE',  ( 13.14999999999989733, 2.500000000000000000, -2.411473670974877859 ) ) ;
#65681 = DIRECTION ( 'NONE',  ( 0.000000000000000000, 0.000000000000000000, -1.000000000000000000 ) ) ;
#65682 = EDGE_CURVE ( 'NONE', #77485, #59628, #9082, .T. ) ;
#65683 = EDGE_CURVE ( 'NONE', #63939, #7340, #8977, .T. ) ;
#65684 = CIRCLE ( 'NONE', #11401, 0.06509327318403745899 ) ;
#65685 = AXIS2_PLACEMENT_3D ( 'NONE', #40094, #57804, #80011 ) ;
#65686 = VERTEX_POINT ( 'NONE', #88460 ) ;
#65687 = VERTEX_POINT ( 'NONE', #128429 ) ;
#65689 = ORIENTED_EDGE ( 'NONE', *, *, #25472, .T. ) ;
#65688 = EDGE_CURVE ( 'NONE', #91704, #41081, #38763, .T. ) ;
#65690 = VERTEX_POINT ( 'NONE', #4570 ) ;
#65691 = CARTESIAN_POINT ( 'NONE',  ( 4.599999999999936584, 12.50000000000000000, 4.265033745738159077 ) ) ;
#65692 = CARTESIAN_POINT ( 'NONE',  ( -7.100000000000017408, 2.500000000000000000, 0.6928203230275494784 ) ) ;
#65693 = CIRCLE ( 'NONE', #120086, 0.1000000000000002554 ) ;
#65694 = CARTESIAN_POINT ( 'NONE',  ( 9.999999999999911182, 2.500000000000000000, -3.637306695894650055 ) ) ;
#65695 = EDGE_LOOP ( 'NONE', ( #73721, #1416 ) ) ;
#65696 = FACE_BOUND ( 'NONE', #113856, .T. ) ;
#65697 = LINE ( 'NONE', #85966, #96009 ) ;
#65698 = FACE_OUTER_BOUND ( 'NONE', #110980, .T. ) ;
#65699 = EDGE_CURVE ( 'NONE', #12208, #21956, #102789, .T. ) ;
#65700 = DIRECTION ( 'NONE',  ( -0.000000000000000000, 1.000000000000000000, -0.000000000000000000 ) ) ;
#65701 = EDGE_CURVE ( 'NONE', #49033, #34747, #81861, .T. ) ;
#65702 = FACE_OUTER_BOUND ( 'NONE', #58367, .T. ) ;
#65703 = CARTESIAN_POINT ( 'NONE',  ( 0.6499999999999566125, 2.500000000000000000, -6.048780366869526581 ) ) ;
#65704 = CARTESIAN_POINT ( 'NONE',  ( -0.4500000000000402012, 2.500000000000000000, 6.495190528383297135 ) ) ;
#65705 = FACE_OUTER_BOUND ( 'NONE', #118834, .T. ) ;
#65706 = DIRECTION ( 'NONE',  ( 0.000000000000000000, 0.000000000000000000, 1.000000000000000000 ) ) ;
#65707 = CARTESIAN_POINT ( 'NONE',  ( 6.449999999999930012, 2.500000000000000000, 6.841600689897072485 ) ) ;
#65708 = CIRCLE ( 'NONE', #117935, 0.1000000000000000472 ) ;
#65709 = CARTESIAN_POINT ( 'NONE',  ( -7.900000000000014566, 12.50000000000000000, -3.702399969078687292 ) ) ;
#65710 = EDGE_LOOP ( 'NONE', ( #1328, #61412 ) ) ;
#65711 = VERTEX_POINT ( 'NONE', #34076 ) ;
#65712 = ORIENTED_EDGE ( 'NONE', *, *, #26804, .T. ) ;
#65713 = EDGE_LOOP ( 'NONE', ( #89784, #117437, #60032, #98612 ) ) ;
#65714 = CARTESIAN_POINT ( 'NONE',  ( -9.150000000000009237, 12.50000000000000000, -2.165063509461101710 ) ) ;
#65715 = VERTEX_POINT ( 'NONE', #124389 ) ;
#65716 = FACE_OUTER_BOUND ( 'NONE', #18734, .T. ) ;
#65717 = ORIENTED_EDGE ( 'NONE', *, *, #71860, .T. ) ;
#65718 = EDGE_CURVE ( 'NONE', #107053, #63043, #456, .T. ) ;
#65719 = ORIENTED_EDGE ( 'NONE', *, *, #7723, .T. ) ;
#65720 = CARTESIAN_POINT ( 'NONE',  ( -5.850000000000021849, 2.500000000000000000, -2.857883832488653741 ) ) ;
#65721 = VECTOR ( 'NONE', #51680, 1000.000000000000000 ) ;
#65722 = FACE_OUTER_BOUND ( 'NONE', #100672, .T. ) ;
#65723 = CARTESIAN_POINT ( 'NONE',  ( -10.00000000000000533, 2.500000000000000000, 5.122947341949749323 ) ) ;
#65724 = DIRECTION ( 'NONE',  ( 0.000000000000000000, 0.000000000000000000, -1.000000000000000000 ) ) ;
#65725 = FACE_OUTER_BOUND ( 'NONE', #88962, .T. ) ;
#65726 = ORIENTED_EDGE ( 'NONE', *, *, #17925, .T. ) ;
#65727 = ORIENTED_EDGE ( 'NONE', *, *, #52677, .T. ) ;
#65728 = CIRCLE ( 'NONE', #67785, 0.06509327318403745899 ) ;
#65729 = ORIENTED_EDGE ( 'NONE', *, *, #118604, .F. ) ;
#65730 = EDGE_LOOP ( 'NONE', ( #75130, #53837 ) ) ;
#65731 = DIRECTION ( 'NONE',  ( -0.000000000000000000, 1.000000000000000000, -0.000000000000000000 ) ) ;
#65732 = EDGE_LOOP ( 'NONE', ( #29905, #19041 ) ) ;
#65733 = ORIENTED_EDGE ( 'NONE', *, *, #50090, .F. ) ;
#65734 = DIRECTION ( 'NONE',  ( 0.000000000000000000, 0.000000000000000000, 1.000000000000000000 ) ) ;
#65735 = EDGE_CURVE ( 'NONE', #108831, #53510, #50658, .T. ) ;
#65737 = CIRCLE ( 'NONE', #74060, 0.06509327318403745899 ) ;
#65736 = DIRECTION ( 'NONE',  ( -1.000000000000000000, 0.000000000000000000, 0.000000000000000000 ) ) ;
#65738 = DIRECTION ( 'NONE',  ( 0.000000000000000000, -0.000000000000000000, 1.000000000000000000 ) ) ;
#65739 = VECTOR ( 'NONE', #76971, 1000.000000000000000 ) ;
#65740 = DIRECTION ( 'NONE',  ( -0.000000000000000000, 1.000000000000000000, -0.000000000000000000 ) ) ;
#65741 = DIRECTION ( 'NONE',  ( 0.000000000000000000, -0.9999939076577903929, 0.003490651415223739937 ) ) ;
#65742 = DIRECTION ( 'NONE',  ( 0.000000000000000000, 1.000000000000000000, -1.224646799147353207E-16 ) ) ;
#65743 = ORIENTED_EDGE ( 'NONE', *, *, #86142, .T. ) ;
#65744 = AXIS2_PLACEMENT_3D ( 'NONE', #75016, #26560, #95940 ) ;
#65745 = FACE_OUTER_BOUND ( 'NONE', #68572, .T. ) ;
#65746 = ORIENTED_EDGE ( 'NONE', *, *, #91933, .F. ) ;
#65747 = DIRECTION ( 'NONE',  ( 0.000000000000000000, 0.000000000000000000, 1.000000000000000000 ) ) ;
#65748 = ORIENTED_EDGE ( 'NONE', *, *, #49141, .F. ) ;
#65749 = DIRECTION ( 'NONE',  ( 0.000000000000000000, -0.000000000000000000, 1.000000000000000000 ) ) ;
#65750 = CARTESIAN_POINT ( 'NONE',  ( 11.64999999999990798, 12.50000000000000000, -2.857883832488653741 ) ) ;
#65751 = ORIENTED_EDGE ( 'NONE', *, *, #34227, .T. ) ;
#65752 = DIRECTION ( 'NONE',  ( -0.000000000000000000, -1.000000000000000000, -0.000000000000000000 ) ) ;
#65753 = CARTESIAN_POINT ( 'NONE',  ( -1.850000000000033396, 2.500000000000000000, -1.818653347947325916 ) ) ;
#65754 = ORIENTED_EDGE ( 'NONE', *, *, #80592, .F. ) ;
#65755 = DIRECTION ( 'NONE',  ( 0.000000000000000000, 0.000000000000000000, 1.000000000000000000 ) ) ;
#65757 = DIRECTION ( 'NONE',  ( 0.000000000000000000, 1.000000000000000000, 0.000000000000000000 ) ) ;
#65756 = AXIS2_PLACEMENT_3D ( 'NONE', #89437, #48224, #129395 ) ;
#65758 = EDGE_LOOP ( 'NONE', ( #81921, #69246, #44149, #12260 ) ) ;
#65759 = CONICAL_SURFACE ( 'NONE', #17727, 0.1000000000000002554, 0.003490658503988666988 ) ;
#65760 = CIRCLE ( 'NONE', #51207, 0.09999999999999982514 ) ;
#65761 = ORIENTED_EDGE ( 'NONE', *, *, #67403, .F. ) ;
#65762 = DIRECTION ( 'NONE',  ( 0.000000000000000000, -0.9999939076577903929, 0.003490651415223739937 ) ) ;
#65763 = CARTESIAN_POINT ( 'NONE',  ( -3.950000000000024603, 2.500000000000000000, -2.611473670974877592 ) ) ;
#65764 = CARTESIAN_POINT ( 'NONE',  ( 187.2968750003414300, 8.734944146203032389, 5.348610694689227483E-16 ) ) ;
#65765 = CARTESIAN_POINT ( 'NONE',  ( 0.000000000000000000, 0.000000000000000000, 6.000000000000005329 ) ) ;
#65766 = CIRCLE ( 'NONE', #9339, 0.06509327318403745899 ) ;
#65767 = CARTESIAN_POINT ( 'NONE',  ( 12.09999999999990550, 12.50000000000000000, -5.088040615133791356 ) ) ;
#65768 = CIRCLE ( 'NONE', #95308, 0.06509327318403743123 ) ;
#65769 = CIRCLE ( 'NONE', #76155, 0.09999999999999982514 ) ;
#65770 = DIRECTION ( 'NONE',  ( 0.000000000000000000, 0.000000000000000000, 1.000000000000000000 ) ) ;
#65771 = VECTOR ( 'NONE', #69982, 1000.000000000000000 ) ;
#65772 = EDGE_CURVE ( 'NONE', #65023, #14140, #73628, .T. ) ;
#65773 = EDGE_LOOP ( 'NONE', ( #104865, #92647 ) ) ;
#65774 = VECTOR ( 'NONE', #84920, 1000.000000000000000 ) ;
#65775 = CARTESIAN_POINT ( 'NONE',  ( 76.44832593087598127, 3.583109180387994641, -6.086770968619237721 ) ) ;
#65777 = ADVANCED_FACE ( 'NONE', ( #111991 ), #6705, .T. ) ;
#65776 = AXIS2_PLACEMENT_3D ( 'NONE', #110604, #2561, #32068 ) ;
#65778 = ORIENTED_EDGE ( 'NONE', *, *, #68618, .F. ) ;
#65779 = CIRCLE ( 'NONE', #122239, 3.000000000000000000 ) ;
#65780 = EDGE_CURVE ( 'NONE', #115619, #48060, #115682, .T. ) ;
#65781 = DIRECTION ( 'NONE',  ( 0.000000000000000000, -0.9999939076577903929, 0.003490651415223739937 ) ) ;
#65782 = DIRECTION ( 'NONE',  ( -0.000000000000000000, -0.000000000000000000, -1.000000000000000000 ) ) ;
#65783 = CARTESIAN_POINT ( 'NONE',  ( 5.599999999999931255, 2.500000000000000000, 4.576537180435972019 ) ) ;
#65784 = EDGE_CURVE ( 'NONE', #31107, #57789, #111184, .T. ) ;
#65785 = ORIENTED_EDGE ( 'NONE', *, *, #28178, .F. ) ;
#65786 = DIRECTION ( 'NONE',  ( -0.000000000000000000, 1.000000000000000000, -0.000000000000000000 ) ) ;
#65787 = CARTESIAN_POINT ( 'NONE',  ( 6.249999999999967137, 2.500000000000000000, 6.395190528383296602 ) ) ;
#65788 = EDGE_CURVE ( 'NONE', #59434, #74772, #98665, .T. ) ;
#65789 = EDGE_CURVE ( 'NONE', #103313, #62839, #74631, .T. ) ;
#65790 = EDGE_CURVE ( 'NONE', #75929, #126716, #109124, .T. ) ;
#65791 = EDGE_CURVE ( 'NONE', #20224, #116295, #92710, .T. ) ;
#65792 = VERTEX_POINT ( 'NONE', #24248 ) ;
#65793 = CARTESIAN_POINT ( 'NONE',  ( 5.849999999999933920, 2.500000000000000000, 5.802370205355744659 ) ) ;
#65794 = ORIENTED_EDGE ( 'NONE', *, *, #99411, .T. ) ;
#65795 = VERTEX_POINT ( 'NONE', #53066 ) ;
#65796 = CARTESIAN_POINT ( 'NONE',  ( -4.600000000000024514, 2.500000000000000000, 0.6928203230275494784 ) ) ;
#65797 = EDGE_CURVE ( 'NONE', #39483, #36299, #92997, .T. ) ;
#65798 = ORIENTED_EDGE ( 'NONE', *, *, #118861, .T. ) ;
#65799 = DIRECTION ( 'NONE',  ( 0.000000000000000000, -0.9999939076577903929, 0.003490651415223739937 ) ) ;
#65800 = CARTESIAN_POINT ( 'NONE',  ( -8.350000000000008527, 2.500000000000000000, 7.288010851410849256 ) ) ;
#65801 = CIRCLE ( 'NONE', #86737, 0.1000000000000002554 ) ;
#65802 = CARTESIAN_POINT ( 'NONE',  ( -7.500000000000001776, 2.500000000000000000, 1.734723475976807094E-15 ) ) ;
#65803 = AXIS2_PLACEMENT_3D ( 'NONE', #1117, #71146, #31243 ) ;
#65804 = ORIENTED_EDGE ( 'NONE', *, *, #128347, .T. ) ;
#65805 = FACE_BOUND ( 'NONE', #90017, .T. ) ;
#65807 = VERTEX_POINT ( 'NONE', #103457 ) ;
#65806 = DIRECTION ( 'NONE',  ( -0.000000000000000000, -1.000000000000000000, -0.000000000000000000 ) ) ;
#65808 = CARTESIAN_POINT ( 'NONE',  ( 175.5000000000000000, 0.000000000000000000, 2.000000000000000000 ) ) ;
#65809 = CARTESIAN_POINT ( 'NONE',  ( 1.649999999999951061, 2.500000000000000000, -6.595190528383302109 ) ) ;
#65810 = EDGE_LOOP ( 'NONE', ( #10655, #52644, #112805, #34401 ) ) ;
#65811 = AXIS2_PLACEMENT_3D ( 'NONE', #87851, #38126, #117962 ) ;
#65812 = ORIENTED_EDGE ( 'NONE', *, *, #106401, .T. ) ;
#65813 = CONICAL_SURFACE ( 'NONE', #9407, 0.1000000000000002554, 0.003490658503988666988 ) ;
#65814 = EDGE_LOOP ( 'NONE', ( #93252, #37701, #43753, #67512 ) ) ;
#65815 = CARTESIAN_POINT ( 'NONE',  ( -8.550000000000014921, 2.500000000000000000, -6.148780366869520897 ) ) ;
#65816 = CARTESIAN_POINT ( 'NONE',  ( 4.849235612604186230, 2.499999999999999112, 8.943930330504295867 ) ) ;
#65817 = DIRECTION ( 'NONE',  ( 0.000000000000000000, 0.000000000000000000, 1.000000000000000000 ) ) ;
#65818 = EDGE_CURVE ( 'NONE', #117733, #102950, #38050, .T. ) ;
#65819 = FACE_BOUND ( 'NONE', #30590, .T. ) ;
#65820 = ORIENTED_EDGE ( 'NONE', *, *, #17935, .T. ) ;
#65821 = CARTESIAN_POINT ( 'NONE',  ( 186.1093750003413732, 9.264065473108010111E-16, -7.564683531250000925 ) ) ;
#65822 = CARTESIAN_POINT ( 'NONE',  ( 6.849999999999929479, 2.500000000000000000, -1.818653347947326138 ) ) ;
#65823 = DIRECTION ( 'NONE',  ( 0.000000000000000000, -0.9999939076577903929, 0.003490651415223739937 ) ) ;
#65825 = CONICAL_SURFACE ( 'NONE', #21945, 0.09999999999999982514, 0.003490658503988666988 ) ;
#65824 = DIRECTION ( 'NONE',  ( 0.000000000000000000, 1.000000000000000000, 0.000000000000000000 ) ) ;
#65826 = VECTOR ( 'NONE', #122693, 1000.000000000000000 ) ;
#65827 = LINE ( 'NONE', #6248, #69504 ) ;
#65828 = CARTESIAN_POINT ( 'NONE',  ( -7.700000000000010836, 2.500000000000000000, 4.083716857408421497 ) ) ;
#65829 = EDGE_CURVE ( 'NONE', #240, #59971, #29728, .T. ) ;
#65830 = DIRECTION ( 'NONE',  ( 0.000000000000000000, -0.000000000000000000, 1.000000000000000000 ) ) ;
#65831 = DIRECTION ( 'NONE',  ( -0.000000000000000000, -1.000000000000000000, -0.000000000000000000 ) ) ;
#65832 = EDGE_CURVE ( 'NONE', #109827, #84019, #2827, .T. ) ;
#65833 = DIRECTION ( 'NONE',  ( 0.000000000000000000, 1.000000000000000000, 0.000000000000000000 ) ) ;
#65834 = EDGE_CURVE ( 'NONE', #1184, #12403, #75681, .T. ) ;
#65835 = ORIENTED_EDGE ( 'NONE', *, *, #47010, .F. ) ;
#65836 = ORIENTED_EDGE ( 'NONE', *, *, #68744, .T. ) ;
#65837 = ORIENTED_EDGE ( 'NONE', *, *, #38903, .F. ) ;
#65838 = ORIENTED_EDGE ( 'NONE', *, *, #45035, .T. ) ;
#65839 = ORIENTED_EDGE ( 'NONE', *, *, #35063, .F. ) ;
#65840 = LINE ( 'NONE', #36411, #4569 ) ;
#65841 = LINE ( 'NONE', #16722, #88542 ) ;
#65843 = EDGE_CURVE ( 'NONE', #121535, #60091, #107076, .T. ) ;
#65842 = EDGE_LOOP ( 'NONE', ( #99702, #80801, #82707, #86091 ) ) ;
#65844 = FACE_BOUND ( 'NONE', #117063, .T. ) ;
#65845 = AXIS2_PLACEMENT_3D ( 'NONE', #60910, #92299, #2620 ) ;
#65846 = DIRECTION ( 'NONE',  ( -0.000000000000000000, 1.000000000000000000, -0.000000000000000000 ) ) ;
#65847 = EDGE_CURVE ( 'NONE', #4275, #42483, #2651, .T. ) ;
#65848 = EDGE_CURVE ( 'NONE', #63445, #74853, #67346, .T. ) ;
#65849 = EDGE_CURVE ( 'NONE', #51178, #90407, #42259, .T. ) ;
#65850 = CONICAL_SURFACE ( 'NONE', #120244, 0.1000000000000002554, 0.003490658503988666988 ) ;
#65851 = DIRECTION ( 'NONE',  ( 0.000000000000000000, 1.000000000000000000, 0.000000000000000000 ) ) ;
#65852 = VECTOR ( 'NONE', #7491, 1000.000000000000000 ) ;
#65853 = CIRCLE ( 'NONE', #103519, 0.06509327318403745899 ) ;
#65854 = DIRECTION ( 'NONE',  ( 0.000000000000000000, 0.000000000000000000, 1.000000000000000000 ) ) ;
#65855 = DIRECTION ( 'NONE',  ( 0.000000000000000000, 0.000000000000000000, -1.000000000000000000 ) ) ;
#65856 = CARTESIAN_POINT ( 'NONE',  ( 5.399999999999932854, 12.50000000000000000, 3.637306695894644726 ) ) ;
#65857 = ORIENTED_EDGE ( 'NONE', *, *, #119176, .F. ) ;
#65858 = CARTESIAN_POINT ( 'NONE',  ( -0.6000000000000323963, 2.500000000000000000, -0.3464101615137759604 ) ) ;
#65859 = EDGE_CURVE ( 'NONE', #69451, #114181, #15028, .T. ) ;
#65860 = VECTOR ( 'NONE', #121945, 1000.000000000000000 ) ;
#65861 = ORIENTED_EDGE ( 'NONE', *, *, #72836, .F. ) ;
#65862 = CIRCLE ( 'NONE', #36554, 0.06509327318403745899 ) ;
#65863 = CONICAL_SURFACE ( 'NONE', #90912, 0.1000000000000002554, 0.003490658503988666988 ) ;
#65864 = ORIENTED_EDGE ( 'NONE', *, *, #84111, .T. ) ;
#65865 = EDGE_LOOP ( 'NONE', ( #100056, #54942 ) ) ;
#65866 = CARTESIAN_POINT ( 'NONE',  ( -5.000000000000026645, 12.50000000000000000, -3.637306695894650055 ) ) ;
#65867 = VECTOR ( 'NONE', #126162, 1000.000000000000000 ) ;
#65868 = FACE_OUTER_BOUND ( 'NONE', #105657, .T. ) ;
#65869 = DIRECTION ( 'NONE',  ( 0.000000000000000000, 0.000000000000000000, -1.000000000000000000 ) ) ;
#65870 = VERTEX_POINT ( 'NONE', #57589 ) ;
#65871 = CARTESIAN_POINT ( 'NONE',  ( 14.38463633656722607, 2.500000000000127454, -7.683002074691031247 ) ) ;
#65872 = AXIS2_PLACEMENT_3D ( 'NONE', #85412, #124703, #24561 ) ;
#65873 = VECTOR ( 'NONE', #14648, 1000.000000000000000 ) ;
#65874 = PLANE ( 'NONE',  #82513 ) ;
#65875 = DIRECTION ( 'NONE',  ( 0.000000000000000000, 0.000000000000000000, 1.000000000000000000 ) ) ;
#65876 = CARTESIAN_POINT ( 'NONE',  ( 185.2812500006828031, 0.000000000000000000, 7.700000000000000178 ) ) ;
#65878 = VECTOR ( 'NONE', #123877, 1000.000000000000000 ) ;
#65877 = CARTESIAN_POINT ( 'NONE',  ( -10.65000000000000391, 2.500000000000000000, -1.818653347947322141 ) ) ;
#65879 = CARTESIAN_POINT ( 'NONE',  ( -12.49999999999999289, 2.500000000000000000, 3.737306695894644371 ) ) ;
#65880 = EDGE_LOOP ( 'NONE', ( #117429, #60252, #39720, #101765 ) ) ;
#65881 = DIRECTION ( 'NONE',  ( 0.000000000000000000, 1.000000000000000000, 0.000000000000000000 ) ) ;
#65882 = ORIENTED_EDGE ( 'NONE', *, *, #89004, .T. ) ;
#65883 = VERTEX_POINT ( 'NONE', #106031 ) ;
#65884 = LINE ( 'NONE', #84884, #69706 ) ;
#65885 = FACE_OUTER_BOUND ( 'NONE', #9978, .T. ) ;
#65886 = CARTESIAN_POINT ( 'NONE',  ( 5.849999999999933920, 2.500000000000000000, -2.957883832488653830 ) ) ;
#65887 = CIRCLE ( 'NONE', #74216, 0.1000000000000002554 ) ;
#65888 = EDGE_LOOP ( 'NONE', ( #35509, #110766 ) ) ;
#65889 = ORIENTED_EDGE ( 'NONE', *, *, #97382, .F. ) ;
#65890 = CARTESIAN_POINT ( 'NONE',  ( 133.2169897921533845, 0.5000000000000000000, -2.337293474289257933 ) ) ;
#65891 = ADVANCED_FACE ( 'NONE', ( #45830 ), #125649, .T. ) ;
#65892 = DIRECTION ( 'NONE',  ( 0.000000000000000000, 0.000000000000000000, -1.000000000000000000 ) ) ;
#65893 = DIRECTION ( 'NONE',  ( 0.000000000000000000, 1.000000000000000000, 0.000000000000000000 ) ) ;
#65894 = EDGE_LOOP ( 'NONE', ( #5387, #114053 ) ) ;
#65895 = ORIENTED_EDGE ( 'NONE', *, *, #109737, .T. ) ;
#65896 = DIRECTION ( 'NONE',  ( 0.000000000000000000, 0.000000000000000000, 1.000000000000000000 ) ) ;
#65897 = CONICAL_SURFACE ( 'NONE', #49207, 0.1000000000000002554, 0.003490658503988666988 ) ;
#65898 = CIRCLE ( 'NONE', #61727, 0.1000000000000000472 ) ;
#65899 = ORIENTED_EDGE ( 'NONE', *, *, #62821, .T. ) ;
#65901 = VECTOR ( 'NONE', #123459, 1000.000000000000000 ) ;
#65900 = DIRECTION ( 'NONE',  ( -0.000000000000000000, -1.000000000000000000, -0.000000000000000000 ) ) ;
#65902 = DIRECTION ( 'NONE',  ( 0.000000000000000000, 0.000000000000000000, 1.000000000000000000 ) ) ;
#65903 = VERTEX_POINT ( 'NONE', #96841 ) ;
#65904 = FACE_OUTER_BOUND ( 'NONE', #95739, .T. ) ;
#65905 = DIRECTION ( 'NONE',  ( -0.000000000000000000, 1.000000000000000000, -0.000000000000000000 ) ) ;
#65906 = FACE_OUTER_BOUND ( 'NONE', #23046, .T. ) ;
#65907 = ADVANCED_FACE ( 'NONE', ( #27449 ), #56892, .T. ) ;
#65908 = FACE_OUTER_BOUND ( 'NONE', #72306, .T. ) ;
#65909 = EDGE_LOOP ( 'NONE', ( #28652, #117612 ) ) ;
#65910 = AXIS2_PLACEMENT_3D ( 'NONE', #63571, #34110, #51823 ) ;
#65911 = CARTESIAN_POINT ( 'NONE',  ( -8.950000000000009948, 2.500000000000000000, -6.841600689897072485 ) ) ;
#65913 = AXIS2_PLACEMENT_3D ( 'NONE', #2407, #10935, #90814 ) ;
#65912 = DIRECTION ( 'NONE',  ( 0.000000000000000000, 1.000000000000000000, 0.000000000000000000 ) ) ;
#65914 = ORIENTED_EDGE ( 'NONE', *, *, #3891, .F. ) ;
#65915 = ORIENTED_EDGE ( 'NONE', *, *, #32128, .F. ) ;
#65916 = CARTESIAN_POINT ( 'NONE',  ( 185.5468750003414300, -8.734944146203032389, -1.604583208406768146E-15 ) ) ;
#65917 = DIRECTION ( 'NONE',  ( 0.000000000000000000, 0.000000000000000000, -1.000000000000000000 ) ) ;
#65918 = LINE ( 'NONE', #25341, #105428 ) ;
#65919 = DIRECTION ( 'NONE',  ( 0.000000000000000000, 0.000000000000000000, 1.000000000000000000 ) ) ;
#65920 = DIRECTION ( 'NONE',  ( 0.000000000000000000, 0.000000000000000000, -1.000000000000000000 ) ) ;
#65921 = CARTESIAN_POINT ( 'NONE',  ( -2.050000000000032685, 12.50000000000000000, -6.560283801567339701 ) ) ;
#65922 = AXIS2_PLACEMENT_3D ( 'NONE', #41555, #81468, #82101 ) ;
#65923 = AXIS2_PLACEMENT_3D ( 'NONE', #34336, #93883, #66341 ) ;
#65924 = CARTESIAN_POINT ( 'NONE',  ( -8.350000000000012079, 2.500000000000000000, 2.857883832488649301 ) ) ;
#65925 = FACE_OUTER_BOUND ( 'NONE', #82570, .T. ) ;
#65926 = CARTESIAN_POINT ( 'NONE',  ( -11.24999999999999822, 2.500000000000000000, 1.472243186433545459 ) ) ;
#65927 = DIRECTION ( 'NONE',  ( 1.000000000000000000, 0.000000000000000000, 0.000000000000000000 ) ) ;
#65928 = EDGE_LOOP ( 'NONE', ( #58768, #75160, #9540, #6092 ) ) ;
#65929 = EDGE_CURVE ( 'NONE', #60457, #38221, #47763, .T. ) ;
#65931 = EDGE_LOOP ( 'NONE', ( #80713, #100716 ) ) ;
#65930 = VECTOR ( 'NONE', #61389, 1000.000000000000000 ) ;
#65932 = DIRECTION ( 'NONE',  ( -0.000000000000000000, -1.000000000000000000, -0.000000000000000000 ) ) ;
#65933 = ORIENTED_EDGE ( 'NONE', *, *, #109566, .T. ) ;
#65934 = FACE_OUTER_BOUND ( 'NONE', #99161, .T. ) ;
#65935 = AXIS2_PLACEMENT_3D ( 'NONE', #49027, #8422, #48361 ) ;
#65936 = DIRECTION ( 'NONE',  ( -0.000000000000000000, -1.000000000000000000, -0.000000000000000000 ) ) ;
#65937 = DIRECTION ( 'NONE',  ( -4.274815082592931898E-19, -0.9999939076577903929, -0.003490651415223739937 ) ) ;
#65938 = ADVANCED_FACE ( 'NONE', ( #35365 ), #27647, .T. ) ;
#65939 = ORIENTED_EDGE ( 'NONE', *, *, #129076, .F. ) ;
#65940 = DIRECTION ( 'NONE',  ( -0.000000000000000000, -1.000000000000000000, -0.000000000000000000 ) ) ;
#65941 = AXIS2_PLACEMENT_3D ( 'NONE', #54189, #64002, #42441 ) ;
#65942 = CIRCLE ( 'NONE', #63895, 0.09999999999999982514 ) ;
#65943 = CARTESIAN_POINT ( 'NONE',  ( 8.349999999999919709, 2.500000000000000000, -2.165063509461101710 ) ) ;
#65945 = ORIENTED_EDGE ( 'NONE', *, *, #67483, .T. ) ;
#65944 = DIRECTION ( 'NONE',  ( 0.000000000000000000, 1.000000000000000000, 0.000000000000000000 ) ) ;
#65946 = EDGE_CURVE ( 'NONE', #82878, #22551, #58982, .T. ) ;
#65947 = EDGE_CURVE ( 'NONE', #110204, #90702, #47123, .T. ) ;
#65948 = EDGE_CURVE ( 'NONE', #38247, #37082, #63178, .T. ) ;
#65949 = EDGE_CURVE ( 'NONE', #104107, #107896, #52710, .T. ) ;
#65950 = EDGE_CURVE ( 'NONE', #76636, #116200, #19245, .T. ) ;
#65951 = DIRECTION ( 'NONE',  ( -0.000000000000000000, 1.000000000000000000, -0.000000000000000000 ) ) ;
#65952 = ORIENTED_EDGE ( 'NONE', *, *, #115920, .F. ) ;
#65953 = AXIS2_PLACEMENT_3D ( 'NONE', #123859, #123240, #33573 ) ;
#65954 = EDGE_LOOP ( 'NONE', ( #104353, #75305, #2694, #8702 ) ) ;
#65955 = VERTEX_POINT ( 'NONE', #46453 ) ;
#65956 = ORIENTED_EDGE ( 'NONE', *, *, #84326, .F. ) ;
#65957 = DIRECTION ( 'NONE',  ( 0.000000000000000000, 1.000000000000000000, 0.000000000000000000 ) ) ;
#65958 = VECTOR ( 'NONE', #52123, 1000.000000000000000 ) ;
#65959 = EDGE_CURVE ( 'NONE', #24765, #64553, #87665, .T. ) ;
#65960 = FACE_OUTER_BOUND ( 'NONE', #112413, .T. ) ;
#65961 = CARTESIAN_POINT ( 'NONE',  ( -11.64999999999999680, 12.50000000000000000, -2.792790559304612508 ) ) ;
#65962 = ADVANCED_FACE ( 'NONE', ( #67357 ), #90351, .T. ) ;
#65963 = VECTOR ( 'NONE', #99758, 1000.000000000000000 ) ;
#65964 = DIRECTION ( 'NONE',  ( -0.000000000000000000, -1.000000000000000000, -0.000000000000000000 ) ) ;
#65965 = VECTOR ( 'NONE', #34170, 1000.000000000000000 ) ;
#65967 = ORIENTED_EDGE ( 'NONE', *, *, #19328, .T. ) ;
#65966 = EDGE_CURVE ( 'NONE', #121536, #107284, #66740, .T. ) ;
#65968 = CIRCLE ( 'NONE', #55514, 0.06509327318403745899 ) ;
#65970 = AXIS2_PLACEMENT_3D ( 'NONE', #43904, #105388, #33443 ) ;
#65969 = DIRECTION ( 'NONE',  ( -0.000000000000000000, 1.000000000000000000, -0.000000000000000000 ) ) ;
#65971 = ORIENTED_EDGE ( 'NONE', *, *, #79152, .F. ) ;
#65972 = CARTESIAN_POINT ( 'NONE',  ( 21.15177371151418129, -2.593223176056361989, -4.151029080743455779 ) ) ;
#65973 = DIRECTION ( 'NONE',  ( 0.000000000000000000, -0.9999939076577903929, 0.003490651415223739937 ) ) ;
#65974 = PRODUCT_DEFINITION ( 'UNKNOWN', '', #113204, #6147 ) ;
#65975 = FACE_OUTER_BOUND ( 'NONE', #124533, .T. ) ;
#65976 = LINE ( 'NONE', #54231, #25539 ) ;
#65977 = ORIENTED_EDGE ( 'NONE', *, *, #108255, .T. ) ;
#65978 = ORIENTED_EDGE ( 'NONE', *, *, #20878, .F. ) ;
#65979 = EDGE_LOOP ( 'NONE', ( #109148, #9704 ) ) ;
#65980 = FACE_OUTER_BOUND ( 'NONE', #6831, .T. ) ;
#65981 = CARTESIAN_POINT ( 'NONE',  ( 0.5999999999999612310, 2.500000000000000000, -0.4464101615137760493 ) ) ;
#65982 = DIRECTION ( 'NONE',  ( 0.000000000000000000, -0.9999939076577903929, 0.003490651415223739937 ) ) ;
#65983 = FACE_BOUND ( 'NONE', #42777, .T. ) ;
#65984 = LINE ( 'NONE', #24783, #91146 ) ;
#65985 = AXIS2_PLACEMENT_3D ( 'NONE', #12559, #53154, #4030 ) ;
#65986 = CARTESIAN_POINT ( 'NONE',  ( -7.499999999999976907, 2.500000000000000000, 4.430127018922196847 ) ) ;
#65987 = CARTESIAN_POINT ( 'NONE',  ( -12.29999999999999538, 12.50000000000000000, 4.611443907251934426 ) ) ;
#65988 = CARTESIAN_POINT ( 'NONE',  ( -0.6500000000000403233, 2.500000000000000000, 1.818653347947321475 ) ) ;
#65989 = CARTESIAN_POINT ( 'NONE',  ( 185.4635416670080872, -4.367472073101520635, 7.564683531249999149 ) ) ;
#65990 = AXIS2_PLACEMENT_3D ( 'NONE', #119800, #32086, #11773 ) ;
#65991 = CARTESIAN_POINT ( 'NONE',  ( 14.99999999999989164, 12.50000000000000000, 0.7579135962115869374 ) ) ;
#65992 = CARTESIAN_POINT ( 'NONE',  ( -8.350000000000012079, 12.50000000000000000, -2.857883832488653741 ) ) ;
#65993 = CONICAL_SURFACE ( 'NONE', #38842, 0.09999999999999999167, 0.003490658503988666988 ) ;
#65994 = CONICAL_SURFACE ( 'NONE', #51446, 0.09999999999999982514, 0.003490658503988666988 ) ;
#65995 = DIRECTION ( 'NONE',  ( -0.000000000000000000, -1.000000000000000000, -0.000000000000000000 ) ) ;
#65996 = AXIS2_PLACEMENT_3D ( 'NONE', #59081, #98997, #111374 ) ;
#65997 = ORIENTED_EDGE ( 'NONE', *, *, #127903, .T. ) ;
#65998 = B_SPLINE_CURVE_WITH_KNOTS ( 'NONE', 3,
 ( #102794, #94270, #103461, #13119, #22336, #93003, #4574, #104102 ),
 .UNSPECIFIED., .F., .F.,
 ( 4, 2, 2, 4 ),
 ( 0.000000000000000000, 0.01659259069806624451, 0.03318518139613248902, 0.06637036279226497804 ),
 .UNSPECIFIED. ) ;
#65999 = ORIENTED_EDGE ( 'NONE', *, *, #37021, .F. ) ;
#66000 = EDGE_LOOP ( 'NONE', ( #54684, #126974 ) ) ;
#66001 = ORIENTED_EDGE ( 'NONE', *, *, #88687, .F. ) ;
#66002 = DIRECTION ( 'NONE',  ( 0.000000000000000000, 1.000000000000000000, 0.000000000000000000 ) ) ;
#66003 = EDGE_CURVE ( 'NONE', #38017, #1197, #98970, .T. ) ;
#66004 = FACE_BOUND ( 'NONE', #39579, .T. ) ;
#66005 = LINE ( 'NONE', #125561, #97488 ) ;
#66006 = AXIS2_PLACEMENT_3D ( 'NONE', #123605, #1904, #44414 ) ;
#66007 = EDGE_CURVE ( 'NONE', #22187, #119878, #44719, .T. ) ;
#66010 = EDGE_CURVE ( 'NONE', #82094, #126222, #65448, .T. ) ;
#66009 = AXIS2_PLACEMENT_3D ( 'NONE', #28526, #116879, #11288 ) ;
#66008 = AXIS2_PLACEMENT_3D ( 'NONE', #124336, #52368, #92281 ) ;
#66011 = ORIENTED_EDGE ( 'NONE', *, *, #121810, .T. ) ;
#66012 = DIRECTION ( 'NONE',  ( 0.000000000000000000, 1.000000000000000000, 0.000000000000000000 ) ) ;
#66013 = CARTESIAN_POINT ( 'NONE',  ( 8.749999999999918288, 2.500000000000000000, 7.188010851410848723 ) ) ;
#66014 = VERTEX_POINT ( 'NONE', #107965 ) ;
#66015 = DIRECTION ( 'NONE',  ( 0.000000000000000000, 0.000000000000000000, 1.000000000000000000 ) ) ;
#66016 = DIRECTION ( 'NONE',  ( -0.000000000000000000, -1.000000000000000000, -0.000000000000000000 ) ) ;
#66017 = ADVANCED_FACE ( 'NONE', ( #20876 ), #88286, .T. ) ;
#66018 = CIRCLE ( 'NONE', #91064, 0.1000000000000002554 ) ;
#66019 = CIRCLE ( 'NONE', #55563, 0.1000000000000002554 ) ;
#66020 = VERTEX_POINT ( 'NONE', #59540 ) ;
#66021 = DIRECTION ( 'NONE',  ( 0.000000000000000000, 1.000000000000000000, 0.000000000000000000 ) ) ;
#66022 = DIRECTION ( 'NONE',  ( -0.000000000000000000, 1.000000000000000000, -0.000000000000000000 ) ) ;
#66023 = ORIENTED_EDGE ( 'NONE', *, *, #117203, .T. ) ;
#66024 = DIRECTION ( 'NONE',  ( 0.000000000000000000, 0.000000000000000000, -1.000000000000000000 ) ) ;
#66025 = CARTESIAN_POINT ( 'NONE',  ( -4.150000000000028777, 2.500000000000000000, -5.802370205355749988 ) ) ;
#66026 = ORIENTED_EDGE ( 'NONE', *, *, #29884, .F. ) ;
#66027 = CARTESIAN_POINT ( 'NONE',  ( -0.2000000000000399791, 2.500000000000000000, -4.576537180435977348 ) ) ;
#66028 = ORIENTED_EDGE ( 'NONE', *, *, #46756, .T. ) ;
#66029 = ORIENTED_EDGE ( 'NONE', *, *, #89732, .F. ) ;
#66030 = CARTESIAN_POINT ( 'NONE',  ( -10.00000000000000533, 2.500000000000000000, 5.022947341949748790 ) ) ;
#66031 = EDGE_CURVE ( 'NONE', #60164, #67886, #60171, .T. ) ;
#66032 = VERTEX_POINT ( 'NONE', #98778 ) ;
#66033 = CARTESIAN_POINT ( 'NONE',  ( 7.499999999999925393, 2.500000000000000000, -0.6928203230275541413 ) ) ;
#66034 = DIRECTION ( 'NONE',  ( 0.000000000000000000, 0.000000000000000000, -1.000000000000000000 ) ) ;
#66035 = AXIS2_PLACEMENT_3D ( 'NONE', #50578, #41435, #81971 ) ;
#66036 = ORIENTED_EDGE ( 'NONE', *, *, #76194, .F. ) ;
#66037 = AXIS2_PLACEMENT_3D ( 'NONE', #109410, #102177, #102796 ) ;
#66038 = DIRECTION ( 'NONE',  ( -1.000000000000000000, 0.000000000000000000, 1.084202172485504434E-16 ) ) ;
#66039 = DIRECTION ( 'NONE',  ( 0.000000000000000000, 0.000000000000000000, -1.000000000000000000 ) ) ;
#66040 = CARTESIAN_POINT ( 'NONE',  ( 187.5000000000000000, 1.375000000000000000, 7.576237522675751457 ) ) ;
#66041 = DIRECTION ( 'NONE',  ( -0.000000000000000000, -1.000000000000000000, -0.000000000000000000 ) ) ;
#66042 = PLANE ( 'NONE',  #77933 ) ;
#66043 = CARTESIAN_POINT ( 'NONE',  ( 17.45053695044966346, 1.969637996572654481, -4.507340027902842827 ) ) ;
#66044 = ORIENTED_EDGE ( 'NONE', *, *, #95664, .F. ) ;
#66045 = EDGE_LOOP ( 'NONE', ( #100228, #103937, #439, #115737 ) ) ;
#66046 = DIRECTION ( 'NONE',  ( 0.000000000000000000, 0.000000000000000000, 1.000000000000000000 ) ) ;
#66047 = EDGE_CURVE ( 'NONE', #112495, #77768, #100081, .T. ) ;
#66048 = FACE_OUTER_BOUND ( 'NONE', #26590, .T. ) ;
#66049 = CARTESIAN_POINT ( 'NONE',  ( -3.550000000000027800, 12.50000000000000000, 6.083687093685482772 ) ) ;
#66052 = EDGE_LOOP ( 'NONE', ( #9811, #1856, #119629, #86644 ) ) ;
#66051 = EDGE_LOOP ( 'NONE', ( #15912, #105020, #129088, #36642 ) ) ;
#66050 = AXIS2_PLACEMENT_3D ( 'NONE', #117439, #107664, #17982 ) ;
#66053 = ORIENTED_EDGE ( 'NONE', *, *, #37474, .T. ) ;
#66054 = FACE_OUTER_BOUND ( 'NONE', #10738, .T. ) ;
#66055 = CARTESIAN_POINT ( 'NONE',  ( -2.500000000000031086, 2.500000000000000000, 3.637306695894644726 ) ) ;
#66056 = CARTESIAN_POINT ( 'NONE',  ( 9.799999999999913669, 2.500000000000000000, 4.776537180435972196 ) ) ;
#66057 = CONICAL_SURFACE ( 'NONE', #128785, 0.1000000000000000472, 0.003490658503988666988 ) ;
#66058 = CARTESIAN_POINT ( 'NONE',  ( -11.64999999999999680, 12.50000000000000000, 7.188010851410848723 ) ) ;
#66059 = CARTESIAN_POINT ( 'NONE',  ( -10.60000000000000320, 2.500000000000000000, -4.083716857408422385 ) ) ;
#66060 = DIRECTION ( 'NONE',  ( -0.000000000000000000, -1.000000000000000000, -0.000000000000000000 ) ) ;
#66061 = DIRECTION ( 'NONE',  ( 0.000000000000000000, 1.000000000000000000, 0.000000000000000000 ) ) ;
#66062 = FACE_OUTER_BOUND ( 'NONE', #51264, .T. ) ;
#66063 = EDGE_CURVE ( 'NONE', #79720, #37929, #38600, .T. ) ;
#66064 = FACE_OUTER_BOUND ( 'NONE', #70387, .T. ) ;
#66065 = ORIENTED_EDGE ( 'NONE', *, *, #117958, .T. ) ;
#66066 = DIRECTION ( 'NONE',  ( -0.000000000000000000, -1.000000000000000000, -0.000000000000000000 ) ) ;
#66067 = EDGE_LOOP ( 'NONE', ( #129155, #81109, #85087, #12732 ) ) ;
#66068 = EDGE_CURVE ( 'NONE', #55758, #30920, #13071, .T. ) ;
#66069 = ORIENTED_EDGE ( 'NONE', *, *, #19097, .T. ) ;
#66070 = DIRECTION ( 'NONE',  ( -0.000000000000000000, 1.000000000000000000, -0.000000000000000000 ) ) ;
#66071 = CARTESIAN_POINT ( 'NONE',  ( 9.149999999999915090, 2.500000000000000000, -2.165063509461101710 ) ) ;
#66072 = VECTOR ( 'NONE', #116407, 1000.000000000000000 ) ;
#66073 = DIRECTION ( 'NONE',  ( -1.000000000000000000, 0.000000000000000000, -0.000000000000000000 ) ) ;
#66074 = CARTESIAN_POINT ( 'NONE',  ( 108.0000000000000142, 9.000000000000001776, -4.500000000000003553 ) ) ;
#66076 = DIRECTION ( 'NONE',  ( 0.000000000000000000, 0.000000000000000000, -1.000000000000000000 ) ) ;
#66075 = PRODUCT_DEFINITION_SHAPE ( 'NONE', 'NONE',  #129622 ) ;
#66077 = DIRECTION ( 'NONE',  ( 0.000000000000000000, 0.000000000000000000, -1.000000000000000000 ) ) ;
#66078 = CONICAL_SURFACE ( 'NONE', #60137, 0.09999999999999982514, 0.003490658503988666988 ) ;
#66079 = DIRECTION ( 'NONE',  ( 0.000000000000000000, 1.000000000000000000, 0.000000000000000000 ) ) ;
#66080 = VERTEX_POINT ( 'NONE', #89613 ) ;
#66081 = DIRECTION ( 'NONE',  ( 0.000000000000000000, 0.000000000000000000, 1.000000000000000000 ) ) ;
#66082 = CIRCLE ( 'NONE', #110013, 0.06509327318403745899 ) ;
#66083 = CIRCLE ( 'NONE', #74501, 0.1000000000000002554 ) ;
#66084 = CARTESIAN_POINT ( 'NONE',  ( 0.1999999999999571565, 2.500000000000000000, 3.883716857408420431 ) ) ;
#66085 = ORIENTED_EDGE ( 'NONE', *, *, #114967, .T. ) ;
#66086 = ORIENTED_EDGE ( 'NONE', *, *, #117043, .T. ) ;
#66087 = AXIS2_PLACEMENT_3D ( 'NONE', #87077, #85788, #127032 ) ;
#66088 = ADVANCED_FACE ( 'NONE', ( #69308 ), #50335, .T. ) ;
#66089 = ORIENTED_EDGE ( 'NONE', *, *, #18809, .F. ) ;
#66090 = ORIENTED_EDGE ( 'NONE', *, *, #68939, .T. ) ;
#66091 = CARTESIAN_POINT ( 'NONE',  ( -8.350000000000010303, 12.50000000000000000, 6.495190528383297135 ) ) ;
#66092 = DIRECTION ( 'NONE',  ( 0.000000000000000000, -0.000000000000000000, 1.000000000000000000 ) ) ;
#66093 = EDGE_CURVE ( 'NONE', #66296, #127206, #99448, .T. ) ;
#66094 = DIRECTION ( 'NONE',  ( 0.000000000000000000, 0.000000000000000000, 1.000000000000000000 ) ) ;
#66095 = DIRECTION ( 'NONE',  ( 0.000000000000000000, 1.000000000000000000, 0.000000000000000000 ) ) ;
#66096 = AXIS2_PLACEMENT_3D ( 'NONE', #100789, #92936, #42557 ) ;
#66097 = DIRECTION ( 'NONE',  ( 0.000000000000000000, 0.000000000000000000, -1.000000000000000000 ) ) ;
#66098 = EDGE_LOOP ( 'NONE', ( #37922, #19089 ) ) ;
#66099 = EDGE_CURVE ( 'NONE', #79663, #85834, #9116, .T. ) ;
#66100 = ADVANCED_FACE ( 'NONE', ( #98134 ), #67432, .T. ) ;
#66101 = EDGE_CURVE ( 'NONE', #71261, #122087, #90234, .T. ) ;
#66102 = LINE ( 'NONE', #73342, #53535 ) ;
#66103 = EDGE_CURVE ( 'NONE', #49433, #56692, #117613, .T. ) ;
#66104 = DIRECTION ( 'NONE',  ( -0.000000000000000000, 1.000000000000000000, -0.000000000000000000 ) ) ;
#66105 = VERTEX_POINT ( 'NONE', #18921 ) ;
#66106 = VERTEX_POINT ( 'NONE', #50995 ) ;
#66108 = ORIENTED_EDGE ( 'NONE', *, *, #101917, .F. ) ;
#66107 = EDGE_CURVE ( 'NONE', #35838, #78758, #107169, .T. ) ;
#66109 = DIRECTION ( 'NONE',  ( 0.000000000000000000, 0.000000000000000000, 1.000000000000000000 ) ) ;
#66110 = ADVANCED_FACE ( 'NONE', ( #110536 ), #52798, .T. ) ;
#66111 = EDGE_CURVE ( 'NONE', #39170, #27061, #71586, .T. ) ;
#66112 = DIRECTION ( 'NONE',  ( 0.000000000000000000, 1.000000000000000000, 0.000000000000000000 ) ) ;
#66113 = DIRECTION ( 'NONE',  ( 0.000000000000000000, 0.000000000000000000, -1.000000000000000000 ) ) ;
#66114 = EDGE_CURVE ( 'NONE', #55194, #90471, #123898, .T. ) ;
#66115 = EDGE_CURVE ( 'NONE', #68282, #90560, #100707, .T. ) ;
#66116 = ORIENTED_EDGE ( 'NONE', *, *, #19884, .T. ) ;
#66117 = DIRECTION ( 'NONE',  ( -0.000000000000000000, -1.000000000000000000, -0.000000000000000000 ) ) ;
#66118 = DIRECTION ( 'NONE',  ( 0.000000000000000000, 0.000000000000000000, -1.000000000000000000 ) ) ;
#66119 = CARTESIAN_POINT ( 'NONE',  ( 12.69999999999990337, 2.500000000000000000, 3.983716857408420076 ) ) ;
#66120 = DIRECTION ( 'NONE',  ( 0.000000000000000000, 0.000000000000000000, 1.000000000000000000 ) ) ;
#66121 = CARTESIAN_POINT ( 'NONE',  ( -15.39999999999997904, 12.50000000000000000, 0.000000000000000000 ) ) ;
#66122 = ADVANCED_FACE ( 'NONE', ( #30719 ), #90897, .T. ) ;
#66123 = ORIENTED_EDGE ( 'NONE', *, *, #93173, .F. ) ;
#66124 = CIRCLE ( 'NONE', #101652, 0.09999999999999982514 ) ;
#66125 = DIRECTION ( 'NONE',  ( -0.000000000000000000, 1.000000000000000000, -0.000000000000000000 ) ) ;
#66126 = AXIS2_PLACEMENT_3D ( 'NONE', #30727, #111165, #79794 ) ;
#66127 = VERTEX_POINT ( 'NONE', #24097 ) ;
#66128 = VERTEX_POINT ( 'NONE', #102012 ) ;
#66129 = ORIENTED_EDGE ( 'NONE', *, *, #31221, .T. ) ;
#66130 = DIRECTION ( 'NONE',  ( -0.000000000000000000, 1.000000000000000000, -0.000000000000000000 ) ) ;
#66131 = FACE_BOUND ( 'NONE', #119604, .T. ) ;
#66132 = DIRECTION ( 'NONE',  ( 0.000000000000000000, 0.000000000000000000, -1.000000000000000000 ) ) ;
#66133 = CARTESIAN_POINT ( 'NONE',  ( 194.5000000000000000, 0.000000000000000000, 0.000000000000000000 ) ) ;
#66135 = AXIS2_PLACEMENT_3D ( 'NONE', #126864, #27341, #88187 ) ;
#66134 = CIRCLE ( 'NONE', #1383, 0.1000000000000000056 ) ;
#66136 = DIRECTION ( 'NONE',  ( 1.000000000000000000, 0.000000000000000000, 0.000000000000000000 ) ) ;
#66137 = VERTEX_POINT ( 'NONE', #21520 ) ;
#66138 = CARTESIAN_POINT ( 'NONE',  ( 133.2169897921533845, 2.500000000000000000, -2.337293474289257933 ) ) ;
#66139 = DIRECTION ( 'NONE',  ( 0.000000000000000000, 0.000000000000000000, 1.000000000000000000 ) ) ;
#66140 = DIRECTION ( 'NONE',  ( 0.000000000000000000, 0.000000000000000000, 1.000000000000000000 ) ) ;
#66141 = DIRECTION ( 'NONE',  ( -4.274815082592931898E-19, -0.9999939076577903929, -0.003490651415223739937 ) ) ;
#66142 = EDGE_LOOP ( 'NONE', ( #102142, #79743 ) ) ;
#66144 = AXIS2_PLACEMENT_3D ( 'NONE', #98333, #99643, #87223 ) ;
#66143 = CONICAL_SURFACE ( 'NONE', #80833, 0.1000000000000000472, 0.003490658503988666988 ) ;
#66145 = CARTESIAN_POINT ( 'NONE',  ( -3.300000000000027800, 2.500000000000000000, -4.430127018922202176 ) ) ;
#66146 = VECTOR ( 'NONE', #53668, 1000.000000000000000 ) ;
#66147 = DIRECTION ( 'NONE',  ( -4.274815082592931898E-19, -0.9999939076577903929, -0.003490651415223739937 ) ) ;
#66148 = ORIENTED_EDGE ( 'NONE', *, *, #5948, .T. ) ;
#66149 = CARTESIAN_POINT ( 'NONE',  ( -6.250000000000017764, 2.500000000000000000, 7.088010851410848190 ) ) ;
#66150 = FACE_BOUND ( 'NONE', #36202, .T. ) ;
#66151 = LINE ( 'NONE', #106088, #118320 ) ;
#66152 = EDGE_CURVE ( 'NONE', #3902, #127429, #54844, .T. ) ;
#66153 = ORIENTED_EDGE ( 'NONE', *, *, #97139, .T. ) ;
#66154 = DIRECTION ( 'NONE',  ( 0.000000000000000000, 0.000000000000000000, 1.000000000000000000 ) ) ;
#66155 = DIRECTION ( 'NONE',  ( -0.000000000000000000, 1.000000000000000000, -0.000000000000000000 ) ) ;
#66156 = EDGE_CURVE ( 'NONE', #14509, #105930, #19340, .T. ) ;
#66157 = ORIENTED_EDGE ( 'NONE', *, *, #19009, .F. ) ;
#66158 = VERTEX_POINT ( 'NONE', #64019 ) ;
#66159 = CARTESIAN_POINT ( 'NONE',  ( 186.1250000000000000, -8.891194145520236347, -1.633285867636356693E-15 ) ) ;
#66160 = AXIS2_PLACEMENT_3D ( 'NONE', #1157, #60732, #100632 ) ;
#66161 = VERTEX_POINT ( 'NONE', #12331 ) ;
#66162 = CARTESIAN_POINT ( 'NONE',  ( 185.1302083336747728, -4.367472073101514418, -7.564683531250002702 ) ) ;
#66163 = CIRCLE ( 'NONE', #41163, 0.1000000000000002554 ) ;
#66164 = DIRECTION ( 'NONE',  ( 0.000000000000000000, 1.000000000000000000, 0.000000000000000000 ) ) ;
#66165 = ADVANCED_FACE ( 'NONE', ( #113112 ), #92179, .T. ) ;
#66166 = AXIS2_PLACEMENT_3D ( 'NONE', #24610, #34443, #56618 ) ;
#66167 = DIRECTION ( 'NONE',  ( -0.000000000000000000, -1.000000000000000000, -0.000000000000000000 ) ) ;
#66168 = DIRECTION ( 'NONE',  ( 0.000000000000000000, 0.000000000000000000, -1.000000000000000000 ) ) ;
#66169 = DIRECTION ( 'NONE',  ( -0.000000000000000000, -1.000000000000000000, -0.000000000000000000 ) ) ;
#66170 = CONICAL_SURFACE ( 'NONE', #32762, 0.09999999999999982514, 0.003490658503988666988 ) ;
#66171 = EDGE_LOOP ( 'NONE', ( #92989, #85688, #106781, #87805 ) ) ;
#66172 = CONICAL_SURFACE ( 'NONE', #45261, 0.09999999999999982514, 0.003490658503988666988 ) ;
#66173 = DIRECTION ( 'NONE',  ( 0.000000000000000000, -0.9999939076577903929, 0.003490651415223739937 ) ) ;
#66174 = DIRECTION ( 'NONE',  ( 0.000000000000000000, -0.9999939076577903929, 0.003490651415223739937 ) ) ;
#66175 = CARTESIAN_POINT ( 'NONE',  ( -10.65000000000000391, 2.500000000000000000, -1.718653347947322052 ) ) ;
#66176 = CARTESIAN_POINT ( 'NONE',  ( -6.650000000000015454, 2.500000000000000000, 2.757883832488649656 ) ) ;
#66178 = ORIENTED_EDGE ( 'NONE', *, *, #83713, .T. ) ;
#66177 = ORIENTED_EDGE ( 'NONE', *, *, #90672, .T. ) ;
#66179 = FACE_BOUND ( 'NONE', #38880, .T. ) ;
#66180 = VERTEX_POINT ( 'NONE', #33914 ) ;
#66181 = CARTESIAN_POINT ( 'NONE',  ( 187.5000000000000000, 0.000000000000000000, 0.000000000000000000 ) ) ;
#66182 = CARTESIAN_POINT ( 'NONE',  ( -11.89999999999999680, 2.500000000000000000, -0.2464101615137742063 ) ) ;
#66183 = AXIS2_PLACEMENT_3D ( 'NONE', #1744, #90780, #1107 ) ;
#66184 = ORIENTED_EDGE ( 'NONE', *, *, #74977, .F. ) ;
#66185 = DIRECTION ( 'NONE',  ( 0.000000000000000000, 1.000000000000000000, 0.000000000000000000 ) ) ;
#66186 = CARTESIAN_POINT ( 'NONE',  ( -3.550000000000031797, 2.500000000000000000, -6.248780366869526759 ) ) ;
#66187 = FACE_OUTER_BOUND ( 'NONE', #119293, .T. ) ;
#66188 = AXIS2_PLACEMENT_3D ( 'NONE', #107098, #77009, #114984 ) ;
#66189 = DIRECTION ( 'NONE',  ( 0.000000000000000000, -0.9999939076577903929, 0.003490651415223739937 ) ) ;
#66190 = ORIENTED_EDGE ( 'NONE', *, *, #91351, .T. ) ;
#66191 = CARTESIAN_POINT ( 'NONE',  ( 13.54999999999990123, 2.500000000000000000, 1.918653347947321564 ) ) ;
#66192 = DIRECTION ( 'NONE',  ( -0.000000000000000000, -1.000000000000000000, -0.000000000000000000 ) ) ;
#66193 = CARTESIAN_POINT ( 'NONE',  ( 187.3177083336747160, 4.367472073101515306, 7.564683531250000925 ) ) ;
#66194 = CARTESIAN_POINT ( 'NONE',  ( -9.350000000000006750, 2.500000000000000000, -2.511473670974877948 ) ) ;
#66195 = CARTESIAN_POINT ( 'NONE',  ( -12.49999999999999289, 2.500000000000000000, 3.537306695894645081 ) ) ;
#66196 = ADVANCED_FACE ( 'NONE', ( #2497 ), #561, .T. ) ;
#66197 = ORIENTED_EDGE ( 'NONE', *, *, #26127, .F. ) ;
#66198 = VERTEX_POINT ( 'NONE', #42464 ) ;
#66199 = DIRECTION ( 'NONE',  ( -4.274815082592931898E-19, -0.9999939076577903929, -0.003490651415223739937 ) ) ;
#66200 = ORIENTED_EDGE ( 'NONE', *, *, #98594, .T. ) ;
#66201 = CARTESIAN_POINT ( 'NONE',  ( -6.850000000000017408, 2.500000000000000000, -6.148780366869526226 ) ) ;
#66203 = VERTEX_POINT ( 'NONE', #32656 ) ;
#66202 = VERTEX_POINT ( 'NONE', #31354 ) ;
#66204 = ORIENTED_EDGE ( 'NONE', *, *, #50573, .T. ) ;
#66205 = DIRECTION ( 'NONE',  ( 0.000000000000000000, 1.000000000000000000, 0.000000000000000000 ) ) ;
#66206 = DIRECTION ( 'NONE',  ( 0.000000000000000000, 0.000000000000000000, 1.000000000000000000 ) ) ;
#66207 = DIRECTION ( 'NONE',  ( 0.000000000000000000, 0.000000000000000000, 1.000000000000000000 ) ) ;
#66208 = FILL_AREA_STYLE_COLOUR ( '', #49832 ) ;
#66209 = FACE_OUTER_BOUND ( 'NONE', #55440, .T. ) ;
#66210 = FACE_OUTER_BOUND ( 'NONE', #66984, .T. ) ;
#66211 = EDGE_CURVE ( 'NONE', #126580, #31765, #21403, .T. ) ;
#66212 = DIRECTION ( 'NONE',  ( 0.000000000000000000, 1.000000000000000000, 0.000000000000000000 ) ) ;
#66213 = ORIENTED_EDGE ( 'NONE', *, *, #36405, .T. ) ;
#66214 = EDGE_CURVE ( 'NONE', #65156, #121453, #65307, .T. ) ;
#66215 = DIRECTION ( 'NONE',  ( -0.000000000000000000, -1.000000000000000000, -0.000000000000000000 ) ) ;
#66216 = VERTEX_POINT ( 'NONE', #113771 ) ;
#66218 = EDGE_LOOP ( 'NONE', ( #28246, #62599, #81319, #118394 ) ) ;
#66217 = AXIS2_PLACEMENT_3D ( 'NONE', #106130, #6597, #47218 ) ;
#66219 = ORIENTED_EDGE ( 'NONE', *, *, #37097, .F. ) ;
#66220 = ORIENTED_EDGE ( 'NONE', *, *, #31293, .T. ) ;
#66221 = CIRCLE ( 'NONE', #116387, 0.1000000000000002554 ) ;
#66222 = CARTESIAN_POINT ( 'NONE',  ( -3.150000000000032330, 12.50000000000000000, -6.213873640053564351 ) ) ;
#66223 = ORIENTED_EDGE ( 'NONE', *, *, #37055, .T. ) ;
#66224 = ADVANCED_FACE ( 'NONE', ( #31997 ), #46525, .T. ) ;
#66225 = ORIENTED_EDGE ( 'NONE', *, *, #4144, .T. ) ;
#66227 = AXIS2_PLACEMENT_3D ( 'NONE', #49288, #89191, #119944 ) ;
#66226 = AXIS2_PLACEMENT_3D ( 'NONE', #10425, #60194, #39908 ) ;
#66228 = LINE ( 'NONE', #113403, #35095 ) ;
#66229 = CARTESIAN_POINT ( 'NONE',  ( 187.3593750003414016, 0.000000000000000000, 7.564683531250000925 ) ) ;
#66230 = DIRECTION ( 'NONE',  ( 1.000000000000000000, 0.000000000000000000, 0.000000000000000000 ) ) ;
#66231 = FACE_OUTER_BOUND ( 'NONE', #51259, .T. ) ;
#66232 = FACE_OUTER_BOUND ( 'NONE', #45408, .T. ) ;
#66233 = ORIENTED_EDGE ( 'NONE', *, *, #97769, .T. ) ;
#66234 = CIRCLE ( 'NONE', #72517, 0.06509327318403745899 ) ;
#66235 = DIRECTION ( 'NONE',  ( 0.000000000000000000, 0.000000000000000000, 1.000000000000000000 ) ) ;
#66237 = AXIS2_PLACEMENT_3D ( 'NONE', #66783, #106710, #112540 ) ;
#66236 = AXIS2_PLACEMENT_3D ( 'NONE', #113928, #64169, #124394 ) ;
#66238 = ORIENTED_EDGE ( 'NONE', *, *, #99955, .F. ) ;
#66239 = CARTESIAN_POINT ( 'NONE',  ( -9.999999999999969802, 2.500000000000000000, -0.1000000000000022815 ) ) ;
#66240 = AXIS2_PLACEMENT_3D ( 'NONE', #98362, #68261, #108828 ) ;
#66241 = ORIENTED_EDGE ( 'NONE', *, *, #32799, .F. ) ;
#66242 = DIRECTION ( 'NONE',  ( 0.000000000000000000, 1.000000000000000000, 0.000000000000000000 ) ) ;
#66243 = ORIENTED_EDGE ( 'NONE', *, *, #100483, .T. ) ;
#66244 = ORIENTED_EDGE ( 'NONE', *, *, #121635, .T. ) ;
#66245 = CARTESIAN_POINT ( 'NONE',  ( 7.499999999999923617, 2.500000000000000000, 0.7928203230275495672 ) ) ;
#66246 = DIRECTION ( 'NONE',  ( -4.274815082592931898E-19, -0.9999939076577903929, -0.003490651415223739937 ) ) ;
#66247 = EDGE_CURVE ( 'NONE', #41822, #45891, #84183, .T. ) ;
#66248 = DIRECTION ( 'NONE',  ( -0.000000000000000000, -1.000000000000000000, -0.000000000000000000 ) ) ;
#66249 = CARTESIAN_POINT ( 'NONE',  ( -8.750000000000008882, 12.50000000000000000, -2.857883832488653741 ) ) ;
#66250 = CARTESIAN_POINT ( 'NONE',  ( 8.749999999999921840, 2.500000000000000000, 2.957883832488649389 ) ) ;
#66251 = ORIENTED_EDGE ( 'NONE', *, *, #108837, .F. ) ;
#66252 = DIRECTION ( 'NONE',  ( -4.274815082592931898E-19, -0.9999939076577903929, -0.003490651415223739937 ) ) ;
#66253 = DIRECTION ( 'NONE',  ( 0.000000000000000000, 0.000000000000000000, 1.000000000000000000 ) ) ;
#66254 = ADVANCED_FACE ( 'NONE', ( #94122 ), #93486, .T. ) ;
#66255 = DIRECTION ( 'NONE',  ( -0.000000000000000000, 1.000000000000000000, -0.000000000000000000 ) ) ;
#66256 = CIRCLE ( 'NONE', #108020, 0.06509327318403745899 ) ;
#66257 = CARTESIAN_POINT ( 'NONE',  ( 5.599999999999931255, 12.50000000000000000, 3.983716857408420076 ) ) ;
#66258 = AXIS2_PLACEMENT_3D ( 'NONE', #33382, #93576, #81178 ) ;
#66259 = EDGE_CURVE ( 'NONE', #87328, #37658, #94559, .T. ) ;
#66260 = CONICAL_SURFACE ( 'NONE', #80943, 0.1000000000000002554, 0.003490658503988666988 ) ;
#66261 = LINE ( 'NONE', #25691, #43813 ) ;
#66262 = ORIENTED_EDGE ( 'NONE', *, *, #20241, .F. ) ;
#66263 = AXIS2_PLACEMENT_3D ( 'NONE', #23156, #101731, #112840 ) ;
#66264 = ORIENTED_EDGE ( 'NONE', *, *, #115428, .F. ) ;
#66265 = ADVANCED_FACE ( 'NONE', ( #121004, #72564 ), #112483, .F. ) ;
#66266 = EDGE_CURVE ( 'NONE', #71492, #34635, #23558, .T. ) ;
#66267 = DIRECTION ( 'NONE',  ( 0.000000000000000000, -0.000000000000000000, 1.000000000000000000 ) ) ;
#66268 = ADVANCED_FACE ( 'NONE', ( #61459 ), #101372, .T. ) ;
#66269 = AXIS2_PLACEMENT_3D ( 'NONE', #46876, #85501, #86780 ) ;
#66270 = ORIENTED_EDGE ( 'NONE', *, *, #10720, .T. ) ;
#66271 = CIRCLE ( 'NONE', #80952, 0.06509327318403741736 ) ;
#66272 = CARTESIAN_POINT ( 'NONE',  ( -2.500000000000030642, 2.500000000000000000, -5.022947341949754119 ) ) ;
#66273 = DIRECTION ( 'NONE',  ( -0.000000000000000000, 1.000000000000000000, -0.000000000000000000 ) ) ;
#66274 = CONICAL_SURFACE ( 'NONE', #51624, 0.1000000000000000472, 0.003490658503988666988 ) ;
#66275 = ADVANCED_FACE ( 'NONE', ( #81714 ), #15115, .T. ) ;
#66276 = ORIENTED_EDGE ( 'NONE', *, *, #14090, .T. ) ;
#66277 = CARTESIAN_POINT ( 'NONE',  ( 184.6250000000000000, -8.891194145520236347, -1.633285867636356693E-15 ) ) ;
#66279 = AXIS2_PLACEMENT_3D ( 'NONE', #65396, #35950, #85685 ) ;
#66278 = DIRECTION ( 'NONE',  ( 0.000000000000000000, 0.000000000000000000, 1.000000000000000000 ) ) ;
#66280 = FACE_OUTER_BOUND ( 'NONE', #86666, .T. ) ;
#66281 =( LENGTH_UNIT ( ) NAMED_UNIT ( * ) SI_UNIT ( .MILLI., .METRE. ) );
#66282 = DIRECTION ( 'NONE',  ( 0.000000000000000000, 0.000000000000000000, -1.000000000000000000 ) ) ;
#66283 = ORIENTED_EDGE ( 'NONE', *, *, #59152, .F. ) ;
#66284 = ADVANCED_FACE ( 'NONE', ( #114397 ), #77837, .T. ) ;
#66285 = CONICAL_SURFACE ( 'NONE', #118504, 0.1000000000000002554, 0.003490658503988666988 ) ;
#66287 = CIRCLE ( 'NONE', #76667, 0.06509327318403745899 ) ;
#66286 = CONICAL_SURFACE ( 'NONE', #97677, 0.1000000000000002554, 0.003490658503988666988 ) ;
#66288 = CARTESIAN_POINT ( 'NONE',  ( -11.84999999999999609, 12.50000000000000000, 6.213873640053559022 ) ) ;
#66289 = DIRECTION ( 'NONE',  ( 0.000000000000000000, -0.9999939076577903929, 0.003490651415223739937 ) ) ;
#66290 = ORIENTED_EDGE ( 'NONE', *, *, #101124, .T. ) ;
#66291 = DIRECTION ( 'NONE',  ( 0.000000000000000000, 0.000000000000000000, 1.000000000000000000 ) ) ;
#66292 = DIRECTION ( 'NONE',  ( 0.000000000000000000, 0.000000000000000000, -1.000000000000000000 ) ) ;
#66293 = DIRECTION ( 'NONE',  ( 0.000000000000000000, 0.000000000000000000, 1.000000000000000000 ) ) ;
#66294 = ORIENTED_EDGE ( 'NONE', *, *, #105223, .T. ) ;
#66295 = FACE_OUTER_BOUND ( 'NONE', #56201, .T. ) ;
#66296 = VERTEX_POINT ( 'NONE', #96675 ) ;
#66297 = CARTESIAN_POINT ( 'NONE',  ( -1.650000000000034328, 12.50000000000000000, -2.857883832488653741 ) ) ;
#66298 = DIRECTION ( 'NONE',  ( -0.000000000000000000, -1.000000000000000000, -0.000000000000000000 ) ) ;
#66299 = CIRCLE ( 'NONE', #41198, 0.06509327318403745899 ) ;
#66300 = CARTESIAN_POINT ( 'NONE',  ( -12.49999999999995914, 12.50000000000000000, -4.395220292106237103 ) ) ;
#66301 = ORIENTED_EDGE ( 'NONE', *, *, #41140, .F. ) ;
#66302 = DIRECTION ( 'NONE',  ( 0.000000000000000000, 0.000000000000000000, 1.000000000000000000 ) ) ;
#66303 = DIRECTION ( 'NONE',  ( -0.000000000000000000, -1.000000000000000000, -0.000000000000000000 ) ) ;
#66304 = ORIENTED_EDGE ( 'NONE', *, *, #90935, .T. ) ;
#66305 = EDGE_LOOP ( 'NONE', ( #120896, #13758, #104950, #65669 ) ) ;
#66306 = FACE_OUTER_BOUND ( 'NONE', #124172, .T. ) ;
#66307 = AXIS2_PLACEMENT_3D ( 'NONE', #29363, #120311, #30657 ) ;
#66308 = EDGE_CURVE ( 'NONE', #5152, #32237, #56985, .T. ) ;
#66309 = AXIS2_PLACEMENT_3D ( 'NONE', #1555, #41517, #42140 ) ;
#66310 = ORIENTED_EDGE ( 'NONE', *, *, #1594, .F. ) ;
#66311 = DIRECTION ( 'NONE',  ( 0.000000000000000000, 1.000000000000000000, 0.000000000000000000 ) ) ;
#66312 = CARTESIAN_POINT ( 'NONE',  ( 6.649999999999930189, 12.50000000000000000, 5.867463478539781896 ) ) ;
#66313 = ORIENTED_EDGE ( 'NONE', *, *, #67788, .T. ) ;
#66314 = FACE_OUTER_BOUND ( 'NONE', #111035, .T. ) ;
#66315 = CARTESIAN_POINT ( 'NONE',  ( -12.89999999999999325, 2.500000000000000000, -3.637306695894647390 ) ) ;
#66316 = ORIENTED_EDGE ( 'NONE', *, *, #95695, .T. ) ;
#66317 = AXIS2_PLACEMENT_3D ( 'NONE', #7028, #118938, #109099 ) ;
#66318 = EDGE_CURVE ( 'NONE', #20664, #107019, #25592, .T. ) ;
#66319 = DIRECTION ( 'NONE',  ( 0.000000000000000000, 0.000000000000000000, 1.000000000000000000 ) ) ;
#66320 = DIRECTION ( 'NONE',  ( 0.000000000000000000, -0.9999939076577903929, 0.003490651415223739937 ) ) ;
#66321 = AXIS2_PLACEMENT_3D ( 'NONE', #76690, #106777, #98251 ) ;
#66322 = CARTESIAN_POINT ( 'NONE',  ( 4.599999999999938360, 12.50000000000000000, -2.276824562219559311E-15 ) ) ;
#66323 = DIRECTION ( 'NONE',  ( 0.000000000000000000, 1.000000000000000000, 0.000000000000000000 ) ) ;
#66324 = DIRECTION ( 'NONE',  ( 0.000000000000000000, 1.000000000000000000, 0.000000000000000000 ) ) ;
#66325 = FACE_OUTER_BOUND ( 'NONE', #43388, .T. ) ;
#66327 = AXIS2_PLACEMENT_3D ( 'NONE', #89666, #111212, #22874 ) ;
#66326 = AXIS2_PLACEMENT_3D ( 'NONE', #31194, #71099, #21349 ) ;
#66328 = CONICAL_SURFACE ( 'NONE', #1576, 0.1000000000000002554, 0.003490658503988666988 ) ;
#66329 = ORIENTED_EDGE ( 'NONE', *, *, #87920, .F. ) ;
#66330 = ORIENTED_EDGE ( 'NONE', *, *, #86154, .T. ) ;
#66331 = EDGE_LOOP ( 'NONE', ( #44648, #60391, #32679, #34841 ) ) ;
#66332 = EDGE_LOOP ( 'NONE', ( #45199, #14154, #76696, #123468, #15780, #84507 ) ) ;
#66333 = CARTESIAN_POINT ( 'NONE',  ( 6.649999999999930189, 2.500000000000000000, -2.957883832488653830 ) ) ;
#66334 = CARTESIAN_POINT ( 'NONE',  ( 10.39999999999991509, 12.50000000000000000, 0.6928203230275494784 ) ) ;
#66335 = DIRECTION ( 'NONE',  ( -4.274815082592931898E-19, -0.9999939076577903929, -0.003490651415223739937 ) ) ;
#66336 = ORIENTED_EDGE ( 'NONE', *, *, #35735, .F. ) ;
#66337 = FACE_BOUND ( 'NONE', #33733, .T. ) ;
#66338 = DIRECTION ( 'NONE',  ( 0.000000000000000000, 1.000000000000000000, 0.000000000000000000 ) ) ;
#66339 = DIRECTION ( 'NONE',  ( 0.000000000000000000, 1.000000000000000000, 0.000000000000000000 ) ) ;
#66340 = CARTESIAN_POINT ( 'NONE',  ( -2.500000000000030642, 2.500000000000000000, -0.6928203230275541413 ) ) ;
#66341 = DIRECTION ( 'NONE',  ( 0.000000000000000000, 0.000000000000000000, -1.000000000000000000 ) ) ;
#66342 = DIRECTION ( 'NONE',  ( 0.000000000000000000, 1.000000000000000000, 0.000000000000000000 ) ) ;
#66343 = VECTOR ( 'NONE', #48489, 1000.000000000000000 ) ;
#66344 = CARTESIAN_POINT ( 'NONE',  ( -4.999999999999986677, 2.500000000000000000, -2.276824562219559311E-15 ) ) ;
#66345 = DIRECTION ( 'NONE',  ( 0.000000000000000000, -0.9999939076577903929, 0.003490651415223739937 ) ) ;
#66346 = CARTESIAN_POINT ( 'NONE',  ( 8.749999999999920064, 2.500000000000000000, 5.802370205355744659 ) ) ;
#66347 = CARTESIAN_POINT ( 'NONE',  ( -12.04999999999999716, 2.500000000000000000, -2.165063509461097713 ) ) ;
#66348 = AXIS2_PLACEMENT_3D ( 'NONE', #104367, #22125, #91478 ) ;
#66349 = AXIS2_PLACEMENT_3D ( 'NONE', #118297, #9633, #68545 ) ;
#66350 = PLANE ( 'NONE',  #77324 ) ;
#66351 = EDGE_CURVE ( 'NONE', #41444, #128319, #90435, .T. ) ;
#66352 = ORIENTED_EDGE ( 'NONE', *, *, #6545, .F. ) ;
#66354 = ORIENTED_EDGE ( 'NONE', *, *, #61346, .T. ) ;
#66353 = CONICAL_SURFACE ( 'NONE', #11978, 0.09999999999999999167, 0.003490658503988666988 ) ;
#66355 = ORIENTED_EDGE ( 'NONE', *, *, #125512, .T. ) ;
#66356 = EDGE_LOOP ( 'NONE', ( #63879, #128950 ) ) ;
#66357 = CARTESIAN_POINT ( 'NONE',  ( -7.500000000000001776, 1.500000000000000000, -9.999999999999998224 ) ) ;
#66358 = ORIENTED_EDGE ( 'NONE', *, *, #123422, .F. ) ;
#66359 = DIRECTION ( 'NONE',  ( 0.000000000000000000, -0.9999939076577903929, 0.003490651415223739937 ) ) ;
#66360 = ORIENTED_EDGE ( 'NONE', *, *, #101717, .T. ) ;
#66361 = VERTEX_POINT ( 'NONE', #15542 ) ;
#66363 = AXIS2_PLACEMENT_3D ( 'NONE', #19325, #79559, #80207 ) ;
#66362 = LINE ( 'NONE', #5497, #108572 ) ;
#66364 = EDGE_CURVE ( 'NONE', #87143, #19500, #23651, .T. ) ;
#66365 = VECTOR ( 'NONE', #101018, 1000.000000000000000 ) ;
#66366 = VECTOR ( 'NONE', #11715, 1000.000000000000000 ) ;
#66368 = CARTESIAN_POINT ( 'NONE',  ( 1.249999999999953815, 12.50000000000000000, -2.857883832488653741 ) ) ;
#66367 = PRODUCT_DEFINITION_CONTEXT ( 'detailed design', #58082, 'design' ) ;
#66369 = CARTESIAN_POINT ( 'NONE',  ( -8.100000000000013856, 2.500000000000000000, 0.3464101615137736845 ) ) ;
#66370 = DIRECTION ( 'NONE',  ( -0.000000000000000000, 1.000000000000000000, -0.000000000000000000 ) ) ;
#66371 = CARTESIAN_POINT ( 'NONE',  ( 13.74999999999989875, 2.500000000000000000, 1.372243186433545370 ) ) ;
#66372 = ADVANCED_FACE ( 'NONE', ( #36511 ), #92612, .T. ) ;
#66373 = CONICAL_SURFACE ( 'NONE', #24523, 0.1000000000000002554, 0.003490658503988666988 ) ;
#66374 = ADVANCED_FACE ( 'NONE', ( #46967 ), #65408, .T. ) ;
#66375 = ORIENTED_EDGE ( 'NONE', *, *, #38047, .T. ) ;
#66376 = ORIENTED_EDGE ( 'NONE', *, *, #76978, .T. ) ;
#66378 = CONICAL_SURFACE ( 'NONE', #53762, 0.09999999999999982514, 0.003490658503988666988 ) ;
#66377 = AXIS2_PLACEMENT_3D ( 'NONE', #17255, #106945, #118712 ) ;
#66379 = VERTEX_POINT ( 'NONE', #55490 ) ;
#66380 = VERTEX_POINT ( 'NONE', #75126 ) ;
#66381 = EDGE_CURVE ( 'NONE', #40041, #119267, #88374, .T. ) ;
#66382 = DIRECTION ( 'NONE',  ( 0.000000000000000000, 0.000000000000000000, 1.000000000000000000 ) ) ;
#66383 = ORIENTED_EDGE ( 'NONE', *, *, #45695, .F. ) ;
#66384 = EDGE_CURVE ( 'NONE', #96534, #44118, #7008, .T. ) ;
#66385 = EDGE_LOOP ( 'NONE', ( #74919, #48662, #13893, #19794 ) ) ;
#66386 = DIRECTION ( 'NONE',  ( 0.000000000000000000, 1.000000000000000000, 0.000000000000000000 ) ) ;
#66387 = CARTESIAN_POINT ( 'NONE',  ( 145.7653593504141725, 2.500000000000000000, -3.576063159858998475 ) ) ;
#66388 = DIRECTION ( 'NONE',  ( 0.000000000000000000, 0.000000000000000000, -1.000000000000000000 ) ) ;
#66389 = FACE_OUTER_BOUND ( 'NONE', #87224, .T. ) ;
#66390 = DIRECTION ( 'NONE',  ( 0.000000000000000000, 1.000000000000000000, 0.000000000000000000 ) ) ;
#66391 = DIRECTION ( 'NONE',  ( 0.000000000000000000, 0.000000000000000000, 1.000000000000000000 ) ) ;
#66392 = ORIENTED_EDGE ( 'NONE', *, *, #86523, .T. ) ;
#66393 = FACE_OUTER_BOUND ( 'NONE', #23513, .T. ) ;
#66394 = ORIENTED_EDGE ( 'NONE', *, *, #87502, .T. ) ;
#66395 = DIRECTION ( 'NONE',  ( 0.000000000000000000, 0.000000000000000000, 1.000000000000000000 ) ) ;
#66396 = ORIENTED_EDGE ( 'NONE', *, *, #7943, .T. ) ;
#66397 = DIRECTION ( 'NONE',  ( 0.000000000000000000, 1.000000000000000000, 0.000000000000000000 ) ) ;
#66398 = FACE_OUTER_BOUND ( 'NONE', #19766, .T. ) ;
#66399 = ORIENTED_EDGE ( 'NONE', *, *, #581, .T. ) ;
#66400 = CARTESIAN_POINT ( 'NONE',  ( 4.349999999999940137, 2.500000000000000000, -2.511473670974877948 ) ) ;
#66401 = DIRECTION ( 'NONE',  ( -0.000000000000000000, 1.000000000000000000, -0.000000000000000000 ) ) ;
#66402 = ORIENTED_EDGE ( 'NONE', *, *, #63345, .T. ) ;
#66403 = AXIS2_PLACEMENT_3D ( 'NONE', #84887, #62688, #124171 ) ;
#66404 = EDGE_CURVE ( 'NONE', #44450, #129161, #98853, .T. ) ;
#66405 = AXIS2_PLACEMENT_3D ( 'NONE', #28953, #69493, #28299 ) ;
#66406 = CARTESIAN_POINT ( 'NONE',  ( -2.300000000000032685, 12.50000000000000000, -0.3464101615137783474 ) ) ;
#66407 = ORIENTED_EDGE ( 'NONE', *, *, #20089, .T. ) ;
#66408 = ORIENTED_EDGE ( 'NONE', *, *, #112879, .T. ) ;
#66409 = FACE_OUTER_BOUND ( 'NONE', #18977, .T. ) ;
#66410 = FACE_OUTER_BOUND ( 'NONE', #58342, .T. ) ;
#66411 = CARTESIAN_POINT ( 'NONE',  ( 186.0052083336747444, -6.551208109652278289, 3.782341765624995134 ) ) ;
#66412 = LINE ( 'NONE', #36343, #57552 ) ;
#66414 = EDGE_CURVE ( 'NONE', #27277, #56832, #8753, .T. ) ;
#66413 = CIRCLE ( 'NONE', #14168, 0.09999999999999999167 ) ;
#66415 = AXIS2_PLACEMENT_3D ( 'NONE', #87779, #58355, #38056 ) ;
#66416 = CARTESIAN_POINT ( 'NONE',  ( 6.049999999999934097, 12.50000000000000000, 6.148780366869520897 ) ) ;
#66417 = DIRECTION ( 'NONE',  ( -0.000000000000000000, -1.000000000000000000, -0.000000000000000000 ) ) ;
#66418 = EDGE_CURVE ( 'NONE', #74873, #52167, #35851, .T. ) ;
#66419 = EDGE_CURVE ( 'NONE', #103260, #6628, #36189, .T. ) ;
#66420 = EDGE_CURVE ( 'NONE', #125657, #93435, #84941, .T. ) ;
#66421 = ORIENTED_EDGE ( 'NONE', *, *, #69783, .T. ) ;
#66422 = DIRECTION ( 'NONE',  ( -0.000000000000000000, 1.000000000000000000, -0.000000000000000000 ) ) ;
#66423 = CIRCLE ( 'NONE', #3728, 0.1000000000000002554 ) ;
#66424 = ORIENTED_EDGE ( 'NONE', *, *, #12454, .F. ) ;
#66425 = EDGE_CURVE ( 'NONE', #45263, #125434, #86215, .T. ) ;
#66426 = CONICAL_SURFACE ( 'NONE', #83173, 0.1000000000000002554, 0.003490658503988666988 ) ;
#66427 = CARTESIAN_POINT ( 'NONE',  ( -4.076600168545496672E-14, 2.500000000000000000, -4.922947341949753586 ) ) ;
#66428 = CARTESIAN_POINT ( 'NONE',  ( 9.799999999999918998, 12.50000000000000000, -0.3464101615137782364 ) ) ;
#66429 = DIRECTION ( 'NONE',  ( -0.000000000000000000, -1.000000000000000000, -0.000000000000000000 ) ) ;
#66430 = ORIENTED_EDGE ( 'NONE', *, *, #48525, .T. ) ;
#66431 = ADVANCED_FACE ( 'NONE', ( #86870 ), #24740, .T. ) ;
#66432 = CONICAL_SURFACE ( 'NONE', #33007, 0.1000000000000002554, 0.003490658503988666988 ) ;
#66433 = EDGE_CURVE ( 'NONE', #45043, #32461, #111364, .T. ) ;
#66434 = DIRECTION ( 'NONE',  ( 0.000000000000000000, 0.000000000000000000, 1.000000000000000000 ) ) ;
#66435 = CARTESIAN_POINT ( 'NONE',  ( 7.949999999999922018, 2.500000000000000000, 6.495190528383297135 ) ) ;
#66436 = VECTOR ( 'NONE', #59812, 1000.000000000000000 ) ;
#66437 = AXIS2_PLACEMENT_3D ( 'NONE', #89877, #29048, #88597 ) ;
#66438 = EDGE_LOOP ( 'NONE', ( #305, #116845, #29844, #33261 ) ) ;
#66439 = AXIS2_PLACEMENT_3D ( 'NONE', #124348, #56233, #16922 ) ;
#66440 = DIRECTION ( 'NONE',  ( 0.000000000000000000, 1.000000000000000000, 0.000000000000000000 ) ) ;
#66441 = CIRCLE ( 'NONE', #114558, 0.06509327318403745899 ) ;
#66442 = VERTEX_POINT ( 'NONE', #127455 ) ;
#66443 = EDGE_LOOP ( 'NONE', ( #98854, #5079, #60929, #108035 ) ) ;
#66444 = CARTESIAN_POINT ( 'NONE',  ( 3.099999999999943245, 2.500000000000000000, 3.983716857408420076 ) ) ;
#66445 = AXIS2_PLACEMENT_3D ( 'NONE', #114799, #106278, #106908 ) ;
#66446 = EDGE_LOOP ( 'NONE', ( #119505, #94394 ) ) ;
#66447 = DIRECTION ( 'NONE',  ( -0.000000000000000000, 1.000000000000000000, -0.000000000000000000 ) ) ;
#66448 = CARTESIAN_POINT ( 'NONE',  ( -11.64999999999999680, 12.50000000000000000, 1.537336459617582918 ) ) ;
#66449 = CONICAL_SURFACE ( 'NONE', #83103, 0.1000000000000002554, 0.003490658503988666988 ) ;
#66450 = DIRECTION ( 'NONE',  ( 0.000000000000000000, 1.000000000000000000, 0.000000000000000000 ) ) ;
#66451 = ORIENTED_EDGE ( 'NONE', *, *, #81448, .F. ) ;
#66452 = AXIS2_PLACEMENT_3D ( 'NONE', #75155, #42487, #104603 ) ;
#66453 = FACE_BOUND ( 'NONE', #37258, .T. ) ;
#66455 = VERTEX_POINT ( 'NONE', #8945 ) ;
#66454 = DIRECTION ( 'NONE',  ( 0.000000000000000000, -0.9999939076577903929, 0.003490651415223739937 ) ) ;
#66456 = LINE ( 'NONE', #16693, #102918 ) ;
#66457 = CARTESIAN_POINT ( 'NONE',  ( 11.64999999999990443, 12.50000000000000000, 1.537336459617582918 ) ) ;
#66458 = ORIENTED_EDGE ( 'NONE', *, *, #61067, .T. ) ;
#66460 = CIRCLE ( 'NONE', #64322, 0.1000000000000002554 ) ;
#66459 = CONICAL_SURFACE ( 'NONE', #124965, 0.09999999999999982514, 0.003490658503988666988 ) ;
#66462 = VERTEX_POINT ( 'NONE', #88135 ) ;
#66461 = EDGE_CURVE ( 'NONE', #11512, #45894, #50846, .T. ) ;
#66463 = VERTEX_POINT ( 'NONE', #109068 ) ;
#66464 = CARTESIAN_POINT ( 'NONE',  ( -6.050000000000017586, 12.50000000000000000, 6.148780366869520009 ) ) ;
#66465 = PLANE ( 'NONE',  #93805 ) ;
#66466 = DIRECTION ( 'NONE',  ( 0.000000000000000000, 1.000000000000000000, 0.000000000000000000 ) ) ;
#66467 = FACE_BOUND ( 'NONE', #108462, .T. ) ;
#66468 = EDGE_LOOP ( 'NONE', ( #49843, #36031 ) ) ;
#66469 = CARTESIAN_POINT ( 'NONE',  ( 186.5260416670080588, -6.551208109652273848, -3.782341765625003571 ) ) ;
#66470 = CARTESIAN_POINT ( 'NONE',  ( 7.899999999999924860, 12.50000000000000000, -3.637306695894650055 ) ) ;
#66471 = DIRECTION ( 'NONE',  ( 0.000000000000000000, -0.000000000000000000, 1.000000000000000000 ) ) ;
#66472 = EDGE_CURVE ( 'NONE', #118333, #38253, #129416, .T. ) ;
#66473 = FACE_OUTER_BOUND ( 'NONE', #125643, .T. ) ;
#66474 = DIRECTION ( 'NONE',  ( -0.000000000000000000, -1.000000000000000000, -0.000000000000000000 ) ) ;
#66475 = DIRECTION ( 'NONE',  ( 0.000000000000000000, 0.000000000000000000, 1.000000000000000000 ) ) ;
#66476 = LINE ( 'NONE', #44256, #109823 ) ;
#66477 = DIRECTION ( 'NONE',  ( 0.000000000000000000, 0.000000000000000000, -1.000000000000000000 ) ) ;
#66478 = CARTESIAN_POINT ( 'NONE',  ( 1.049999999999954081, 12.50000000000000000, -6.148780366869526226 ) ) ;
#66479 = ORIENTED_EDGE ( 'NONE', *, *, #127465, .T. ) ;
#66480 = ORIENTED_EDGE ( 'NONE', *, *, #107143, .T. ) ;
#66481 = EDGE_LOOP ( 'NONE', ( #42530, #64014, #108091, #41257 ) ) ;
#66482 = AXIS2_PLACEMENT_3D ( 'NONE', #21614, #52354, #30807 ) ;
#66483 = ORIENTED_EDGE ( 'NONE', *, *, #65948, .T. ) ;
#66484 = ORIENTED_EDGE ( 'NONE', *, *, #115750, .T. ) ;
#66485 = DIRECTION ( 'NONE',  ( 0.000000000000000000, 1.000000000000000000, 0.000000000000000000 ) ) ;
#66486 = CIRCLE ( 'NONE', #10070, 0.06509327318403745899 ) ;
#66487 = DIRECTION ( 'NONE',  ( 0.000000000000000000, 1.000000000000000000, 0.000000000000000000 ) ) ;
#66488 = ORIENTED_EDGE ( 'NONE', *, *, #14346, .F. ) ;
#66489 = FACE_BOUND ( 'NONE', #97997, .T. ) ;
#66490 = CARTESIAN_POINT ( 'NONE',  ( 10.59999999999990905, 12.50000000000000000, 3.983716857408420076 ) ) ;
#66491 = CIRCLE ( 'NONE', #62310, 0.09999999999999982514 ) ;
#66492 = AXIS2_PLACEMENT_3D ( 'NONE', #81267, #83205, #92354 ) ;
#66493 = CARTESIAN_POINT ( 'NONE',  ( 185.5312500006828031, 9.429780353434619030E-16, -7.700000000000000178 ) ) ;
#66494 = DIRECTION ( 'NONE',  ( 0.000000000000000000, 0.000000000000000000, 1.000000000000000000 ) ) ;
#66495 = FACE_OUTER_BOUND ( 'NONE', #40930, .T. ) ;
#66496 = DIRECTION ( 'NONE',  ( -4.274815082592931898E-19, -0.9999939076577903929, -0.003490651415223739937 ) ) ;
#66497 = ORIENTED_EDGE ( 'NONE', *, *, #24864, .T. ) ;
#66498 = FACE_OUTER_BOUND ( 'NONE', #36676, .T. ) ;
#66499 = CIRCLE ( 'NONE', #10082, 0.1000000000000002554 ) ;
#66500 = B_SPLINE_CURVE_WITH_KNOTS ( 'NONE', 3,
 ( #49442, #78902, #20612, #71000, #69052, #19299, #101096, #48139 ),
 .UNSPECIFIED., .F., .F.,
 ( 4, 2, 2, 4 ),
 ( -1.045402497787284507E-05, 0.001241257413634800407, 0.001867113132941136070, 0.002492968852247471733 ),
 .UNSPECIFIED. ) ;
#66501 = ORIENTED_EDGE ( 'NONE', *, *, #119489, .T. ) ;
#66502 = EDGE_LOOP ( 'NONE', ( #53207, #53044, #77546, #108581 ) ) ;
#66503 = ORIENTED_EDGE ( 'NONE', *, *, #52785, .F. ) ;
#66504 = DIRECTION ( 'NONE',  ( 0.000000000000000000, -1.846105847067148515E-16, -1.000000000000000000 ) ) ;
#66505 = FACE_OUTER_BOUND ( 'NONE', #33972, .T. ) ;
#66506 = CARTESIAN_POINT ( 'NONE',  ( 4.149999999999936406, 2.500000000000000000, 6.595190528383296780 ) ) ;
#66507 = ORIENTED_EDGE ( 'NONE', *, *, #79669, .T. ) ;
#66508 = CARTESIAN_POINT ( 'NONE',  ( 130.5000000000000000, 0.5000000000000000000, -7.500000000000001776 ) ) ;
#66510 = ADVANCED_FACE ( 'NONE', ( #58711 ), #109324, .T. ) ;
#66509 = AXIS2_PLACEMENT_3D ( 'NONE', #127532, #107880, #27372 ) ;
#66511 = CARTESIAN_POINT ( 'NONE',  ( 187.5000000000000000, 9.429780353434619030E-16, -7.700000000000000178 ) ) ;
#66512 = DIRECTION ( 'NONE',  ( 0.000000000000000000, 1.000000000000000000, 0.000000000000000000 ) ) ;
#66513 = CARTESIAN_POINT ( 'NONE',  ( 186.4843750003414016, -8.734944146203032389, -1.604583208406768146E-15 ) ) ;
#66514 = DIRECTION ( 'NONE',  ( 0.000000000000000000, 1.000000000000000000, 0.000000000000000000 ) ) ;
#66515 = EDGE_CURVE ( 'NONE', #87716, #93847, #80093, .T. ) ;
#66516 = CARTESIAN_POINT ( 'NONE',  ( -4.250072516143177381E-14, 12.50000000000000000, -3.637306695894650055 ) ) ;
#66517 = EDGE_CURVE ( 'NONE', #11592, #18164, #42453, .T. ) ;
#66518 = VERTEX_POINT ( 'NONE', #40373 ) ;
#66519 = CARTESIAN_POINT ( 'NONE',  ( -4.400000000000025224, 12.50000000000000000, -0.3464101615137783474 ) ) ;
#66520 = CIRCLE ( 'NONE', #26827, 0.1000000000000002554 ) ;
#66521 = VERTEX_POINT ( 'NONE', #37783 ) ;
#66522 = VERTEX_POINT ( 'NONE', #77686 ) ;
#66523 = STYLED_ITEM ( 'NONE', ( #95044 ), #122749 ) ;
#66524 = DIRECTION ( 'NONE',  ( 0.000000000000000000, 0.000000000000000000, 1.000000000000000000 ) ) ;
#66525 = EDGE_CURVE ( 'NONE', #37178, #17512, #110379, .T. ) ;
#66526 = ADVANCED_FACE ( 'NONE', ( #109748 ), #27851, .T. ) ;
#66527 = LINE ( 'NONE', #116911, #101070 ) ;
#66528 = FACE_OUTER_BOUND ( 'NONE', #97471, .T. ) ;
#66529 = ADVANCED_FACE ( 'NONE', ( #39740 ), #128117, .T. ) ;
#66530 = ORIENTED_EDGE ( 'NONE', *, *, #49863, .F. ) ;
#66531 = VECTOR ( 'NONE', #7777, 1000.000000000000000 ) ;
#66532 = VERTEX_POINT ( 'NONE', #7658 ) ;
#66533 = FACE_OUTER_BOUND ( 'NONE', #51208, .T. ) ;
#66534 = CIRCLE ( 'NONE', #14299, 0.06509327318403743123 ) ;
#66535 = FACE_OUTER_BOUND ( 'NONE', #26414, .T. ) ;
#66536 = DIRECTION ( 'NONE',  ( 0.000000000000000000, 0.000000000000000000, 1.000000000000000000 ) ) ;
#66537 = EDGE_LOOP ( 'NONE', ( #3165, #127989 ) ) ;
#66538 = VERTEX_POINT ( 'NONE', #80292 ) ;
#66539 = DIRECTION ( 'NONE',  ( 0.000000000000000000, 0.000000000000000000, 1.000000000000000000 ) ) ;
#66540 = AXIS2_PLACEMENT_3D ( 'NONE', #101619, #42052, #102261 ) ;
#66541 = ORIENTED_EDGE ( 'NONE', *, *, #21998, .F. ) ;
#66542 = DIRECTION ( 'NONE',  ( -0.000000000000000000, 1.000000000000000000, -0.000000000000000000 ) ) ;
#66543 = CARTESIAN_POINT ( 'NONE',  ( 179.5000000000000000, -1.375000000000002442, -6.000000000000000888 ) ) ;
#66544 = VERTEX_POINT ( 'NONE', #120211 ) ;
#66545 = DIRECTION ( 'NONE',  ( 0.000000000000000000, 0.000000000000000000, -1.000000000000000000 ) ) ;
#66546 = DIRECTION ( 'NONE',  ( 0.000000000000000000, 1.000000000000000000, 0.000000000000000000 ) ) ;
#66547 = DIRECTION ( 'NONE',  ( -0.000000000000000000, -1.000000000000000000, -0.000000000000000000 ) ) ;
#66548 = AXIS2_PLACEMENT_3D ( 'NONE', #4015, #52473, #113329 ) ;
#66549 = CARTESIAN_POINT ( 'NONE',  ( 3.149999999999946176, 2.500000000000000000, -6.941600689897077459 ) ) ;
#66550 = ORIENTED_EDGE ( 'NONE', *, *, #60918, .F. ) ;
#66551 = CARTESIAN_POINT ( 'NONE',  ( 11.69999999999990870, 2.500000000000000000, 4.330127018922196314 ) ) ;
#66552 = AXIS2_PLACEMENT_3D ( 'NONE', #13584, #112461, #22801 ) ;
#66553 = CARTESIAN_POINT ( 'NONE',  ( -3.750000000000031086, 12.50000000000000000, -5.737276932171712751 ) ) ;
#66554 = VERTEX_POINT ( 'NONE', #97982 ) ;
#66555 = ORIENTED_EDGE ( 'NONE', *, *, #56637, .F. ) ;
#66556 = CARTESIAN_POINT ( 'NONE',  ( 184.7135416670080872, 4.367472073101518859, -7.564683531249999149 ) ) ;
#66557 = DIRECTION ( 'NONE',  ( 0.000000000000000000, 0.000000000000000000, -1.000000000000000000 ) ) ;
#66558 = CARTESIAN_POINT ( 'NONE',  ( 14.34999999999989662, 12.50000000000000000, 2.576566944158910744 ) ) ;
#66559 = LINE ( 'NONE', #127436, #85614 ) ;
#66560 = DIRECTION ( 'NONE',  ( 1.000000000000000000, 0.000000000000000000, 0.000000000000000000 ) ) ;
#66561 = FACE_OUTER_BOUND ( 'NONE', #94450, .T. ) ;
#66562 = CARTESIAN_POINT ( 'NONE',  ( 0.8499999999999536815, 12.50000000000000000, 5.802370205355744659 ) ) ;
#66563 = DIRECTION ( 'NONE',  ( -0.000000000000000000, 1.000000000000000000, -0.000000000000000000 ) ) ;
#66564 = LINE ( 'NONE', #76409, #2413 ) ;
#66565 = EDGE_CURVE ( 'NONE', #94907, #82804, #54946, .T. ) ;
#66566 = AXIS2_PLACEMENT_3D ( 'NONE', #110116, #139, #122516 ) ;
#66567 = EDGE_CURVE ( 'NONE', #70903, #46827, #4755, .T. ) ;
#66568 = ADVANCED_FACE ( 'NONE', ( #48906 ), #71678, .T. ) ;
#66569 = DIRECTION ( 'NONE',  ( 0.000000000000000000, 1.000000000000000000, 0.000000000000000000 ) ) ;
#66570 = VERTEX_POINT ( 'NONE', #99930 ) ;
#66571 = AXIS2_PLACEMENT_3D ( 'NONE', #101531, #2660, #43910 ) ;
#66572 = CONICAL_SURFACE ( 'NONE', #37353, 0.1000000000000002554, 0.003490658503988666988 ) ;
#66573 = ORIENTED_EDGE ( 'NONE', *, *, #53719, .F. ) ;
#66574 = CONICAL_SURFACE ( 'NONE', #70787, 0.09999999999999982514, 0.003490658503988666988 ) ;
#66575 = CARTESIAN_POINT ( 'NONE',  ( 9.399999999999918643, 2.500000000000000000, 0.3464101615137736845 ) ) ;
#66576 = EDGE_CURVE ( 'NONE', #84673, #76977, #31987, .T. ) ;
#66577 = ORIENTED_EDGE ( 'NONE', *, *, #105381, .T. ) ;
#66578 = EDGE_CURVE ( 'NONE', #122820, #23588, #69820, .T. ) ;
#66579 = CARTESIAN_POINT ( 'NONE',  ( 14.14999999999989377, 2.500000000000000000, -2.857883832488653741 ) ) ;
#66580 = DIRECTION ( 'NONE',  ( -0.000000000000000000, 1.000000000000000000, -0.000000000000000000 ) ) ;
#66581 = CARTESIAN_POINT ( 'NONE',  ( 12.89999999999989910, 2.500000000000000000, 0.6928203230275494784 ) ) ;
#66583 = EDGE_CURVE ( 'NONE', #47691, #90584, #117716, .T. ) ;
#66582 = CONICAL_SURFACE ( 'NONE', #129318, 0.1000000000000000472, 0.003490658503988666988 ) ;
#66584 = VERTEX_POINT ( 'NONE', #128765 ) ;
#66586 = EDGE_CURVE ( 'NONE', #40907, #56626, #113536, .T. ) ;
#66585 = AXIS2_PLACEMENT_3D ( 'NONE', #81212, #80571, #82507 ) ;
#66587 = DIRECTION ( 'NONE',  ( 0.000000000000000000, 1.000000000000000000, 0.000000000000000000 ) ) ;
#66588 = AXIS2_PLACEMENT_3D ( 'NONE', #114571, #75299, #124412 ) ;
#66589 = ADVANCED_FACE ( 'NONE', ( #70461 ), #73824, .T. ) ;
#66590 = CARTESIAN_POINT ( 'NONE',  ( -8.100000000000010303, 2.500000000000000000, 3.983716857408420964 ) ) ;
#66592 = VERTEX_POINT ( 'NONE', #120848 ) ;
#66591 = DIRECTION ( 'NONE',  ( -0.000000000000000000, -1.000000000000000000, -0.000000000000000000 ) ) ;
#66593 = EDGE_CURVE ( 'NONE', #91689, #30841, #121844, .T. ) ;
#66594 = CONICAL_SURFACE ( 'NONE', #10175, 0.09999999999999982514, 0.003490658503988666988 ) ;
#66595 = CARTESIAN_POINT ( 'NONE',  ( -4.550000000000022915, 2.500000000000000000, -2.165063509461101710 ) ) ;
#66596 = VERTEX_POINT ( 'NONE', #52746 ) ;
#66597 = AXIS2_PLACEMENT_3D ( 'NONE', #54344, #46450, #126961 ) ;
#66598 = ORIENTED_EDGE ( 'NONE', *, *, #126748, .T. ) ;
#66599 = ORIENTED_EDGE ( 'NONE', *, *, #19811, .F. ) ;
#66600 = EDGE_LOOP ( 'NONE', ( #124849, #720 ) ) ;
#66601 = LINE ( 'NONE', #28627, #92901 ) ;
#66602 = CARTESIAN_POINT ( 'NONE',  ( 1.049999999999952971, 2.500000000000000000, 6.148780366869520897 ) ) ;
#66603 = DIRECTION ( 'NONE',  ( 0.000000000000000000, 0.000000000000000000, 1.000000000000000000 ) ) ;
#66604 = DIRECTION ( 'NONE',  ( 0.000000000000000000, 0.000000000000000000, -1.000000000000000000 ) ) ;
#66605 = CIRCLE ( 'NONE', #100069, 0.06509327318403745899 ) ;
#66606 = ORIENTED_EDGE ( 'NONE', *, *, #44276, .F. ) ;
#66607 = CARTESIAN_POINT ( 'NONE',  ( 6.649999999999929301, 12.50000000000000000, -2.165063509461101710 ) ) ;
#66608 = ORIENTED_EDGE ( 'NONE', *, *, #104767, .T. ) ;
#66609 = CIRCLE ( 'NONE', #14372, 0.06509327318403743123 ) ;
#66610 = DIRECTION ( 'NONE',  ( -1.000000000000000000, -0.000000000000000000, -0.000000000000000000 ) ) ;
#66611 = CARTESIAN_POINT ( 'NONE',  ( 5.199999999999931788, 2.500000000000000000, 4.676537180435972552 ) ) ;
#66612 = CARTESIAN_POINT ( 'NONE',  ( 105.6184301395928031, 9.000000000000001776, -1.375000000000000888 ) ) ;
#66613 = DIRECTION ( 'NONE',  ( -4.274815082592931898E-19, -0.9999939076577903929, -0.003490651415223739937 ) ) ;
#66614 = EDGE_LOOP ( 'NONE', ( #64362, #128599, #6225, #51285 ) ) ;
#66615 =( GEOMETRIC_REPRESENTATION_CONTEXT ( 3 ) GLOBAL_UNCERTAINTY_ASSIGNED_CONTEXT ( ( #114463 ) ) GLOBAL_UNIT_ASSIGNED_CONTEXT ( ( #80562, #33402, #74597 ) ) REPRESENTATION_CONTEXT ( 'NONE', 'WORKASPACE' ) );
#66616 = ORIENTED_EDGE ( 'NONE', *, *, #65033, .T. ) ;
#66617 = ORIENTED_EDGE ( 'NONE', *, *, #120396, .F. ) ;
#66618 = CARTESIAN_POINT ( 'NONE',  ( -7.700000000000010836, 2.500000000000000000, 3.983716857408420964 ) ) ;
#66619 = DIRECTION ( 'NONE',  ( 0.000000000000000000, 1.000000000000000000, 0.000000000000000000 ) ) ;
#66620 = CARTESIAN_POINT ( 'NONE',  ( 1.249999999999952482, 12.50000000000000000, -5.867463478539787225 ) ) ;
#66621 = FACE_BOUND ( 'NONE', #14889, .T. ) ;
#66622 = LINE ( 'NONE', #106549, #55639 ) ;
#66623 = DIRECTION ( 'NONE',  ( 0.000000000000000000, 0.000000000000000000, 1.000000000000000000 ) ) ;
#66624 = DIRECTION ( 'NONE',  ( -0.000000000000000000, 1.000000000000000000, -0.000000000000000000 ) ) ;
#66625 = DIRECTION ( 'NONE',  ( -0.000000000000000000, -1.000000000000000000, -0.000000000000000000 ) ) ;
#66626 = CIRCLE ( 'NONE', #83370, 0.06509327318403745899 ) ;
#66627 = ADVANCED_FACE ( 'NONE', ( #2339 ), #69619, .T. ) ;
#66628 = CARTESIAN_POINT ( 'NONE',  ( 184.3802083336747444, 4.367472073101515306, 7.564683531250000925 ) ) ;
#66629 = DIRECTION ( 'NONE',  ( -1.000000000000000000, -0.000000000000000000, -0.000000000000000000 ) ) ;
#66630 = CARTESIAN_POINT ( 'NONE',  ( -13.34999999999999076, 2.500000000000000000, -1.572243186433547990 ) ) ;
#66631 = CARTESIAN_POINT ( 'NONE',  ( 5.849999999999933920, 2.500000000000000000, 6.495190528383297135 ) ) ;
#66633 = CONICAL_SURFACE ( 'NONE', #47883, 0.1000000000000000472, 0.003490658503988666988 ) ;
#66632 = VECTOR ( 'NONE', #68186, 1000.000000000000000 ) ;
#66634 = EDGE_LOOP ( 'NONE', ( #52673, #39069, #99095, #123288 ) ) ;
#66635 = ORIENTED_EDGE ( 'NONE', *, *, #101145, .F. ) ;
#66636 = ORIENTED_EDGE ( 'NONE', *, *, #3955, .T. ) ;
#66637 = VERTEX_POINT ( 'NONE', #1708 ) ;
#66638 = AXIS2_PLACEMENT_3D ( 'NONE', #59439, #100611, #10927 ) ;
#66639 = CARTESIAN_POINT ( 'NONE',  ( -4.150000000000024336, 12.50000000000000000, 1.407149913249508000 ) ) ;
#66640 = FACE_BOUND ( 'NONE', #12478, .T. ) ;
#66641 = CARTESIAN_POINT ( 'NONE',  ( 13.09999999999989839, 12.50000000000000000, 0.3464101615137735735 ) ) ;
#66642 = DIRECTION ( 'NONE',  ( -4.274815082592931898E-19, -0.9999939076577903929, -0.003490651415223739937 ) ) ;
#66643 = AXIS2_PLACEMENT_3D ( 'NONE', #62117, #13634, #14897 ) ;
#66644 = ORIENTED_EDGE ( 'NONE', *, *, #4002, .T. ) ;
#66645 = FACE_OUTER_BOUND ( 'NONE', #99639, .T. ) ;
#66646 = CARTESIAN_POINT ( 'NONE',  ( 175.5000000000000000, 0.000000000000000000, 0.000000000000000000 ) ) ;
#66647 = ORIENTED_EDGE ( 'NONE', *, *, #67117, .F. ) ;
#66648 = CARTESIAN_POINT ( 'NONE',  ( -8.750000000000010658, 2.500000000000000000, 2.857883832488649301 ) ) ;
#66649 = DIRECTION ( 'NONE',  ( 0.000000000000000000, 0.000000000000000000, 1.000000000000000000 ) ) ;
#66650 = ORIENTED_EDGE ( 'NONE', *, *, #16335, .F. ) ;
#66651 = CONICAL_SURFACE ( 'NONE', #1815, 0.1000000000000002554, 0.003490658503988666988 ) ;
#66652 = DIRECTION ( 'NONE',  ( 0.000000000000000000, 1.000000000000000000, 0.000000000000000000 ) ) ;
#66653 = FACE_OUTER_BOUND ( 'NONE', #120600, .T. ) ;
#66654 = ORIENTED_EDGE ( 'NONE', *, *, #55185, .F. ) ;
#66655 = AXIS2_PLACEMENT_3D ( 'NONE', #41829, #11042, #73206 ) ;
#66656 = EDGE_CURVE ( 'NONE', #80887, #26124, #103071, .T. ) ;
#66657 = LINE ( 'NONE', #38532, #113710 ) ;
#66658 = AXIS2_PLACEMENT_3D ( 'NONE', #45818, #6485, #46440 ) ;
#66659 = CARTESIAN_POINT ( 'NONE',  ( 5.199999999999935341, 12.50000000000000000, -0.3464101615137783474 ) ) ;
#66660 = ORIENTED_EDGE ( 'NONE', *, *, #31802, .F. ) ;
#66661 = DIRECTION ( 'NONE',  ( 0.000000000000000000, 0.000000000000000000, -1.000000000000000000 ) ) ;
#66662 = ORIENTED_EDGE ( 'NONE', *, *, #114151, .T. ) ;
#66663 = ORIENTED_EDGE ( 'NONE', *, *, #599, .T. ) ;
#66664 = ADVANCED_FACE ( 'NONE', ( #92030 ), #90744, .T. ) ;
#66665 = CARTESIAN_POINT ( 'NONE',  ( 0.6499999999999561684, 2.500000000000000000, -2.511473670974877948 ) ) ;
#66666 = EDGE_CURVE ( 'NONE', #51434, #12584, #22665, .T. ) ;
#66667 = ORIENTED_EDGE ( 'NONE', *, *, #51640, .F. ) ;
#66668 = DIRECTION ( 'NONE',  ( 0.000000000000000000, 1.000000000000000000, 0.000000000000000000 ) ) ;
#66669 = CARTESIAN_POINT ( 'NONE',  ( -2.100000000000034284, 12.50000000000000000, -2.385244779468109755E-15 ) ) ;
#66670 = CONICAL_SURFACE ( 'NONE', #91725, 0.1000000000000002554, 0.003490658503988666988 ) ;
#66671 = AXIS2_PLACEMENT_3D ( 'NONE', #94083, #105831, #95374 ) ;
#66672 = ORIENTED_EDGE ( 'NONE', *, *, #46143, .T. ) ;
#66673 = DIRECTION ( 'NONE',  ( 0.000000000000000000, -0.000000000000000000, 1.000000000000000000 ) ) ;
#66674 = PLANE ( 'NONE',  #69162 ) ;
#66675 = FACE_OUTER_BOUND ( 'NONE', #128058, .T. ) ;
#66676 = EDGE_CURVE ( 'NONE', #54499, #49457, #115673, .T. ) ;
#66677 = EDGE_CURVE ( 'NONE', #86613, #74320, #9073, .T. ) ;
#66678 = DIRECTION ( 'NONE',  ( -0.000000000000000000, 1.000000000000000000, -0.000000000000000000 ) ) ;
#66679 = EDGE_CURVE ( 'NONE', #41126, #61697, #94751, .T. ) ;
#66680 = CARTESIAN_POINT ( 'NONE',  ( 10.84999999999990905, 2.500000000000000000, -5.902370205355750521 ) ) ;
#66681 = EDGE_CURVE ( 'NONE', #96385, #3617, #21356, .T. ) ;
#66682 = EDGE_CURVE ( 'NONE', #27458, #117981, #78137, .T. ) ;
#66683 = CARTESIAN_POINT ( 'NONE',  ( 17.50000000000000355, 2.481874935395226078, -3.264429721014347585 ) ) ;
#66684 = AXIS2_PLACEMENT_3D ( 'NONE', #70339, #110262, #70986 ) ;
#66685 = ORIENTED_EDGE ( 'NONE', *, *, #49014, .F. ) ;
#66687 = ORIENTED_EDGE ( 'NONE', *, *, #46214, .T. ) ;
#66686 = AXIS2_PLACEMENT_3D ( 'NONE', #21517, #82384, #122943 ) ;
#66688 = DIRECTION ( 'NONE',  ( 0.000000000000000000, 0.000000000000000000, 1.000000000000000000 ) ) ;
#66689 = CARTESIAN_POINT ( 'NONE',  ( 179.5000000000000000, 0.6250000000000000000, 7.634788798650556707 ) ) ;
#66690 = PLANE ( 'NONE',  #16711 ) ;
#66692 = ORIENTED_EDGE ( 'NONE', *, *, #123717, .F. ) ;
#66691 = EDGE_LOOP ( 'NONE', ( #58892, #12819, #35413, #123106 ) ) ;
#66693 = ORIENTED_EDGE ( 'NONE', *, *, #102018, .F. ) ;
#66694 = EDGE_CURVE ( 'NONE', #77155, #31364, #122158, .T. ) ;
#66695 = DIRECTION ( 'NONE',  ( -0.000000000000000000, -1.000000000000000000, -0.000000000000000000 ) ) ;
#66696 = CARTESIAN_POINT ( 'NONE',  ( -14.99999999999994671, 12.50000000000000000, 0.000000000000000000 ) ) ;
#66697 = ADVANCED_FACE ( 'NONE', ( #101215 ), #21699, .T. ) ;
#66698 = LINE ( 'NONE', #66056, #49837 ) ;
#66699 = DIRECTION ( 'NONE',  ( 0.000000000000000000, 1.000000000000000000, 0.000000000000000000 ) ) ;
#66700 = CARTESIAN_POINT ( 'NONE',  ( 187.0833333333333144, -6.668395609140180369, 3.849999999999994760 ) ) ;
#66701 = DIRECTION ( 'NONE',  ( 0.000000000000000000, 0.000000000000000000, 1.000000000000000000 ) ) ;
#66702 = CARTESIAN_POINT ( 'NONE',  ( -10.00000000000000533, 12.50000000000000000, 4.957854068765711553 ) ) ;
#66703 = CONICAL_SURFACE ( 'NONE', #56240, 0.09999999999999982514, 0.003490658503988666988 ) ;
#66704 = CARTESIAN_POINT ( 'NONE',  ( -12.09999999999999609, 12.50000000000000000, 0.6928203230275535862 ) ) ;
#66705 = CARTESIAN_POINT ( 'NONE',  ( 184.6979166673494603, 6.668395609140176816, 3.850000000000000977 ) ) ;
#66706 = ORIENTED_EDGE ( 'NONE', *, *, #58420, .T. ) ;
#66707 = DIRECTION ( 'NONE',  ( 0.000000000000000000, 0.000000000000000000, -1.000000000000000000 ) ) ;
#66708 = ORIENTED_EDGE ( 'NONE', *, *, #25303, .T. ) ;
#66709 = ORIENTED_EDGE ( 'NONE', *, *, #70743, .T. ) ;
#66710 = CARTESIAN_POINT ( 'NONE',  ( -9.350000000000008527, 2.500000000000000000, -6.941600689897073018 ) ) ;
#66711 = CARTESIAN_POINT ( 'NONE',  ( 3.749999999999978684, 2.500000000000000000, -2.265063509461101798 ) ) ;
#66712 = CONICAL_SURFACE ( 'NONE', #91868, 0.1000000000000002554, 0.003490658503988666988 ) ;
#66713 = DIRECTION ( 'NONE',  ( -0.000000000000000000, 1.000000000000000000, -0.000000000000000000 ) ) ;
#66715 = VECTOR ( 'NONE', #66454, 1000.000000000000000 ) ;
#66714 = CARTESIAN_POINT ( 'NONE',  ( 7.699999999999922018, 2.500000000000000000, 0.2464101615137735679 ) ) ;
#66716 = CARTESIAN_POINT ( 'NONE',  ( -4.150000000000027889, 2.500000000000000000, -6.395190528383301931 ) ) ;
#66717 = LINE ( 'NONE', #48381, #120149 ) ;
#66718 = DIRECTION ( 'NONE',  ( -0.000000000000000000, 1.000000000000000000, -0.000000000000000000 ) ) ;
#66719 = ORIENTED_EDGE ( 'NONE', *, *, #61158, .F. ) ;
#66720 = CARTESIAN_POINT ( 'NONE',  ( 3.149999999999946176, 2.500000000000000000, -6.148780366869526226 ) ) ;
#66721 = EDGE_CURVE ( 'NONE', #62965, #69394, #91384, .T. ) ;
#66722 = EDGE_CURVE ( 'NONE', #27, #110433, #15316, .T. ) ;
#66723 = DIRECTION ( 'NONE',  ( 0.000000000000000000, 1.000000000000000000, 0.000000000000000000 ) ) ;
#66724 = ORIENTED_EDGE ( 'NONE', *, *, #5924, .F. ) ;
#66725 = ORIENTED_EDGE ( 'NONE', *, *, #126969, .F. ) ;
#66726 = EDGE_CURVE ( 'NONE', #92801, #125152, #59272, .T. ) ;
#66728 = AXIS2_PLACEMENT_3D ( 'NONE', #60698, #90783, #10297 ) ;
#66727 = AXIS2_PLACEMENT_3D ( 'NONE', #48904, #126807, #69154 ) ;
#66729 = EDGE_LOOP ( 'NONE', ( #128461, #3463, #84765, #30422 ) ) ;
#66730 = AXIS2_PLACEMENT_3D ( 'NONE', #43505, #4184, #83423 ) ;
#66731 = ORIENTED_EDGE ( 'NONE', *, *, #67880, .F. ) ;
#66732 = ADVANCED_FACE ( 'NONE', ( #119991 ), #18559, .T. ) ;
#66733 = ORIENTED_EDGE ( 'NONE', *, *, #43422, .T. ) ;
#66734 = LINE ( 'NONE', #106662, #115128 ) ;
#66735 = CARTESIAN_POINT ( 'NONE',  ( 11.24999999999990941, 2.500000000000000000, -1.472243186433550122 ) ) ;
#66736 = ADVANCED_FACE ( 'NONE', ( #119331 ), #751, .T. ) ;
#66739 = EDGE_LOOP ( 'NONE', ( #70281, #105313 ) ) ;
#66738 = AXIS2_PLACEMENT_3D ( 'NONE', #79648, #59398, #1088 ) ;
#66737 = AXIS2_PLACEMENT_3D ( 'NONE', #13590, #4395, #84921 ) ;
#66740 = LINE ( 'NONE', #24891, #35998 ) ;
#66741 = DIRECTION ( 'NONE',  ( 0.000000000000000000, -0.9999939076577903929, 0.003490651415223739937 ) ) ;
#66742 = EDGE_CURVE ( 'NONE', #113165, #1374, #80717, .T. ) ;
#66743 = DIRECTION ( 'NONE',  ( 0.000000000000000000, 0.000000000000000000, -1.000000000000000000 ) ) ;
#66744 = ORIENTED_EDGE ( 'NONE', *, *, #33492, .T. ) ;
#66745 = DIRECTION ( 'NONE',  ( 0.000000000000000000, -0.9999939076577903929, 0.003490651415223739937 ) ) ;
#66746 = ADVANCED_FACE ( 'NONE', ( #59811 ), #111474, .T. ) ;
#66747 = DIRECTION ( 'NONE',  ( 0.000000000000000000, 0.000000000000000000, 1.000000000000000000 ) ) ;
#66748 = ORIENTED_EDGE ( 'NONE', *, *, #55536, .F. ) ;
#66749 = ORIENTED_EDGE ( 'NONE', *, *, #109980, .T. ) ;
#66750 = ORIENTED_EDGE ( 'NONE', *, *, #129074, .F. ) ;
#66751 = AXIS2_PLACEMENT_3D ( 'NONE', #117341, #59778, #47357 ) ;
#66752 = DIRECTION ( 'NONE',  ( 0.000000000000000000, 0.000000000000000000, 1.000000000000000000 ) ) ;
#66753 = CARTESIAN_POINT ( 'NONE',  ( 14.34999999999989662, 2.500000000000000000, 1.718653347947321386 ) ) ;
#66754 = CIRCLE ( 'NONE', #33346, 0.06509327318403745899 ) ;
#66755 = ORIENTED_EDGE ( 'NONE', *, *, #103819, .F. ) ;
#66756 = DIRECTION ( 'NONE',  ( -0.000000000000000000, 1.000000000000000000, -0.000000000000000000 ) ) ;
#66757 = DIRECTION ( 'NONE',  ( 0.000000000000000000, 0.000000000000000000, -1.000000000000000000 ) ) ;
#66758 = DIRECTION ( 'NONE',  ( 0.000000000000000000, 0.000000000000000000, -1.000000000000000000 ) ) ;
#66759 = FACE_OUTER_BOUND ( 'NONE', #6176, .T. ) ;
#66760 = EDGE_CURVE ( 'NONE', #121359, #5786, #2815, .T. ) ;
#66761 = VECTOR ( 'NONE', #129087, 1000.000000000000000 ) ;
#66762 = VECTOR ( 'NONE', #18096, 1000.000000000000000 ) ;
#66763 = ORIENTED_EDGE ( 'NONE', *, *, #117779, .T. ) ;
#66764 = CIRCLE ( 'NONE', #116934, 0.06509327318403745899 ) ;
#66765 = DIRECTION ( 'NONE',  ( -0.000000000000000000, 1.000000000000000000, -0.000000000000000000 ) ) ;
#66766 = EDGE_LOOP ( 'NONE', ( #113853, #108809 ) ) ;
#66767 = VERTEX_POINT ( 'NONE', #118043 ) ;
#66768 = ORIENTED_EDGE ( 'NONE', *, *, #46651, .T. ) ;
#66769 = CARTESIAN_POINT ( 'NONE',  ( 12.09999999999990550, 12.50000000000000000, 4.395220292106234439 ) ) ;
#66770 = FACE_BOUND ( 'NONE', #102776, .T. ) ;
#66771 = DIRECTION ( 'NONE',  ( 0.000000000000000000, 0.000000000000000000, 1.000000000000000000 ) ) ;
#66772 = CARTESIAN_POINT ( 'NONE',  ( -5.650000000000023448, 2.500000000000000000, -2.611473670974877592 ) ) ;
#66773 = CARTESIAN_POINT ( 'NONE',  ( 3.749999999999942268, 2.500000000000000000, -5.802370205355749988 ) ) ;
#66774 = VECTOR ( 'NONE', #118100, 1000.000000000000000 ) ;
#66775 = ADVANCED_FACE ( 'NONE', ( #68947 ), #75967, .T. ) ;
#66776 = ORIENTED_EDGE ( 'NONE', *, *, #100827, .T. ) ;
#66777 = PLANE ( 'NONE',  #90246 ) ;
#66778 = DIRECTION ( 'NONE',  ( 0.000000000000000000, -0.9999939076577903929, 0.003490651415223739937 ) ) ;
#66779 = DIRECTION ( 'NONE',  ( 0.000000000000000000, 1.000000000000000000, 0.000000000000000000 ) ) ;
#66780 = CARTESIAN_POINT ( 'NONE',  ( 7.099999999999926814, 2.500000000000000000, 0.09999999999999772959 ) ) ;
#66781 = ORIENTED_EDGE ( 'NONE', *, *, #30492, .F. ) ;
#66782 = CARTESIAN_POINT ( 'NONE',  ( -4.400000000000025224, 2.500000000000000000, 0.2464101615137735679 ) ) ;
#66783 = CARTESIAN_POINT ( 'NONE',  ( 7.099999999999925926, 2.500000000000000000, 0.6928203230275494784 ) ) ;
#66784 = CIRCLE ( 'NONE', #10370, 0.06509327318403745899 ) ;
#66785 = ORIENTED_EDGE ( 'NONE', *, *, #97404, .T. ) ;
#66786 = CARTESIAN_POINT ( 'NONE',  ( 14.14999999999989733, 2.500000000000000000, 1.472243186433545459 ) ) ;
#66787 = ADVANCED_FACE ( 'NONE', ( #70889 ), #8714, .T. ) ;
#66788 = DIRECTION ( 'NONE',  ( 0.000000000000000000, 0.000000000000000000, 1.000000000000000000 ) ) ;
#66789 = FACE_BOUND ( 'NONE', #1158, .T. ) ;
#66790 = CARTESIAN_POINT ( 'NONE',  ( 4.848431875627508880, -2.500000000000000000, -8.943854603337396014 ) ) ;
#66791 = ORIENTED_EDGE ( 'NONE', *, *, #89902, .T. ) ;
#66792 = DIRECTION ( 'NONE',  ( -0.000000000000000000, 1.000000000000000000, -0.000000000000000000 ) ) ;
#66793 = ORIENTED_EDGE ( 'NONE', *, *, #7238, .F. ) ;
#66794 = EDGE_LOOP ( 'NONE', ( #91556, #101992, #80441, #38555 ) ) ;
#66795 = CARTESIAN_POINT ( 'NONE',  ( -1.010904742827955045E-17, 12.50000000000000000, -0.06509327318403743123 ) ) ;
#66796 = CARTESIAN_POINT ( 'NONE',  ( 186.8750000000000284, 8.891194145520236347, 5.444286225454521982E-16 ) ) ;
#66797 = EDGE_LOOP ( 'NONE', ( #126090, #31623 ) ) ;
#66798 = CARTESIAN_POINT ( 'NONE',  ( 12.69999999999990337, 12.50000000000000000, 3.983716857408420076 ) ) ;
#66799 = DIRECTION ( 'NONE',  ( 0.000000000000000000, 0.000000000000000000, -1.000000000000000000 ) ) ;
#66800 = PLANE ( 'NONE',  #11347 ) ;
#66801 = LINE ( 'NONE', #94335, #92383 ) ;
#66802 = VECTOR ( 'NONE', #89237, 1000.000000000000000 ) ;
#66803 = ORIENTED_EDGE ( 'NONE', *, *, #100529, .T. ) ;
#66804 = EDGE_CURVE ( 'NONE', #86025, #34124, #71776, .T. ) ;
#66805 = FACE_OUTER_BOUND ( 'NONE', #64745, .T. ) ;
#66807 = CONICAL_SURFACE ( 'NONE', #6257, 0.1000000000000002554, 0.003490658503988666988 ) ;
#66806 = CIRCLE ( 'NONE', #37600, 0.1000000000000002554 ) ;
#66808 = CARTESIAN_POINT ( 'NONE',  ( 7.099999999999926814, 12.50000000000000000, -2.276824562219559311E-15 ) ) ;
#66809 = DIRECTION ( 'NONE',  ( 0.000000000000000000, 0.000000000000000000, 1.000000000000000000 ) ) ;
#66810 = DIRECTION ( 'NONE',  ( 0.000000000000000000, 0.000000000000000000, 1.000000000000000000 ) ) ;
#66811 = VECTOR ( 'NONE', #48009, 1000.000000000000000 ) ;
#66812 = ORIENTED_EDGE ( 'NONE', *, *, #58771, .F. ) ;
#66813 = CARTESIAN_POINT ( 'NONE',  ( -2.499999999999996003, 12.50000000000000000, -0.06509327318403970719 ) ) ;
#66814 = ORIENTED_EDGE ( 'NONE', *, *, #123340, .F. ) ;
#66815 = CARTESIAN_POINT ( 'NONE',  ( 7.699999999999923794, 2.500000000000000000, -0.3464101615137783474 ) ) ;
#66816 = DIRECTION ( 'NONE',  ( 0.000000000000000000, 0.000000000000000000, 1.000000000000000000 ) ) ;
#66817 = ORIENTED_EDGE ( 'NONE', *, *, #45197, .T. ) ;
#66819 = ADVANCED_FACE ( 'NONE', ( #10643 ), #70245, .T. ) ;
#66818 = CARTESIAN_POINT ( 'NONE',  ( 108.0000000000000142, 9.000000000000001776, 0.000000000000000000 ) ) ;
#66821 = CARTESIAN_POINT ( 'NONE',  ( -8.950000000000011724, 2.500000000000000000, -6.048780366869521252 ) ) ;
#66820 = AXIS2_PLACEMENT_3D ( 'NONE', #51183, #20422, #91090 ) ;
#66822 = CARTESIAN_POINT ( 'NONE',  ( -10.84999999999999964, 2.500000000000000000, 7.188010851410848723 ) ) ;
#66823 = CARTESIAN_POINT ( 'NONE',  ( 11.89999999999990443, 2.500000000000000000, 0.3464101615137736845 ) ) ;
#66824 = ORIENTED_EDGE ( 'NONE', *, *, #66586, .F. ) ;
#66825 = CARTESIAN_POINT ( 'NONE',  ( -10.45000000000000107, 2.500000000000000000, 6.495190528383297135 ) ) ;
#66826 = FACE_OUTER_BOUND ( 'NONE', #13512, .T. ) ;
#66827 = EDGE_CURVE ( 'NONE', #127840, #81996, #61058, .T. ) ;
#66828 = EDGE_CURVE ( 'NONE', #128555, #26610, #96895, .T. ) ;
#66829 = CARTESIAN_POINT ( 'NONE',  ( 185.1510416670080872, 4.367472073101518859, -7.564683531249999149 ) ) ;
#66830 = CARTESIAN_POINT ( 'NONE',  ( -2.100000000000034284, 2.500000000000000000, -2.385244779468109755E-15 ) ) ;
#66831 = EDGE_CURVE ( 'NONE', #36298, #60265, #28391, .T. ) ;
#66832 = ADVANCED_FACE ( 'NONE', ( #60446 ), #121950, .T. ) ;
#66833 = DIRECTION ( 'NONE',  ( 0.000000000000000000, 0.000000000000000000, 1.000000000000000000 ) ) ;
#66834 = ORIENTED_EDGE ( 'NONE', *, *, #60199, .F. ) ;
#66835 = ORIENTED_EDGE ( 'NONE', *, *, #30980, .F. ) ;
#66836 = CARTESIAN_POINT ( 'NONE',  ( 179.5000000000000000, -0.6250000000000000000, 7.634788798650553154 ) ) ;
#66838 = EDGE_LOOP ( 'NONE', ( #42046, #82664 ) ) ;
#66837 = EDGE_CURVE ( 'NONE', #88967, #43024, #40497, .T. ) ;
#66839 = EDGE_CURVE ( 'NONE', #32739, #85461, #29043, .T. ) ;
#66840 = CARTESIAN_POINT ( 'NONE',  ( 7.299999999999926104, 12.50000000000000000, -0.4115034346978156399 ) ) ;
#66842 = ORIENTED_EDGE ( 'NONE', *, *, #129402, .T. ) ;
#66841 = ORIENTED_EDGE ( 'NONE', *, *, #27594, .T. ) ;
#66843 = ORIENTED_EDGE ( 'NONE', *, *, #76299, .T. ) ;
#66844 = EDGE_CURVE ( 'NONE', #16096, #121037, #36289, .T. ) ;
#66845 = FACE_OUTER_BOUND ( 'NONE', #26421, .T. ) ;
#66846 = ADVANCED_FACE ( 'NONE', ( #129194 ), #29672, .T. ) ;
#66847 = AXIS2_PLACEMENT_3D ( 'NONE', #31676, #59224, #31056 ) ;
#66848 = DIRECTION ( 'NONE',  ( 0.000000000000000000, 0.000000000000000000, 1.000000000000000000 ) ) ;
#66849 = EDGE_CURVE ( 'NONE', #34783, #42431, #119890, .T. ) ;
#66850 = CONICAL_SURFACE ( 'NONE', #127413, 0.1000000000000000472, 0.003490658503988666988 ) ;
#66851 = CARTESIAN_POINT ( 'NONE',  ( -11.64999999999999858, 12.50000000000000000, -5.802370205355746435 ) ) ;
#66852 =( NAMED_UNIT ( * ) PLANE_ANGLE_UNIT ( ) SI_UNIT ( $, .RADIAN. ) );
#66853 = CARTESIAN_POINT ( 'NONE',  ( -10.85000000000000142, 12.50000000000000000, -2.792790559304612508 ) ) ;
#66854 = LINE ( 'NONE', #55751, #16668 ) ;
#66855 = DIRECTION ( 'NONE',  ( 0.000000000000000000, 1.000000000000000000, 0.000000000000000000 ) ) ;
#66856 = ORIENTED_EDGE ( 'NONE', *, *, #53439, .F. ) ;
#66857 = EDGE_CURVE ( 'NONE', #111968, #74697, #86427, .T. ) ;
#66860 = AXIS2_PLACEMENT_3D ( 'NONE', #60298, #100200, #40658 ) ;
#66859 = CARTESIAN_POINT ( 'NONE',  ( 9.149999999999920419, 12.50000000000000000, 1.472243186433545459 ) ) ;
#66858 = AXIS2_PLACEMENT_3D ( 'NONE', #102468, #52719, #63189 ) ;
#66861 = ORIENTED_EDGE ( 'NONE', *, *, #127484, .F. ) ;
#66862 = EDGE_LOOP ( 'NONE', ( #125372, #114108, #39441, #119555 ) ) ;
#66863 = VERTEX_POINT ( 'NONE', #31612 ) ;
#66864 = ORIENTED_EDGE ( 'NONE', *, *, #81644, .F. ) ;
#66865 = CARTESIAN_POINT ( 'NONE',  ( -5.400000000000019895, 12.50000000000000000, 0.06509327318403515528 ) ) ;
#66866 = ORIENTED_EDGE ( 'NONE', *, *, #58369, .F. ) ;
#66867 = VERTEX_POINT ( 'NONE', #52534 ) ;
#66868 = AXIS2_PLACEMENT_3D ( 'NONE', #122841, #20777, #91442 ) ;
#66869 = AXIS2_PLACEMENT_3D ( 'NONE', #95743, #106207, #76100 ) ;
#66870 = DIRECTION ( 'NONE',  ( 0.000000000000000000, 1.000000000000000000, 0.000000000000000000 ) ) ;
#66871 = DIRECTION ( 'NONE',  ( -4.274815082592931898E-19, -0.9999939076577903929, -0.003490651415223739937 ) ) ;
#66872 = CONICAL_SURFACE ( 'NONE', #75282, 0.1000000000000000472, 0.003490658503988666988 ) ;
#66873 = DIRECTION ( 'NONE',  ( 0.000000000000000000, 0.000000000000000000, -1.000000000000000000 ) ) ;
#66874 = DIRECTION ( 'NONE',  ( 0.000000000000000000, 0.000000000000000000, 1.000000000000000000 ) ) ;
#66875 = LINE ( 'NONE', #117243, #30030 ) ;
#66876 = ORIENTED_EDGE ( 'NONE', *, *, #26082, .F. ) ;
#66877 = VECTOR ( 'NONE', #28213, 1000.000000000000000 ) ;
#66878 = FACE_OUTER_BOUND ( 'NONE', #119021, .T. ) ;
#66879 = AXIS2_PLACEMENT_3D ( 'NONE', #47150, #115879, #16993 ) ;
#66880 = ORIENTED_EDGE ( 'NONE', *, *, #14144, .T. ) ;
#66881 = LINE ( 'NONE', #17107, #4585 ) ;
#66882 = ORIENTED_EDGE ( 'NONE', *, *, #67449, .F. ) ;
#66883 = DIRECTION ( 'NONE',  ( 0.000000000000000000, -0.9999939076577903929, 0.003490651415223739937 ) ) ;
#66884 = CIRCLE ( 'NONE', #71096, 0.1000000000000000472 ) ;
#66885 = EDGE_LOOP ( 'NONE', ( #57842, #10949 ) ) ;
#66886 = VERTEX_POINT ( 'NONE', #71520 ) ;
#66887 = CARTESIAN_POINT ( 'NONE',  ( -8.150000000000009237, 12.50000000000000000, 6.776507416713035248 ) ) ;
#66888 = LINE ( 'NONE', #115996, #102816 ) ;
#66889 = ADVANCED_FACE ( 'NONE', ( #123833 ), #64281, .T. ) ;
#66890 = CARTESIAN_POINT ( 'NONE',  ( 186.2500000000000000, 9.429780353434619030E-16, -7.700000000000000178 ) ) ;
#66891 = CARTESIAN_POINT ( 'NONE',  ( -3.150000000000033218, 2.500000000000000000, -6.941600689897078347 ) ) ;
#66892 = EDGE_CURVE ( 'NONE', #33146, #92869, #23757, .T. ) ;
#66893 = DIRECTION ( 'NONE',  ( 0.000000000000000000, 1.000000000000000000, 0.000000000000000000 ) ) ;
#66894 = ORIENTED_EDGE ( 'NONE', *, *, #113188, .T. ) ;
#66895 = DIRECTION ( 'NONE',  ( 0.000000000000000000, 0.000000000000000000, 1.000000000000000000 ) ) ;
#66896 = CARTESIAN_POINT ( 'NONE',  ( 8.749999999999957367, 12.50000000000000000, 2.165063509461097713 ) ) ;
#66897 = FACE_OUTER_BOUND ( 'NONE', #80436, .T. ) ;
#66898 = FACE_OUTER_BOUND ( 'NONE', #624, .T. ) ;
#66899 = EDGE_CURVE ( 'NONE', #96815, #12366, #43380, .T. ) ;
#66900 = DIRECTION ( 'NONE',  ( -4.274815082592931898E-19, -0.9999939076577903929, -0.003490651415223739937 ) ) ;
#66901 = ORIENTED_EDGE ( 'NONE', *, *, #84425, .F. ) ;
#66902 = ORIENTED_EDGE ( 'NONE', *, *, #72394, .F. ) ;
#66903 = CARTESIAN_POINT ( 'NONE',  ( -8.950000000000004619, 2.500000000000000000, 6.048780366869521252 ) ) ;
#66904 = VECTOR ( 'NONE', #7118, 1000.000000000000000 ) ;
#66905 = VERTEX_POINT ( 'NONE', #42748 ) ;
#66906 = DIRECTION ( 'NONE',  ( -0.000000000000000000, -1.000000000000000000, -0.000000000000000000 ) ) ;
#66907 = CARTESIAN_POINT ( 'NONE',  ( -6.650000000000015454, 12.50000000000000000, 2.857883832488649301 ) ) ;
#66908 = ORIENTED_EDGE ( 'NONE', *, *, #82930, .F. ) ;
#66909 = CARTESIAN_POINT ( 'NONE',  ( 184.3750000000000000, 8.891194145520236347, 5.444286225454521982E-16 ) ) ;
#66910 = DIRECTION ( 'NONE',  ( -0.000000000000000000, -1.000000000000000000, -0.000000000000000000 ) ) ;
#66911 = CARTESIAN_POINT ( 'NONE',  ( 9.999999999999952038, 12.50000000000000000, -2.276824562219559311E-15 ) ) ;
#66912 =( NAMED_UNIT ( * ) SI_UNIT ( $, .STERADIAN. ) SOLID_ANGLE_UNIT ( ) );
#66913 = CARTESIAN_POINT ( 'NONE',  ( 4.149999999999941735, 12.50000000000000000, -1.537336459617587581 ) ) ;
#66914 = EDGE_LOOP ( 'NONE', ( #123965, #4924 ) ) ;
#66915 = AXIS2_PLACEMENT_3D ( 'NONE', #32965, #122616, #123883 ) ;
#66916 = FACE_OUTER_BOUND ( 'NONE', #32908, .T. ) ;
#66917 = DIRECTION ( 'NONE',  ( 0.000000000000000000, 1.000000000000000000, 0.000000000000000000 ) ) ;
#66918 = ORIENTED_EDGE ( 'NONE', *, *, #109262, .F. ) ;
#66919 = DIRECTION ( 'NONE',  ( 0.000000000000000000, 0.000000000000000000, 1.000000000000000000 ) ) ;
#66920 = DIRECTION ( 'NONE',  ( 0.000000000000000000, 0.000000000000000000, -1.000000000000000000 ) ) ;
#66921 = DIRECTION ( 'NONE',  ( -0.000000000000000000, -1.000000000000000000, -0.000000000000000000 ) ) ;
#66922 = EDGE_LOOP ( 'NONE', ( #98527, #90610 ) ) ;
#66923 = DIRECTION ( 'NONE',  ( -4.274815082592931898E-19, -0.9999939076577903929, -0.003490651415223739937 ) ) ;
#66924 = ORIENTED_EDGE ( 'NONE', *, *, #80025, .T. ) ;
#66925 = FACE_OUTER_BOUND ( 'NONE', #60025, .T. ) ;
#66926 = DIRECTION ( 'NONE',  ( 0.000000000000000000, -0.000000000000000000, 1.000000000000000000 ) ) ;
#66927 = DIRECTION ( 'NONE',  ( 0.000000000000000000, 0.000000000000000000, 1.000000000000000000 ) ) ;
#66928 = EDGE_LOOP ( 'NONE', ( #82242, #12385 ) ) ;
#66929 = AXIS2_PLACEMENT_3D ( 'NONE', #55602, #44488, #24855 ) ;
#66930 = DIRECTION ( 'NONE',  ( 0.000000000000000000, 0.000000000000000000, -1.000000000000000000 ) ) ;
#66931 = CONICAL_SURFACE ( 'NONE', #43975, 0.1000000000000000472, 0.003490658503988666988 ) ;
#66932 = DIRECTION ( 'NONE',  ( -0.000000000000000000, 1.000000000000000000, -0.000000000000000000 ) ) ;
#66933 = EDGE_CURVE ( 'NONE', #57940, #10654, #34231, .T. ) ;
#66934 = EDGE_LOOP ( 'NONE', ( #75163, #117277, #87163, #97980 ) ) ;
#66935 = DIRECTION ( 'NONE',  ( 0.000000000000000000, 0.000000000000000000, 1.000000000000000000 ) ) ;
#66936 = EDGE_CURVE ( 'NONE', #62733, #594, #34195, .T. ) ;
#66937 = ORIENTED_EDGE ( 'NONE', *, *, #116034, .T. ) ;
#66938 = DIRECTION ( 'NONE',  ( 0.000000000000000000, 1.000000000000000000, 0.000000000000000000 ) ) ;
#66939 = ORIENTED_EDGE ( 'NONE', *, *, #32448, .T. ) ;
#66940 = DIRECTION ( 'NONE',  ( 0.000000000000000000, 0.000000000000000000, 1.000000000000000000 ) ) ;
#66941 = CARTESIAN_POINT ( 'NONE',  ( 7.699999999999923794, 12.50000000000000000, 4.676537180435972552 ) ) ;
#66942 = ORIENTED_EDGE ( 'NONE', *, *, #17277, .T. ) ;
#66943 = EDGE_CURVE ( 'NONE', #80214, #96136, #124087, .T. ) ;
#66944 = VERTEX_POINT ( 'NONE', #53194 ) ;
#66945 = DIRECTION ( 'NONE',  ( -0.000000000000000000, 1.000000000000000000, -0.000000000000000000 ) ) ;
#66946 = CARTESIAN_POINT ( 'NONE',  ( 5.849999999999933920, 12.50000000000000000, 5.867463478539781896 ) ) ;
#66947 = EDGE_LOOP ( 'NONE', ( #72269, #107320 ) ) ;
#66949 = FACE_OUTER_BOUND ( 'NONE', #86391, .T. ) ;
#66948 = AXIS2_PLACEMENT_3D ( 'NONE', #32818, #21697, #83199 ) ;
#66950 = DIRECTION ( 'NONE',  ( 0.000000000000000000, 1.000000000000000000, 0.000000000000000000 ) ) ;
#66951 = AXIS2_PLACEMENT_3D ( 'NONE', #79045, #28653, #118948 ) ;
#66952 = FACE_OUTER_BOUND ( 'NONE', #114677, .T. ) ;
#66953 = CARTESIAN_POINT ( 'NONE',  ( -0.6500000000000389910, 2.500000000000000000, -1.818653347947326138 ) ) ;
#66954 = LINE ( 'NONE', #8674, #101697 ) ;
#66955 = FACE_OUTER_BOUND ( 'NONE', #39435, .T. ) ;
#66956 = AXIS2_PLACEMENT_3D ( 'NONE', #119743, #610, #77877 ) ;
#66957 = ORIENTED_EDGE ( 'NONE', *, *, #14699, .F. ) ;
#66959 = EDGE_LOOP ( 'NONE', ( #30903, #70646, #79611, #91739 ) ) ;
#66958 = ADVANCED_FACE ( 'NONE', ( #114037 ), #62369, .T. ) ;
#66960 = ORIENTED_EDGE ( 'NONE', *, *, #34003, .T. ) ;
#66961 = ORIENTED_EDGE ( 'NONE', *, *, #15098, .F. ) ;
#66962 = CIRCLE ( 'NONE', #115078, 8.699999999999999289 ) ;
#66963 = DIRECTION ( 'NONE',  ( 0.000000000000000000, 0.000000000000000000, 1.000000000000000000 ) ) ;
#66964 = DIRECTION ( 'NONE',  ( 0.000000000000000000, 1.000000000000000000, 0.000000000000000000 ) ) ;
#66965 = CARTESIAN_POINT ( 'NONE',  ( -11.64999999999999680, 12.50000000000000000, -2.165063509461097713 ) ) ;
#66966 = VERTEX_POINT ( 'NONE', #2138 ) ;
#66967 = FACE_BOUND ( 'NONE', #15282, .T. ) ;
#66968 = DIRECTION ( 'NONE',  ( 0.000000000000000000, 0.000000000000000000, 1.000000000000000000 ) ) ;
#66969 = CARTESIAN_POINT ( 'NONE',  ( 12.29999999999990656, 2.500000000000000000, 3.883716857408421319 ) ) ;
#66971 = ADVANCED_FACE ( 'NONE', ( #2785 ), #81985, .T. ) ;
#66970 = FACE_OUTER_BOUND ( 'NONE', #121430, .T. ) ;
#66972 = DIRECTION ( 'NONE',  ( 0.000000000000000000, 0.000000000000000000, 1.000000000000000000 ) ) ;
#66973 = DIRECTION ( 'NONE',  ( 0.000000000000000000, -0.000000000000000000, 1.000000000000000000 ) ) ;
#66974 = DIRECTION ( 'NONE',  ( 0.000000000000000000, 0.000000000000000000, -1.000000000000000000 ) ) ;
#66976 = DIRECTION ( 'NONE',  ( 0.000000000000000000, -0.000000000000000000, 1.000000000000000000 ) ) ;
#66975 =( BOUNDED_SURFACE ( )  B_SPLINE_SURFACE ( 3, 2, ( 
 ( #1086, #20735, #51495 ),
 ( #52134, #92043, #1722 ),
 ( #81579, #60672, #50208 ),
 ( #32512, #109091, #2349 ),
 ( #42313, #99301, #90095 ),
 ( #40388, #80308, #120227 ),
 ( #30574, #100568, #62603 ),
 ( #124728, #73059, #15401 ),
 ( #53426, #3666, #114261 ),
 ( #55349, #43611, #12815 ),
 ( #74341, #34436, #33766 ),
 ( #123434, #93341, #83530 ),
 ( #73685, #64512, #14744 ),
 ( #44226, #113624, #23958 ) ),
 .UNSPECIFIED., .F., .F., .F. ) 
 B_SPLINE_SURFACE_WITH_KNOTS ( ( 4, 2, 2, 2, 2, 2, 4 ),
 ( 3, 3 ),
 ( 0.000000000000000000, 0.001744612550434268029, 0.002616918825651402044, 0.003489225100868536059, 0.005233837651302804088, 0.006106143926519938536, 0.006978450201737072117 ),
 ( 0.000000000000000000, 1.000000000000000000 ),
 .UNSPECIFIED. ) 
 GEOMETRIC_REPRESENTATION_ITEM ( )  RATIONAL_B_SPLINE_SURFACE ( (
 ( 1.000000000000000000, 0.7318752858502209913, 1.000000000000000000),
 ( 1.000000000000000000, 0.7270130115579832575, 1.000000000000000000),
 ( 1.000000000000000000, 0.7223762446138062288, 1.000000000000000000),
 ( 1.000000000000000000, 0.7156127915551832031, 1.000000000000000000),
 ( 1.000000000000000000, 0.7133893117691495478, 1.000000000000000000),
 ( 1.000000000000000000, 0.7090389252574379464, 1.000000000000000000),
 ( 1.000000000000000000, 0.7069297463490226141, 1.000000000000000000),
 ( 1.000000000000000000, 0.7010696893203360869, 1.000000000000000000),
 ( 1.000000000000000000, 0.6977361265598307494, 1.000000000000000000),
 ( 1.000000000000000000, 0.6948030504688722520, 1.000000000000000000),
 ( 1.000000000000000000, 0.6942033558614880695, 1.000000000000000000),
 ( 1.000000000000000000, 0.6937817651809198294, 1.000000000000000000),
 ( 1.000000000000000000, 0.6939284133496614881, 1.000000000000000000),
 ( 1.000000000000000000, 0.6944177883068214374, 1.000000000000000000) ) ) 
 REPRESENTATION_ITEM ( '' )  SURFACE ( )  );
#66977 = CARTESIAN_POINT ( 'NONE',  ( -12.09999999999999432, 12.50000000000000000, 5.088040615133786027 ) ) ;
#66978 = EDGE_CURVE ( 'NONE', #91821, #83874, #61422, .T. ) ;
#66979 = EDGE_CURVE ( 'NONE', #61373, #114904, #23728, .T. ) ;
#66980 = CARTESIAN_POINT ( 'NONE',  ( 11.24999999999991118, 2.500000000000000000, 5.802370205355744659 ) ) ;
#66981 = EDGE_CURVE ( 'NONE', #113203, #47037, #76072, .T. ) ;
#66982 = ADVANCED_FACE ( 'NONE', ( #93750 ), #21801, .T. ) ;
#66983 = CARTESIAN_POINT ( 'NONE',  ( -11.84999999999999787, 2.500000000000000000, -1.818653347947321919 ) ) ;
#66984 = EDGE_LOOP ( 'NONE', ( #113723, #63179 ) ) ;
#66985 = ORIENTED_EDGE ( 'NONE', *, *, #5145, .F. ) ;
#66986 = ORIENTED_EDGE ( 'NONE', *, *, #40896, .F. ) ;
#66987 = VERTEX_POINT ( 'NONE', #72825 ) ;
#66988 = DIRECTION ( 'NONE',  ( 0.000000000000000000, 0.000000000000000000, 1.000000000000000000 ) ) ;
#66989 = ADVANCED_FACE ( 'NONE', ( #33554 ), #113378, .T. ) ;
#66990 = AXIS2_PLACEMENT_3D ( 'NONE', #37102, #126769, #68475 ) ;
#66991 = DIRECTION ( 'NONE',  ( 0.000000000000000000, 1.000000000000000000, 0.000000000000000000 ) ) ;
#66992 = CONICAL_SURFACE ( 'NONE', #102511, 0.1000000000000002554, 0.003490658503988666988 ) ;
#66995 = ORIENTED_EDGE ( 'NONE', *, *, #85769, .T. ) ;
#66994 = VERTEX_POINT ( 'NONE', #126440 ) ;
#66993 = EDGE_CURVE ( 'NONE', #89300, #101406, #83913, .T. ) ;
#66996 = VERTEX_POINT ( 'NONE', #125758 ) ;
#66997 = CARTESIAN_POINT ( 'NONE',  ( -0.8000000000000381251, 2.500000000000000000, 4.330127018922196314 ) ) ;
#66999 = ADVANCED_FACE ( 'NONE', ( #15816 ), #65570, .T. ) ;
#66998 = CIRCLE ( 'NONE', #92140, 0.1000000000000002554 ) ;
#67000 = CARTESIAN_POINT ( 'NONE',  ( 4.913542845205344456, -2.500000000001271871, 9.942462991357244206 ) ) ;
#67001 = CARTESIAN_POINT ( 'NONE',  ( 4.799999999999935874, 2.500000000000000000, 0.2464101615137735679 ) ) ;
#67002 = DIRECTION ( 'NONE',  ( -4.274815082592931898E-19, -0.9999939076577903929, -0.003490651415223739937 ) ) ;
#67003 = CARTESIAN_POINT ( 'NONE',  ( -14.54999999999998472, 12.50000000000000000, -2.165063509461099489 ) ) ;
#67004 = ADVANCED_FACE ( 'NONE', ( #55747 ), #51045, .T. ) ;
#67005 = ORIENTED_EDGE ( 'NONE', *, *, #52058, .T. ) ;
#67006 = ADVANCED_FACE ( 'NONE', ( #26305 ), #124189, .T. ) ;
#67007 = EDGE_LOOP ( 'NONE', ( #128271, #33477, #105875, #76683 ) ) ;
#67008 = EDGE_LOOP ( 'NONE', ( #119842, #57455 ) ) ;
#67009 = ORIENTED_EDGE ( 'NONE', *, *, #23377, .T. ) ;
#67010 = DIRECTION ( 'NONE',  ( 0.000000000000000000, 0.000000000000000000, 1.000000000000000000 ) ) ;
#67011 = ORIENTED_EDGE ( 'NONE', *, *, #49356, .F. ) ;
#67012 = ORIENTED_EDGE ( 'NONE', *, *, #86521, .F. ) ;
#67013 = CARTESIAN_POINT ( 'NONE',  ( -0.8000000000000376810, 2.500000000000000000, -4.330127018922201643 ) ) ;
#67014 = CARTESIAN_POINT ( 'NONE',  ( 11.84999999999990372, 2.500000000000000000, 1.818653347947321475 ) ) ;
#67015 = FACE_OUTER_BOUND ( 'NONE', #125658, .T. ) ;
#67016 = DIRECTION ( 'NONE',  ( 0.000000000000000000, 0.000000000000000000, 1.000000000000000000 ) ) ;
#67017 = DIRECTION ( 'NONE',  ( 0.000000000000000000, -0.000000000000000000, 1.000000000000000000 ) ) ;
#67018 = ORIENTED_EDGE ( 'NONE', *, *, #124330, .F. ) ;
#67019 = DIRECTION ( 'NONE',  ( 0.000000000000000000, -0.9999939076577903929, 0.003490651415223739937 ) ) ;
#67020 = CONICAL_SURFACE ( 'NONE', #81703, 0.1000000000000002554, 0.003490658503988666988 ) ;
#67021 = CIRCLE ( 'NONE', #10585, 0.06509327318403745899 ) ;
#67022 = VERTEX_POINT ( 'NONE', #95688 ) ;
#67023 = CARTESIAN_POINT ( 'NONE',  ( -4.200000000000025935, 12.50000000000000000, 4.330127018922196314 ) ) ;
#67024 = ORIENTED_EDGE ( 'NONE', *, *, #60364, .F. ) ;
#67025 = CARTESIAN_POINT ( 'NONE',  ( -6.850000000000017408, 2.500000000000000000, -6.248780366869526759 ) ) ;
#67026 = DIRECTION ( 'NONE',  ( -0.000000000000000000, -1.000000000000000000, -0.000000000000000000 ) ) ;
#67027 = ORIENTED_EDGE ( 'NONE', *, *, #41972, .F. ) ;
#67028 = CARTESIAN_POINT ( 'NONE',  ( -14.34999999999998543, 12.50000000000000000, 1.818653347947325472 ) ) ;
#67029 = DIRECTION ( 'NONE',  ( 0.000000000000000000, 0.000000000000000000, -1.000000000000000000 ) ) ;
#67030 = ORIENTED_EDGE ( 'NONE', *, *, #84737, .T. ) ;
#67031 = EDGE_CURVE ( 'NONE', #36337, #53182, #34849, .T. ) ;
#67032 = CARTESIAN_POINT ( 'NONE',  ( 14.99999999999992895, 12.50000000000000000, -0.06509327318403970719 ) ) ;
#67033 = EDGE_CURVE ( 'NONE', #106863, #55645, #36122, .T. ) ;
#67034 = ORIENTED_EDGE ( 'NONE', *, *, #66419, .T. ) ;
#67035 = VERTEX_POINT ( 'NONE', #117222 ) ;
#67036 = FACE_OUTER_BOUND ( 'NONE', #15303, .T. ) ;
#67037 = DIRECTION ( 'NONE',  ( -0.000000000000000000, 1.000000000000000000, -0.000000000000000000 ) ) ;
#67038 = CARTESIAN_POINT ( 'NONE',  ( 186.2135416670080872, 4.367472073101518859, -7.564683531249999149 ) ) ;
#67039 = DIRECTION ( 'NONE',  ( 0.000000000000000000, 0.000000000000000000, 1.000000000000000000 ) ) ;
#67040 = AXIS2_PLACEMENT_3D ( 'NONE', #83047, #92866, #43771 ) ;
#67041 = CONICAL_SURFACE ( 'NONE', #83787, 0.1000000000000000472, 0.003490658503988666988 ) ;
#67042 = DIRECTION ( 'NONE',  ( 0.000000000000000000, 0.000000000000000000, 1.000000000000000000 ) ) ;
#67043 = DIRECTION ( 'NONE',  ( 0.000000000000000000, 0.000000000000000000, -1.000000000000000000 ) ) ;
#67044 = CONICAL_SURFACE ( 'NONE', #110965, 0.1000000000000002554, 0.003490658503988666988 ) ;
#67045 = EDGE_LOOP ( 'NONE', ( #120999, #124649, #92860, #103220 ) ) ;
#67046 = DIRECTION ( 'NONE',  ( 0.000000000000000000, 1.000000000000000000, 0.000000000000000000 ) ) ;
#67047 = ORIENTED_EDGE ( 'NONE', *, *, #57367, .F. ) ;
#67048 = AXIS2_PLACEMENT_3D ( 'NONE', #114778, #64397, #6731 ) ;
#67049 = CARTESIAN_POINT ( 'NONE',  ( -14.34999999999998543, 12.50000000000000000, 1.818653347947325472 ) ) ;
#67050 = DIRECTION ( 'NONE',  ( 0.000000000000000000, 0.000000000000000000, 1.000000000000000000 ) ) ;
#67051 = DIRECTION ( 'NONE',  ( 0.000000000000000000, 1.000000000000000000, 0.000000000000000000 ) ) ;
#67052 = CARTESIAN_POINT ( 'NONE',  ( 5.199999999999933564, 2.500000000000000000, 3.983716857408420076 ) ) ;
#67053 = CARTESIAN_POINT ( 'NONE',  ( 3.149999999999946176, 12.50000000000000000, -2.511473670974877948 ) ) ;
#67054 = VERTEX_POINT ( 'NONE', #125143 ) ;
#67055 = DIRECTION ( 'NONE',  ( 0.000000000000000000, 0.000000000000000000, 1.000000000000000000 ) ) ;
#67056 =( NAMED_UNIT ( * ) PLANE_ANGLE_UNIT ( ) SI_UNIT ( $, .RADIAN. ) );
#67057 = ORIENTED_EDGE ( 'NONE', *, *, #94147, .T. ) ;
#67058 = FACE_OUTER_BOUND ( 'NONE', #92285, .T. ) ;
#67059 = ADVANCED_FACE ( 'NONE', ( #74757 ), #96308, .T. ) ;
#67060 = ORIENTED_EDGE ( 'NONE', *, *, #65354, .F. ) ;
#67061 = VERTEX_POINT ( 'NONE', #26941 ) ;
#67062 = DIRECTION ( 'NONE',  ( -0.000000000000000000, -1.000000000000000000, -0.000000000000000000 ) ) ;
#67063 = CIRCLE ( 'NONE', #27364, 0.06509327318403745899 ) ;
#67064 = CIRCLE ( 'NONE', #69145, 0.06509327318403745899 ) ;
#67065 = VERTEX_POINT ( 'NONE', #44653 ) ;
#67066 = DIRECTION ( 'NONE',  ( 0.000000000000000000, 0.000000000000000000, -1.000000000000000000 ) ) ;
#67067 = DIRECTION ( 'NONE',  ( 0.000000000000000000, 0.000000000000000000, -1.000000000000000000 ) ) ;
#67068 = CARTESIAN_POINT ( 'NONE',  ( 1.449999999999950440, 12.50000000000000000, 6.148780366869520009 ) ) ;
#67069 = ORIENTED_EDGE ( 'NONE', *, *, #64341, .T. ) ;
#67070 = FACE_BOUND ( 'NONE', #76839, .T. ) ;
#67072 = ORIENTED_EDGE ( 'NONE', *, *, #109184, .T. ) ;
#67071 = CARTESIAN_POINT ( 'NONE',  ( -12.04999999999999538, 2.500000000000000000, 6.595190528383296780 ) ) ;
#67074 = ADVANCED_FACE ( 'NONE', ( #17078 ), #57027, .T. ) ;
#67073 = CIRCLE ( 'NONE', #113075, 0.1000000000000002554 ) ;
#67075 = FACE_OUTER_BOUND ( 'NONE', #93232, .T. ) ;
#67076 = DIRECTION ( 'NONE',  ( 0.000000000000000000, 1.000000000000000000, 0.000000000000000000 ) ) ;
#67077 = EDGE_CURVE ( 'NONE', #76508, #112624, #74014, .T. ) ;
#67078 = ORIENTED_EDGE ( 'NONE', *, *, #116669, .T. ) ;
#67079 = ORIENTED_EDGE ( 'NONE', *, *, #118962, .F. ) ;
#67080 = EDGE_LOOP ( 'NONE', ( #5161, #21669 ) ) ;
#67081 = DIRECTION ( 'NONE',  ( 0.000000000000000000, 0.000000000000000000, 1.000000000000000000 ) ) ;
#67082 = DIRECTION ( 'NONE',  ( -0.000000000000000000, 1.000000000000000000, -0.000000000000000000 ) ) ;
#67083 = CARTESIAN_POINT ( 'NONE',  ( 3.349999999999945466, 2.500000000000000000, -2.857883832488653741 ) ) ;
#67084 = EDGE_CURVE ( 'NONE', #90336, #55993, #17557, .T. ) ;
#67085 = FACE_BOUND ( 'NONE', #107049, .T. ) ;
#67086 = EDGE_LOOP ( 'NONE', ( #120876, #16349 ) ) ;
#67087 = CARTESIAN_POINT ( 'NONE',  ( 4.399999999999940847, 2.500000000000000000, -4.083716857408426826 ) ) ;
#67088 = DIRECTION ( 'NONE',  ( 0.000000000000000000, 1.000000000000000000, 0.000000000000000000 ) ) ;
#67089 = EDGE_LOOP ( 'NONE', ( #68974, #64991, #13936, #42912 ) ) ;
#67090 = CONICAL_SURFACE ( 'NONE', #33683, 0.1000000000000000472, 0.003490658503988666988 ) ;
#67091 = CARTESIAN_POINT ( 'NONE',  ( -8.350000000000013856, 2.500000000000000000, -2.265063509461101798 ) ) ;
#67092 = DIRECTION ( 'NONE',  ( -0.000000000000000000, 1.000000000000000000, -0.000000000000000000 ) ) ;
#67093 = DIRECTION ( 'NONE',  ( 0.000000000000000000, 1.000000000000000000, 0.000000000000000000 ) ) ;
#67094 = DIRECTION ( 'NONE',  ( 0.000000000000000000, 1.000000000000000000, 0.000000000000000000 ) ) ;
#67095 = FACE_OUTER_BOUND ( 'NONE', #90245, .T. ) ;
#67096 = CIRCLE ( 'NONE', #100571, 0.06509327318403745899 ) ;
#67097 = CIRCLE ( 'NONE', #96362, 0.06509327318403745899 ) ;
#67098 = ORIENTED_EDGE ( 'NONE', *, *, #112359, .F. ) ;
#67099 = EDGE_LOOP ( 'NONE', ( #18066, #55102, #80325, #125689 ) ) ;
#67100 = ORIENTED_EDGE ( 'NONE', *, *, #38919, .F. ) ;
#67101 = ORIENTED_EDGE ( 'NONE', *, *, #21276, .T. ) ;
#67102 = ORIENTED_EDGE ( 'NONE', *, *, #52052, .F. ) ;
#67103 = DIRECTION ( 'NONE',  ( 0.000000000000000000, -0.000000000000000000, 1.000000000000000000 ) ) ;
#67104 = DIRECTION ( 'NONE',  ( -0.000000000000000000, 1.000000000000000000, -0.000000000000000000 ) ) ;
#67105 = ORIENTED_EDGE ( 'NONE', *, *, #26222, .F. ) ;
#67106 = FACE_BOUND ( 'NONE', #64201, .T. ) ;
#67107 = CARTESIAN_POINT ( 'NONE',  ( 13.09999999999990195, 2.500000000000000000, -4.676537180435978769 ) ) ;
#67108 = AXIS2_PLACEMENT_3D ( 'NONE', #28250, #19726, #30202 ) ;
#67109 = EDGE_CURVE ( 'NONE', #36921, #103404, #111570, .T. ) ;
#67110 = DIRECTION ( 'NONE',  ( 0.000000000000000000, -0.9999939076577903929, 0.003490651415223739937 ) ) ;
#67111 = PLANE ( 'NONE',  #64123 ) ;
#67112 = DIRECTION ( 'NONE',  ( 0.000000000000000000, -0.000000000000000000, 1.000000000000000000 ) ) ;
#67113 = EDGE_CURVE ( 'NONE', #90160, #63978, #38436, .T. ) ;
#67114 = LINE ( 'NONE', #46878, #22482 ) ;
#67115 = ORIENTED_EDGE ( 'NONE', *, *, #53674, .F. ) ;
#67116 = CARTESIAN_POINT ( 'NONE',  ( 9.999999999999911182, 12.50000000000000000, -3.637306695894650055 ) ) ;
#67117 = EDGE_CURVE ( 'NONE', #53996, #43807, #109525, .T. ) ;
#67118 = AXIS2_PLACEMENT_3D ( 'NONE', #27974, #40389, #77703 ) ;
#67119 = VERTEX_POINT ( 'NONE', #77325 ) ;
#67120 = AXIS2_PLACEMENT_3D ( 'NONE', #110893, #2223, #40237 ) ;
#67121 = ORIENTED_EDGE ( 'NONE', *, *, #107948, .T. ) ;
#67122 = ORIENTED_EDGE ( 'NONE', *, *, #33726, .F. ) ;
#67123 = EDGE_CURVE ( 'NONE', #102800, #60587, #71879, .T. ) ;
#67124 = CARTESIAN_POINT ( 'NONE',  ( 5.849999999999935696, 12.50000000000000000, -7.188010851410854052 ) ) ;
#67126 = EDGE_CURVE ( 'NONE', #48660, #98142, #119989, .T. ) ;
#67125 = DIRECTION ( 'NONE',  ( -0.000000000000000000, -1.000000000000000000, -0.000000000000000000 ) ) ;
#67127 = DIRECTION ( 'NONE',  ( 0.000000000000000000, 0.000000000000000000, 1.000000000000000000 ) ) ;
#67129 = EDGE_LOOP ( 'NONE', ( #38258, #104743 ) ) ;
#67128 = EDGE_CURVE ( 'NONE', #120619, #79607, #2915, .T. ) ;
#67130 = CARTESIAN_POINT ( 'NONE',  ( 11.24999999999994316, 2.500000000000000000, -6.595190528383302109 ) ) ;
#67132 = EDGE_CURVE ( 'NONE', #57691, #73360, #44776, .T. ) ;
#67131 = CIRCLE ( 'NONE', #60901, 0.09999999999999982514 ) ;
#67133 = DIRECTION ( 'NONE',  ( -0.000000000000000000, 1.000000000000000000, -0.000000000000000000 ) ) ;
#67135 = EDGE_CURVE ( 'NONE', #80417, #34203, #117914, .T. ) ;
#67134 = DIRECTION ( 'NONE',  ( -0.000000000000000000, -1.000000000000000000, -0.000000000000000000 ) ) ;
#67136 = AXIS2_PLACEMENT_3D ( 'NONE', #118003, #127828, #57809 ) ;
#67137 = AXIS2_PLACEMENT_3D ( 'NONE', #122912, #5689, #45644 ) ;
#67138 = CARTESIAN_POINT ( 'NONE',  ( 183.8229166673494888, -4.445597072760122614, 7.699999999999998401 ) ) ;
#67139 = DIRECTION ( 'NONE',  ( 0.000000000000000000, 0.000000000000000000, 1.000000000000000000 ) ) ;
#67140 = PLANE ( 'NONE',  #86378 ) ;
#67141 = CARTESIAN_POINT ( 'NONE',  ( -6.900000000000019007, 12.50000000000000000, -4.048810130592463530 ) ) ;
#67142 = ORIENTED_EDGE ( 'NONE', *, *, #121284, .F. ) ;
#67143 = CARTESIAN_POINT ( 'NONE',  ( 1.249999999999952038, 2.500000000000000000, -1.572243186433550211 ) ) ;
#67144 = ADVANCED_FACE ( 'NONE', ( #115821 ), #34320, .T. ) ;
#67145 = EDGE_LOOP ( 'NONE', ( #95365, #46333 ) ) ;
#67146 = ORIENTED_EDGE ( 'NONE', *, *, #33067, .F. ) ;
#67147 = CARTESIAN_POINT ( 'NONE',  ( -6.700000000000016165, 2.500000000000000000, 4.330127018922196314 ) ) ;
#67148 = CARTESIAN_POINT ( 'NONE',  ( -2.050000000000032685, 2.500000000000000000, -6.495190528383302464 ) ) ;
#67149 = CARTESIAN_POINT ( 'NONE',  ( 10.39999999999991154, 2.500000000000000000, -5.022947341949754119 ) ) ;
#67150 = VERTEX_POINT ( 'NONE', #75254 ) ;
#67151 = ORIENTED_EDGE ( 'NONE', *, *, #124899, .T. ) ;
#67152 = CARTESIAN_POINT ( 'NONE',  ( 11.24999999999994316, 12.50000000000000000, 2.230156782645134950 ) ) ;
#67153 = DIRECTION ( 'NONE',  ( -0.000000000000000000, 1.000000000000000000, -0.000000000000000000 ) ) ;
#67154 = CARTESIAN_POINT ( 'NONE',  ( 16.56576425165007649, -1.499999999999997113, -6.084390597445789695 ) ) ;
#67155 = ORIENTED_EDGE ( 'NONE', *, *, #15919, .T. ) ;
#67156 = ORIENTED_EDGE ( 'NONE', *, *, #47704, .F. ) ;
#67157 = VECTOR ( 'NONE', #38082, 1000.000000000000000 ) ;
#67158 = CIRCLE ( 'NONE', #12794, 0.06509327318403745899 ) ;
#67159 = CARTESIAN_POINT ( 'NONE',  ( -14.34999999999998543, 2.500000000000000000, 1.818653347947325472 ) ) ;
#67160 = ORIENTED_EDGE ( 'NONE', *, *, #94771, .F. ) ;
#67161 = CARTESIAN_POINT ( 'NONE',  ( 0.8499999999999553468, 2.500000000000000000, -2.265063509461101798 ) ) ;
#67162 = CIRCLE ( 'NONE', #8591, 0.1000000000000002554 ) ;
#67163 = FACE_OUTER_BOUND ( 'NONE', #27087, .T. ) ;
#67164 = ORIENTED_EDGE ( 'NONE', *, *, #121380, .T. ) ;
#67165 = CARTESIAN_POINT ( 'NONE',  ( -0.6500000000000389910, 2.500000000000000000, -1.918653347947326004 ) ) ;
#67166 = AXIS2_PLACEMENT_3D ( 'NONE', #126750, #77626, #97918 ) ;
#67167 = PLANE ( 'NONE',  #58856 ) ;
#67168 = DIRECTION ( 'NONE',  ( 0.000000000000000000, 0.000000000000000000, 1.000000000000000000 ) ) ;
#67169 = CIRCLE ( 'NONE', #92230, 0.09999999999999982514 ) ;
#67170 = DIRECTION ( 'NONE',  ( -0.000000000000000000, -1.000000000000000000, -0.000000000000000000 ) ) ;
#67171 = ORIENTED_EDGE ( 'NONE', *, *, #119965, .T. ) ;
#67172 = DIRECTION ( 'NONE',  ( -0.000000000000000000, 1.000000000000000000, -0.000000000000000000 ) ) ;
#67173 = ADVANCED_FACE ( 'NONE', ( #83782 ), #32179, .T. ) ;
#67174 = DIRECTION ( 'NONE',  ( 0.000000000000000000, 0.000000000000000000, 1.000000000000000000 ) ) ;
#67175 = VERTEX_POINT ( 'NONE', #105363 ) ;
#67176 = EDGE_LOOP ( 'NONE', ( #63287, #8431 ) ) ;
#67177 = CARTESIAN_POINT ( 'NONE',  ( 185.4218750003414016, 0.000000000000000000, 7.564683531250000925 ) ) ;
#67178 = DIRECTION ( 'NONE',  ( 0.000000000000000000, 0.000000000000000000, -1.000000000000000000 ) ) ;
#67179 = DIRECTION ( 'NONE',  ( 0.000000000000000000, 0.000000000000000000, 1.000000000000000000 ) ) ;
#67180 = FACE_OUTER_BOUND ( 'NONE', #38198, .T. ) ;
#67181 = DIRECTION ( 'NONE',  ( -0.000000000000000000, 1.000000000000000000, -0.000000000000000000 ) ) ;
#67182 = DIRECTION ( 'NONE',  ( 0.000000000000000000, 1.000000000000000000, 0.000000000000000000 ) ) ;
#67183 = EDGE_CURVE ( 'NONE', #5504, #106259, #65599, .T. ) ;
#67184 = CARTESIAN_POINT ( 'NONE',  ( 16.98389417446983884, 2.499999999999060751, -5.627887362476348798 ) ) ;
#67185 = CARTESIAN_POINT ( 'NONE',  ( 11.04999999999990834, 12.50000000000000000, 1.883746621131358934 ) ) ;
#67186 = DIRECTION ( 'NONE',  ( 0.000000000000000000, 0.000000000000000000, 1.000000000000000000 ) ) ;
#67187 = DIRECTION ( 'NONE',  ( 0.000000000000000000, -0.9999939076577903929, 0.003490651415223739937 ) ) ;
#67188 = AXIS2_PLACEMENT_3D ( 'NONE', #64016, #33911, #64655 ) ;
#67189 = AXIS2_PLACEMENT_3D ( 'NONE', #99096, #38245, #118722 ) ;
#67190 = ORIENTED_EDGE ( 'NONE', *, *, #29692, .T. ) ;
#67191 = DIRECTION ( 'NONE',  ( 0.000000000000000000, 0.000000000000000000, 1.000000000000000000 ) ) ;
#67192 = CARTESIAN_POINT ( 'NONE',  ( 4.149999999999939959, 12.50000000000000000, 2.922977105672686982 ) ) ;
#67193 = DIRECTION ( 'NONE',  ( 0.000000000000000000, 0.000000000000000000, 1.000000000000000000 ) ) ;
#67194 = CARTESIAN_POINT ( 'NONE',  ( 4.349999999999940137, 12.50000000000000000, -6.906693963081115939 ) ) ;
#67195 = AXIS2_PLACEMENT_3D ( 'NONE', #60198, #18944, #20899 ) ;
#67196 = CIRCLE ( 'NONE', #71332, 0.1000000000000002554 ) ;
#67197 = ORIENTED_EDGE ( 'NONE', *, *, #75599, .T. ) ;
#67198 = DIRECTION ( 'NONE',  ( 0.000000000000000000, 0.000000000000000000, 1.000000000000000000 ) ) ;
#67199 = CONICAL_SURFACE ( 'NONE', #63040, 0.1000000000000002554, 0.003490658503988666988 ) ;
#67200 = DIRECTION ( 'NONE',  ( 0.000000000000000000, 0.000000000000000000, 1.000000000000000000 ) ) ;
#67202 = ORIENTED_EDGE ( 'NONE', *, *, #24597, .T. ) ;
#67201 = CARTESIAN_POINT ( 'NONE',  ( -0.8000000000000376810, 12.50000000000000000, -4.330127018922201643 ) ) ;
#67203 = CIRCLE ( 'NONE', #27514, 0.06509327318403745899 ) ;
#67204 = ORIENTED_EDGE ( 'NONE', *, *, #88134, .T. ) ;
#67205 = CONICAL_SURFACE ( 'NONE', #14984, 0.1000000000000002554, 0.003490658503988666988 ) ;
#67206 = EDGE_CURVE ( 'NONE', #126098, #78919, #113904, .T. ) ;
#67207 = ORIENTED_EDGE ( 'NONE', *, *, #40464, .T. ) ;
#67208 = ORIENTED_EDGE ( 'NONE', *, *, #84766, .F. ) ;
#67210 = EDGE_LOOP ( 'NONE', ( #54389, #64754 ) ) ;
#67209 = AXIS2_PLACEMENT_3D ( 'NONE', #107812, #108446, #79636 ) ;
#67211 = CARTESIAN_POINT ( 'NONE',  ( 9.999999999999912959, 2.500000000000000000, -5.022947341949754119 ) ) ;
#67212 = VECTOR ( 'NONE', #42848, 1000.000000000000000 ) ;
#67213 = DIRECTION ( 'NONE',  ( 0.000000000000000000, -0.000000000000000000, 1.000000000000000000 ) ) ;
#67214 = CARTESIAN_POINT ( 'NONE',  ( 6.849999999999929479, 2.500000000000000000, -1.718653347947326049 ) ) ;
#67215 = CARTESIAN_POINT ( 'NONE',  ( 8.349999999999923261, 12.50000000000000000, 2.857883832488649301 ) ) ;
#67216 = EDGE_CURVE ( 'NONE', #127598, #119087, #7087, .T. ) ;
#67217 = ORIENTED_EDGE ( 'NONE', *, *, #104684, .T. ) ;
#67218 = CIRCLE ( 'NONE', #40078, 0.09999999999999982514 ) ;
#67219 = CARTESIAN_POINT ( 'NONE',  ( -2.500000000000030642, 2.500000000000000000, -5.122947341949753763 ) ) ;
#67220 = EDGE_LOOP ( 'NONE', ( #49643, #119271 ) ) ;
#67221 = CARTESIAN_POINT ( 'NONE',  ( 48.67919755221870304, -3.179368040587171151, -5.083101271994035386 ) ) ;
#67222 = CARTESIAN_POINT ( 'NONE',  ( 16.56576425165006228, -1.499999999999999778, -6.084390597445814564 ) ) ;
#67223 = EDGE_CURVE ( 'NONE', #59349, #23039, #115767, .T. ) ;
#67224 = CARTESIAN_POINT ( 'NONE',  ( 5.649999999999934630, 12.50000000000000000, 6.148780366869520897 ) ) ;
#67225 = DIRECTION ( 'NONE',  ( 0.000000000000000000, 1.000000000000000000, 0.000000000000000000 ) ) ;
#67226 = EDGE_CURVE ( 'NONE', #55758, #79598, #123687, .T. ) ;
#67227 = EDGE_LOOP ( 'NONE', ( #3908, #102355, #129371, #96674 ) ) ;
#67228 = ORIENTED_EDGE ( 'NONE', *, *, #60524, .T. ) ;
#67230 = ORIENTED_EDGE ( 'NONE', *, *, #51387, .T. ) ;
#67229 = EDGE_CURVE ( 'NONE', #30373, #62733, #59370, .T. ) ;
#67231 = ORIENTED_EDGE ( 'NONE', *, *, #45501, .T. ) ;
#67232 = LINE ( 'NONE', #58748, #98443 ) ;
#67233 = DIRECTION ( 'NONE',  ( -0.000000000000000000, 1.000000000000000000, -0.000000000000000000 ) ) ;
#67234 = DIRECTION ( 'NONE',  ( 0.000000000000000000, 0.000000000000000000, -1.000000000000000000 ) ) ;
#67235 = EDGE_CURVE ( 'NONE', #117751, #102540, #126296, .T. ) ;
#67236 = FACE_BOUND ( 'NONE', #31764, .T. ) ;
#67237 = DIRECTION ( 'NONE',  ( 0.000000000000000000, -0.9999939076577903929, 0.003490651415223739937 ) ) ;
#67238 = CARTESIAN_POINT ( 'NONE',  ( 10.19999999999991402, 12.50000000000000000, 0.3464101615137735735 ) ) ;
#67239 = CARTESIAN_POINT ( 'NONE',  ( 3.149999999999946176, 12.50000000000000000, -6.841600689897077814 ) ) ;
#67240 = PLANE ( 'NONE',  #20771 ) ;
#67241 = AXIS2_PLACEMENT_3D ( 'NONE', #51678, #102060, #71292 ) ;
#67242 = AXIS2_PLACEMENT_3D ( 'NONE', #5710, #126797, #115016 ) ;
#67244 = AXIS2_PLACEMENT_3D ( 'NONE', #15180, #123857, #35506 ) ;
#67243 = CARTESIAN_POINT ( 'NONE',  ( 184.6302083336747444, -4.367472073101514418, -7.564683531250002702 ) ) ;
#67245 = DIRECTION ( 'NONE',  ( 0.000000000000000000, 0.000000000000000000, -1.000000000000000000 ) ) ;
#67246 = CARTESIAN_POINT ( 'NONE',  ( 87.50000000000001421, 0.000000000000000000, 0.000000000000000000 ) ) ;
#67247 = DIRECTION ( 'NONE',  ( 0.000000000000000000, 0.000000000000000000, 1.000000000000000000 ) ) ;
#67248 = ORIENTED_EDGE ( 'NONE', *, *, #80343, .F. ) ;
#67249 = VERTEX_POINT ( 'NONE', #24870 ) ;
#67250 = VERTEX_POINT ( 'NONE', #115146 ) ;
#67251 = EDGE_LOOP ( 'NONE', ( #39700, #29215 ) ) ;
#67252 = AXIS2_PLACEMENT_3D ( 'NONE', #126069, #36435, #76345 ) ;
#67253 = VECTOR ( 'NONE', #13957, 1000.000000000000000 ) ;
#67254 = DIRECTION ( 'NONE',  ( 0.000000000000000000, 0.000000000000000000, 1.000000000000000000 ) ) ;
#67255 = FACE_BOUND ( 'NONE', #17605, .T. ) ;
#67256 = LINE ( 'NONE', #97398, #89172 ) ;
#67257 = DIRECTION ( 'NONE',  ( 0.000000000000000000, 1.846105847067148022E-16, -1.000000000000000000 ) ) ;
#67258 = ORIENTED_EDGE ( 'NONE', *, *, #113394, .T. ) ;
#67259 = DIRECTION ( 'NONE',  ( -4.274815082592931898E-19, -0.9999939076577903929, -0.003490651415223739937 ) ) ;
#67260 = FACE_OUTER_BOUND ( 'NONE', #60688, .T. ) ;
#67261 = DIRECTION ( 'NONE',  ( -0.000000000000000000, -1.000000000000000000, -0.000000000000000000 ) ) ;
#67262 = VERTEX_POINT ( 'NONE', #34714 ) ;
#67263 = CARTESIAN_POINT ( 'NONE',  ( 3.949999999999939782, 2.500000000000000000, 2.411473670974873862 ) ) ;
#67264 = CARTESIAN_POINT ( 'NONE',  ( -9.150000000000009237, 12.50000000000000000, -6.495190528383297135 ) ) ;
#67265 = EDGE_CURVE ( 'NONE', #49835, #76293, #106011, .T. ) ;
#67266 = ADVANCED_FACE ( 'NONE', ( #5852 ), #86525, .T. ) ;
#67267 = ORIENTED_EDGE ( 'NONE', *, *, #34854, .F. ) ;
#67268 = EDGE_CURVE ( 'NONE', #2954, #34969, #13360, .T. ) ;
#67269 = DIRECTION ( 'NONE',  ( 0.000000000000000000, 0.000000000000000000, 1.000000000000000000 ) ) ;
#67270 = LINE ( 'NONE', #39173, #112477 ) ;
#67271 = EDGE_CURVE ( 'NONE', #97516, #98415, #43884, .T. ) ;
#67272 = ADVANCED_FACE ( 'NONE', ( #45165 ), #104076, .T. ) ;
#67273 = VECTOR ( 'NONE', #83514, 1000.000000000000000 ) ;
#67274 = AXIS2_PLACEMENT_3D ( 'NONE', #71552, #111476, #21832 ) ;
#67275 = ORIENTED_EDGE ( 'NONE', *, *, #110626, .T. ) ;
#67276 = CARTESIAN_POINT ( 'NONE',  ( 0.5999999999999551248, 12.50000000000000000, -4.676537180435978769 ) ) ;
#67277 = DIRECTION ( 'NONE',  ( 0.000000000000000000, 1.000000000000000000, 0.000000000000000000 ) ) ;
#67278 = VERTEX_POINT ( 'NONE', #54329 ) ;
#67280 = EDGE_CURVE ( 'NONE', #113021, #127796, #74114, .T. ) ;
#67279 = DIRECTION ( 'NONE',  ( 0.000000000000000000, 0.000000000000000000, 1.000000000000000000 ) ) ;
#67281 = ORIENTED_EDGE ( 'NONE', *, *, #19568, .F. ) ;
#67282 = VERTEX_POINT ( 'NONE', #4544 ) ;
#67283 = CARTESIAN_POINT ( 'NONE',  ( -8.300000000000009592, 12.50000000000000000, 4.265033745738159077 ) ) ;
#67284 = CIRCLE ( 'NONE', #107013, 0.06509327318403745899 ) ;
#67285 = ORIENTED_EDGE ( 'NONE', *, *, #26923, .F. ) ;
#67286 = DIRECTION ( 'NONE',  ( 0.000000000000000000, 0.000000000000000000, 1.000000000000000000 ) ) ;
#67287 = AXIS2_PLACEMENT_3D ( 'NONE', #3604, #86003, #4229 ) ;
#67288 = FACE_BOUND ( 'NONE', #20400, .T. ) ;
#67289 = ADVANCED_FACE ( 'NONE', ( #125630 ), #75895, .T. ) ;
#67290 = CIRCLE ( 'NONE', #98704, 0.1000000000000002554 ) ;
#67291 = EDGE_CURVE ( 'NONE', #68087, #120638, #71972, .T. ) ;
#67292 = ORIENTED_EDGE ( 'NONE', *, *, #89902, .F. ) ;
#67293 = AXIS2_PLACEMENT_3D ( 'NONE', #43592, #83511, #123410 ) ;
#67294 = CARTESIAN_POINT ( 'NONE',  ( 8.749999999999918288, 2.500000000000000000, -1.372243186433550033 ) ) ;
#67295 = EDGE_LOOP ( 'NONE', ( #11997, #18625 ) ) ;
#67296 = CARTESIAN_POINT ( 'NONE',  ( 2.099999999999950351, 12.50000000000000000, -5.022947341949754119 ) ) ;
#67297 = DIRECTION ( 'NONE',  ( -1.000000000000000000, 0.000000000000000000, 0.000000000000000000 ) ) ;
#67298 = LINE ( 'NONE', #107256, #44543 ) ;
#67299 = DIRECTION ( 'NONE',  ( -0.000000000000000000, -1.000000000000000000, -0.000000000000000000 ) ) ;
#67300 = DIRECTION ( 'NONE',  ( -0.000000000000000000, -1.000000000000000000, -0.000000000000000000 ) ) ;
#67301 = CIRCLE ( 'NONE', #100766, 0.09999999999999982514 ) ;
#67302 = VERTEX_POINT ( 'NONE', #58216 ) ;
#67303 = ORIENTED_EDGE ( 'NONE', *, *, #18080, .T. ) ;
#67304 = PLANE ( 'NONE',  #55906 ) ;
#67306 = CIRCLE ( 'NONE', #125818, 0.06509327318403745899 ) ;
#67305 = DIRECTION ( 'NONE',  ( -0.000000000000000000, 1.000000000000000000, -0.000000000000000000 ) ) ;
#67307 = AXIS2_PLACEMENT_3D ( 'NONE', #4081, #73463, #104222 ) ;
#67308 = AXIS2_PLACEMENT_3D ( 'NONE', #38030, #10491, #127696 ) ;
#67309 = DIRECTION ( 'NONE',  ( -0.000000000000000000, 1.000000000000000000, -0.000000000000000000 ) ) ;
#67311 = ORIENTED_EDGE ( 'NONE', *, *, #30723, .T. ) ;
#67310 = ORIENTED_EDGE ( 'NONE', *, *, #116811, .F. ) ;
#67312 = ORIENTED_EDGE ( 'NONE', *, *, #59381, .T. ) ;
#67313 = DIRECTION ( 'NONE',  ( 0.000000000000000000, 0.000000000000000000, 1.000000000000000000 ) ) ;
#67314 = CIRCLE ( 'NONE', #61093, 0.06509327318403745899 ) ;
#67315 = FACE_OUTER_BOUND ( 'NONE', #25546, .T. ) ;
#67316 = PLANE ( 'NONE',  #95887 ) ;
#67317 = SHAPE_DEFINITION_REPRESENTATION ( #75466, #107120 ) ;
#67318 = CARTESIAN_POINT ( 'NONE',  ( -4.550000000000022915, 2.500000000000000000, -2.065063509461102065 ) ) ;
#67319 = AXIS2_PLACEMENT_3D ( 'NONE', #121230, #2086, #42033 ) ;
#67320 = CARTESIAN_POINT ( 'NONE',  ( 13.14999999999989733, 12.50000000000000000, -2.576566944158915184 ) ) ;
#67321 = CARTESIAN_POINT ( 'NONE',  ( 5.599999999999934808, 2.500000000000000000, -4.083716857408426826 ) ) ;
#67322 = FACE_OUTER_BOUND ( 'NONE', #125642, .T. ) ;
#67323 = CARTESIAN_POINT ( 'NONE',  ( -4.550000000000022915, 2.500000000000000000, 6.595190528383296780 ) ) ;
#67324 = CARTESIAN_POINT ( 'NONE',  ( 0.3999999999999563904, 12.50000000000000000, 3.637306695894644726 ) ) ;
#67325 = VERTEX_POINT ( 'NONE', #129544 ) ;
#67326 = ORIENTED_EDGE ( 'NONE', *, *, #59904, .T. ) ;
#67327 = FACE_OUTER_BOUND ( 'NONE', #41276, .T. ) ;
#67328 = VERTEX_POINT ( 'NONE', #98750 ) ;
#67329 = EDGE_LOOP ( 'NONE', ( #23946, #121878, #54788, #117911 ) ) ;
#67330 = DIRECTION ( 'NONE',  ( -0.000000000000000000, 1.000000000000000000, -0.000000000000000000 ) ) ;
#67331 = CARTESIAN_POINT ( 'NONE',  ( -11.25000000000000178, 12.50000000000000000, -5.867463478539783672 ) ) ;
#67332 = CARTESIAN_POINT ( 'NONE',  ( 11.84999999999990727, 12.50000000000000000, -1.818653347947326138 ) ) ;
#67333 = PLANE ( 'NONE',  #17016 ) ;
#67334 = EDGE_CURVE ( 'NONE', #111831, #3112, #90824, .T. ) ;
#67335 = LINE ( 'NONE', #107293, #19333 ) ;
#67336 = CARTESIAN_POINT ( 'NONE',  ( -1.700000000000035261, 2.500000000000000000, 4.230127018922196669 ) ) ;
#67337 = AXIS2_PLACEMENT_3D ( 'NONE', #22711, #102535, #12845 ) ;
#67338 = CARTESIAN_POINT ( 'NONE',  ( 3.749999999999975131, 2.500000000000000000, 6.395190528383296602 ) ) ;
#67339 = VERTEX_POINT ( 'NONE', #88949 ) ;
#67340 = PLANE ( 'NONE',  #43571 ) ;
#67341 = AXIS2_PLACEMENT_3D ( 'NONE', #76763, #25717, #125845 ) ;
#67342 = VECTOR ( 'NONE', #49840, 1000.000000000000000 ) ;
#67343 = CARTESIAN_POINT ( 'NONE',  ( 1.899999999999951283, 12.50000000000000000, 0.3464101615137736845 ) ) ;
#67344 = AXIS2_PLACEMENT_3D ( 'NONE', #115054, #45067, #5110 ) ;
#67345 = VERTEX_POINT ( 'NONE', #67331 ) ;
#67346 = CIRCLE ( 'NONE', #75977, 0.06509327318403745899 ) ;
#67347 = AXIS2_PLACEMENT_3D ( 'NONE', #8561, #48511, #50438 ) ;
#67348 = ORIENTED_EDGE ( 'NONE', *, *, #59850, .F. ) ;
#67349 = CIRCLE ( 'NONE', #58987, 0.1000000000000002554 ) ;
#67350 = AXIS2_PLACEMENT_3D ( 'NONE', #66055, #47082, #4530 ) ;
#67351 = EDGE_LOOP ( 'NONE', ( #60372, #35452, #61483, #66355 ) ) ;
#67352 = ORIENTED_EDGE ( 'NONE', *, *, #78463, .T. ) ;
#67353 = DIRECTION ( 'NONE',  ( 0.000000000000000000, -0.000000000000000000, 1.000000000000000000 ) ) ;
#67354 = DIRECTION ( 'NONE',  ( 0.000000000000000000, -0.000000000000000000, 1.000000000000000000 ) ) ;
#67355 = AXIS2_PLACEMENT_3D ( 'NONE', #13592, #82370, #103288 ) ;
#67356 = ORIENTED_EDGE ( 'NONE', *, *, #85429, .F. ) ;
#67357 = FACE_OUTER_BOUND ( 'NONE', #31003, .T. ) ;
#67358 = DIRECTION ( 'NONE',  ( 0.000000000000000000, 0.000000000000000000, 1.000000000000000000 ) ) ;
#67359 = DIRECTION ( 'NONE',  ( -0.000000000000000000, -1.000000000000000000, -0.000000000000000000 ) ) ;
#67360 = ORIENTED_EDGE ( 'NONE', *, *, #16686, .T. ) ;
#67361 = PLANE ( 'NONE',  #128948 ) ;
#67362 = PLANE ( 'NONE',  #31190 ) ;
#67363 = EDGE_LOOP ( 'NONE', ( #50015, #85594, #114656, #44344 ) ) ;
#67364 = ORIENTED_EDGE ( 'NONE', *, *, #128566, .F. ) ;
#67365 = EDGE_LOOP ( 'NONE', ( #72235, #88901 ) ) ;
#67366 = DIRECTION ( 'NONE',  ( 0.000000000000000000, 0.000000000000000000, 1.000000000000000000 ) ) ;
#67367 = AXIS2_PLACEMENT_3D ( 'NONE', #90579, #78858, #99771 ) ;
#67368 = CARTESIAN_POINT ( 'NONE',  ( 8.949999999999921130, 2.500000000000000000, -6.941600689897078347 ) ) ;
#67369 = EDGE_CURVE ( 'NONE', #77424, #89750, #113817, .T. ) ;
#67370 = EDGE_LOOP ( 'NONE', ( #35435, #51609 ) ) ;
#67371 = CARTESIAN_POINT ( 'NONE',  ( 3.549999999999940314, 12.50000000000000000, 6.841600689897072485 ) ) ;
#67372 = CARTESIAN_POINT ( 'NONE',  ( 129.5000000000000000, 0.000000000000000000, 0.000000000000000000 ) ) ;
#67373 = EDGE_CURVE ( 'NONE', #50205, #61413, #99153, .T. ) ;
#67374 = DIRECTION ( 'NONE',  ( -0.000000000000000000, 1.000000000000000000, -0.000000000000000000 ) ) ;
#67375 = DIRECTION ( 'NONE',  ( -1.000000000000000000, -0.000000000000000000, -0.000000000000000000 ) ) ;
#67376 = VECTOR ( 'NONE', #23969, 1000.000000000000000 ) ;
#67377 = EDGE_CURVE ( 'NONE', #1255, #76788, #57381, .T. ) ;
#67378 = AXIS2_PLACEMENT_3D ( 'NONE', #61085, #41469, #80080 ) ;
#67379 = VERTEX_POINT ( 'NONE', #39236 ) ;
#67380 = DIRECTION ( 'NONE',  ( -0.000000000000000000, -1.000000000000000000, -0.000000000000000000 ) ) ;
#67381 = CONICAL_SURFACE ( 'NONE', #42392, 0.09999999999999999167, 0.003490658503988666988 ) ;
#67382 = ORIENTED_EDGE ( 'NONE', *, *, #98076, .F. ) ;
#67383 = EDGE_CURVE ( 'NONE', #11772, #80189, #25996, .T. ) ;
#67385 = ORIENTED_EDGE ( 'NONE', *, *, #12454, .T. ) ;
#67384 = ADVANCED_FACE ( 'NONE', ( #29395 ), #7185, .T. ) ;
#67386 = DIRECTION ( 'NONE',  ( 0.000000000000000000, 0.000000000000000000, 1.000000000000000000 ) ) ;
#67387 = EDGE_CURVE ( 'NONE', #97216, #129104, #67837, .T. ) ;
#67389 = EDGE_CURVE ( 'NONE', #127947, #31361, #39869, .T. ) ;
#67388 = DIRECTION ( 'NONE',  ( 0.000000000000000000, 0.000000000000000000, 1.000000000000000000 ) ) ;
#67390 = EDGE_CURVE ( 'NONE', #121812, #113368, #96818, .T. ) ;
#67391 = FACE_BOUND ( 'NONE', #126169, .T. ) ;
#67392 = LINE ( 'NONE', #117146, #101521 ) ;
#67394 = CARTESIAN_POINT ( 'NONE',  ( -6.050000000000020250, 2.500000000000000000, -2.411473670974877859 ) ) ;
#67393 = AXIS2_PLACEMENT_3D ( 'NONE', #20265, #9800, #58907 ) ;
#67396 = DIRECTION ( 'NONE',  ( -0.000000000000000000, 1.000000000000000000, -0.000000000000000000 ) ) ;
#67395 = CONICAL_SURFACE ( 'NONE', #10973, 0.1000000000000002554, 0.003490658503988666988 ) ;
#67397 = CIRCLE ( 'NONE', #521, 0.09999999999999982514 ) ;
#67398 = VECTOR ( 'NONE', #22312, 1000.000000000000000 ) ;
#67399 = AXIS2_PLACEMENT_3D ( 'NONE', #20967, #1958, #41912 ) ;
#67400 = ORIENTED_EDGE ( 'NONE', *, *, #81365, .T. ) ;
#67401 = CARTESIAN_POINT ( 'NONE',  ( -8.750000000000008882, 2.500000000000000000, -2.757883832488654097 ) ) ;
#67402 = DIRECTION ( 'NONE',  ( 0.000000000000000000, 0.000000000000000000, 1.000000000000000000 ) ) ;
#67403 = EDGE_CURVE ( 'NONE', #107678, #120135, #65684, .T. ) ;
#67404 = CARTESIAN_POINT ( 'NONE',  ( 14.34999999999989306, 2.500000000000000000, -2.511473670974877948 ) ) ;
#67405 = CIRCLE ( 'NONE', #25670, 0.1000000000000002554 ) ;
#67406 = CARTESIAN_POINT ( 'NONE',  ( -3.950000000000026379, 2.500000000000000000, 2.411473670974873862 ) ) ;
#67407 = EDGE_LOOP ( 'NONE', ( #12990, #33191, #47753, #44122 ) ) ;
#67408 = CARTESIAN_POINT ( 'NONE',  ( 3.349999999999944578, 12.50000000000000000, -5.737276932171712751 ) ) ;
#67409 = PLANE ( 'NONE',  #89234 ) ;
#67410 = AXIS2_PLACEMENT_3D ( 'NONE', #11762, #12404, #121079 ) ;
#67411 = VERTEX_POINT ( 'NONE', #117093 ) ;
#67412 = DIRECTION ( 'NONE',  ( -0.000000000000000000, 1.000000000000000000, -0.000000000000000000 ) ) ;
#67413 = CARTESIAN_POINT ( 'NONE',  ( -12.09999999999999609, 2.500000000000000000, -0.7928203230275502333 ) ) ;
#67414 = FACE_BOUND ( 'NONE', #100850, .T. ) ;
#67415 = DIRECTION ( 'NONE',  ( 0.000000000000000000, 0.000000000000000000, 1.000000000000000000 ) ) ;
#67416 = ORIENTED_EDGE ( 'NONE', *, *, #128664, .F. ) ;
#67417 = PLANE ( 'NONE',  #46590 ) ;
#67418 = VERTEX_POINT ( 'NONE', #66711 ) ;
#67419 = VERTEX_POINT ( 'NONE', #7141 ) ;
#67421 = CIRCLE ( 'NONE', #23631, 0.06509327318403741736 ) ;
#67420 = CARTESIAN_POINT ( 'NONE',  ( 19.52519901027835658, 0.5909487300084670380, -4.333354523369935762 ) ) ;
#67422 = CARTESIAN_POINT ( 'NONE',  ( 185.9583333333333428, 4.445597072760117285, 7.699999999999999289 ) ) ;
#67423 = ORIENTED_EDGE ( 'NONE', *, *, #38207, .T. ) ;
#67424 = CARTESIAN_POINT ( 'NONE',  ( -8.150000000000009237, 2.500000000000000000, 6.148780366869520009 ) ) ;
#67425 = LINE ( 'NONE', #68748, #17695 ) ;
#67426 = AXIS2_PLACEMENT_3D ( 'NONE', #44770, #2235, #24474 ) ;
#67427 = AXIS2_PLACEMENT_3D ( 'NONE', #1044, #81545, #113586 ) ;
#67428 = EDGE_CURVE ( 'NONE', #123090, #42074, #943, .T. ) ;
#67429 = LINE ( 'NONE', #37378, #50629 ) ;
#67430 = EDGE_CURVE ( 'NONE', #39604, #116494, #115862, .T. ) ;
#67431 = AXIS2_PLACEMENT_3D ( 'NONE', #33420, #123076, #85075 ) ;
#67433 = VERTEX_POINT ( 'NONE', #78504 ) ;
#67432 = CONICAL_SURFACE ( 'NONE', #105019, 0.09999999999999982514, 0.003490658503988666988 ) ;
#67434 = EDGE_CURVE ( 'NONE', #122576, #67250, #47740, .T. ) ;
#67435 = AXIS2_PLACEMENT_3D ( 'NONE', #35684, #106349, #16656 ) ;
#67436 = FILL_AREA_STYLE_COLOUR ( '', #50873 ) ;
#67437 = DIRECTION ( 'NONE',  ( 0.000000000000000000, 1.000000000000000000, 0.000000000000000000 ) ) ;
#67438 = DIRECTION ( 'NONE',  ( 0.000000000000000000, 1.000000000000000000, 0.000000000000000000 ) ) ;
#67439 = VECTOR ( 'NONE', #53187, 1000.000000000000000 ) ;
#67440 = CARTESIAN_POINT ( 'NONE',  ( 12.04999999999990479, 2.500000000000000000, -6.495190528383302464 ) ) ;
#67442 = ORIENTED_EDGE ( 'NONE', *, *, #128425, .T. ) ;
#67441 = CONICAL_SURFACE ( 'NONE', #27761, 0.1000000000000000472, 0.003490658503988666988 ) ;
#67444 = CIRCLE ( 'NONE', #61521, 2.750000000000002665 ) ;
#67443 = CARTESIAN_POINT ( 'NONE',  ( -2.950000000000030376, 2.500000000000000000, 6.495190528383297135 ) ) ;
#67445 = VERTEX_POINT ( 'NONE', #68009 ) ;
#67446 = EDGE_CURVE ( 'NONE', #61230, #96281, #18266, .T. ) ;
#67447 = DIRECTION ( 'NONE',  ( 0.000000000000000000, 0.000000000000000000, -1.000000000000000000 ) ) ;
#67448 = CONICAL_SURFACE ( 'NONE', #90558, 0.1000000000000002554, 0.003490658503988666988 ) ;
#67450 = ORIENTED_EDGE ( 'NONE', *, *, #99395, .T. ) ;
#67449 = EDGE_CURVE ( 'NONE', #120047, #66944, #17655, .T. ) ;
#67451 = CARTESIAN_POINT ( 'NONE',  ( 6.649999999999930189, 2.500000000000000000, 7.288010851410849256 ) ) ;
#67452 = DIRECTION ( 'NONE',  ( -0.000000000000000000, 1.000000000000000000, -0.000000000000000000 ) ) ;
#67453 = ADVANCED_FACE ( 'NONE', ( #18901 ), #71896, .T. ) ;
#67454 = CARTESIAN_POINT ( 'NONE',  ( 7.899999999999924860, 2.500000000000000000, -3.637306695894650055 ) ) ;
#67455 = EDGE_CURVE ( 'NONE', #122964, #56169, #2476, .T. ) ;
#67456 = DIRECTION ( 'NONE',  ( 0.000000000000000000, -0.9999939076577903929, 0.003490651415223739937 ) ) ;
#67457 = ORIENTED_EDGE ( 'NONE', *, *, #115906, .T. ) ;
#67458 = DIRECTION ( 'NONE',  ( -4.274815082592931898E-19, -0.9999939076577903929, -0.003490651415223739937 ) ) ;
#67459 = DIRECTION ( 'NONE',  ( 0.000000000000000000, 1.000000000000000000, 0.000000000000000000 ) ) ;
#67460 = CARTESIAN_POINT ( 'NONE',  ( 185.1927083336747160, 6.551208109652275624, -3.782341765624998686 ) ) ;
#67461 = CARTESIAN_POINT ( 'NONE',  ( 3.299999999999944755, 2.500000000000000000, 0.09999999999999761857 ) ) ;
#67463 = EDGE_CURVE ( 'NONE', #71667, #108330, #55236, .T. ) ;
#67462 = PLANE ( 'NONE',  #51570 ) ;
#67464 = AXIS2_PLACEMENT_3D ( 'NONE', #35711, #16682, #16042 ) ;
#67465 = ORIENTED_EDGE ( 'NONE', *, *, #106873, .T. ) ;
#67466 = EDGE_LOOP ( 'NONE', ( #57811, #4080, #62653, #89555 ) ) ;
#67467 = DIRECTION ( 'NONE',  ( 0.000000000000000000, 0.000000000000000000, 1.000000000000000000 ) ) ;
#67468 = EDGE_LOOP ( 'NONE', ( #93958, #45804, #112693, #34745 ) ) ;
#67469 = PLANE ( 'NONE',  #59783 ) ;
#67471 = ORIENTED_EDGE ( 'NONE', *, *, #126328, .T. ) ;
#67470 = ORIENTED_EDGE ( 'NONE', *, *, #123164, .T. ) ;
#67472 = ORIENTED_EDGE ( 'NONE', *, *, #13506, .T. ) ;
#67473 = DIRECTION ( 'NONE',  ( 0.000000000000000000, 1.000000000000000000, 0.000000000000000000 ) ) ;
#67474 = AXIS2_PLACEMENT_3D ( 'NONE', #124109, #65172, #34465 ) ;
#67475 = CARTESIAN_POINT ( 'NONE',  ( -9.400000000000009237, 2.500000000000000000, -4.083716857408422385 ) ) ;
#67476 = CIRCLE ( 'NONE', #27783, 0.1000000000000002554 ) ;
#67477 = DIRECTION ( 'NONE',  ( -0.000000000000000000, 1.000000000000000000, -0.000000000000000000 ) ) ;
#67478 =( LENGTH_UNIT ( ) NAMED_UNIT ( * ) SI_UNIT ( .MILLI., .METRE. ) );
#67479 = CARTESIAN_POINT ( 'NONE',  ( -8.150000000000014566, 2.500000000000000000, -6.148780366869520897 ) ) ;
#67480 = CARTESIAN_POINT ( 'NONE',  ( -9.600000000000006750, 2.500000000000000000, 0.5928203230275495006 ) ) ;
#67481 = CARTESIAN_POINT ( 'NONE',  ( 12.69999999999990159, 2.500000000000000000, 4.676537180435972552 ) ) ;
#67482 = FACE_OUTER_BOUND ( 'NONE', #40058, .T. ) ;
#67483 = EDGE_CURVE ( 'NONE', #128073, #77956, #23939, .T. ) ;
#67484 = ORIENTED_EDGE ( 'NONE', *, *, #86997, .F. ) ;
#67485 = AXIS2_PLACEMENT_3D ( 'NONE', #105436, #15744, #95612 ) ;
#67486 = AXIS2_PLACEMENT_3D ( 'NONE', #123853, #35501, #15175 ) ;
#67487 = FACE_OUTER_BOUND ( 'NONE', #104974, .T. ) ;
#67488 = EDGE_LOOP ( 'NONE', ( #59156, #110097, #94003, #128152 ) ) ;
#67489 = AXIS2_PLACEMENT_3D ( 'NONE', #58960, #108049, #98226 ) ;
#67490 = ORIENTED_EDGE ( 'NONE', *, *, #109998, .T. ) ;
#67491 = ORIENTED_EDGE ( 'NONE', *, *, #65848, .F. ) ;
#67492 = ORIENTED_EDGE ( 'NONE', *, *, #88137, .T. ) ;
#67493 = CARTESIAN_POINT ( 'NONE',  ( -12.49999999999999467, 12.50000000000000000, 0.7579135962115910452 ) ) ;
#67494 = ORIENTED_EDGE ( 'NONE', *, *, #75683, .F. ) ;
#67495 = ORIENTED_EDGE ( 'NONE', *, *, #119132, .F. ) ;
#67496 = CONICAL_SURFACE ( 'NONE', #25751, 0.09999999999999982514, 0.003490658503988666988 ) ;
#67497 = AXIS2_PLACEMENT_3D ( 'NONE', #80283, #120205, #70456 ) ;
#67498 = DIRECTION ( 'NONE',  ( -0.000000000000000000, -1.000000000000000000, -0.000000000000000000 ) ) ;
#67499 = CARTESIAN_POINT ( 'NONE',  ( -3.749999999999991118, 12.50000000000000000, -2.165063509461101710 ) ) ;
#67500 = ADVANCED_FACE ( 'NONE', ( #1842 ), #111818, .T. ) ;
#67501 = DIRECTION ( 'NONE',  ( 0.000000000000000000, 0.000000000000000000, 1.000000000000000000 ) ) ;
#67502 = AXIS2_PLACEMENT_3D ( 'NONE', #30678, #127568, #88935 ) ;
#67503 = DIRECTION ( 'NONE',  ( 0.000000000000000000, 0.000000000000000000, -1.000000000000000000 ) ) ;
#67504 = AXIS2_PLACEMENT_3D ( 'NONE', #9086, #85707, #125625 ) ;
#67505 = AXIS2_PLACEMENT_3D ( 'NONE', #47063, #56844, #28710 ) ;
#67506 = FACE_OUTER_BOUND ( 'NONE', #78780, .T. ) ;
#67507 = EDGE_LOOP ( 'NONE', ( #4821, #73278 ) ) ;
#67508 = CONICAL_SURFACE ( 'NONE', #6857, 0.09999999999999982514, 0.003490658503988666988 ) ;
#67509 = CARTESIAN_POINT ( 'NONE',  ( -0.2000000000000408673, 12.50000000000000000, -3.918623584224389056 ) ) ;
#67510 = ORIENTED_EDGE ( 'NONE', *, *, #115500, .F. ) ;
#67511 = DIRECTION ( 'NONE',  ( -4.274815082592931898E-19, -0.9999939076577903929, -0.003490651415223739937 ) ) ;
#67512 = ORIENTED_EDGE ( 'NONE', *, *, #12144, .F. ) ;
#67513 = AXIS2_PLACEMENT_3D ( 'NONE', #128846, #88208, #67269 ) ;
#67514 = CARTESIAN_POINT ( 'NONE',  ( 7.049999999999928768, 12.50000000000000000, -2.099970236277064473 ) ) ;
#67515 = ORIENTED_EDGE ( 'NONE', *, *, #98816, .F. ) ;
#67516 = EDGE_CURVE ( 'NONE', #97603, #33814, #107552, .T. ) ;
#67517 = ORIENTED_EDGE ( 'NONE', *, *, #45984, .T. ) ;
#67518 = FACE_OUTER_BOUND ( 'NONE', #2228, .T. ) ;
#67519 = DIRECTION ( 'NONE',  ( 0.000000000000000000, -0.000000000000000000, 1.000000000000000000 ) ) ;
#67520 = CARTESIAN_POINT ( 'NONE',  ( -5.600000000000020073, 12.50000000000000000, 3.983716857408420964 ) ) ;
#67521 = FACE_OUTER_BOUND ( 'NONE', #41082, .T. ) ;
#67522 = B_SPLINE_CURVE_WITH_KNOTS ( 'NONE', 3,
 ( #39711, #10832, #373, #91999, #50157, #60624, #89420, #91349, #121445, #21314 ),
 .UNSPECIFIED., .F., .F.,
 ( 4, 2, 2, 2, 4 ),
 ( -0.0001133383185231292639, 0.01648990952740256311, 0.03309315737332825524, 0.04969640521925394738, 0.06629965306517963952 ),
 .UNSPECIFIED. ) ;
#67523 = CARTESIAN_POINT ( 'NONE',  ( -15.79999999999998117, 2.500000000000000000, -0.1000000000000000056 ) ) ;
#67524 = EDGE_LOOP ( 'NONE', ( #48500, #107212, #119978, #90763 ) ) ;
#67525 = CARTESIAN_POINT ( 'NONE',  ( 4.399999999999939071, 12.50000000000000000, -0.3464101615137782364 ) ) ;
#67527 = AXIS2_PLACEMENT_3D ( 'NONE', #41293, #30835, #40660 ) ;
#67526 = DIRECTION ( 'NONE',  ( 0.000000000000000000, 0.000000000000000000, 1.000000000000000000 ) ) ;
#67528 = AXIS2_PLACEMENT_3D ( 'NONE', #29414, #70617, #81095 ) ;
#67529 = DIRECTION ( 'NONE',  ( -0.000000000000000000, 1.000000000000000000, -0.000000000000000000 ) ) ;
#67530 = FACE_OUTER_BOUND ( 'NONE', #13669, .T. ) ;
#67531 = FACE_OUTER_BOUND ( 'NONE', #37306, .T. ) ;
#67532 = ORIENTED_EDGE ( 'NONE', *, *, #22733, .T. ) ;
#67533 = CONICAL_SURFACE ( 'NONE', #107263, 0.1000000000000002554, 0.003490658503988666988 ) ;
#67534 = AXIS2_PLACEMENT_3D ( 'NONE', #69381, #18353, #99511 ) ;
#67535 = ORIENTED_EDGE ( 'NONE', *, *, #95088, .T. ) ;
#67536 = CONICAL_SURFACE ( 'NONE', #55030, 8.699999999999999289, 0.08726646259971666819 ) ;
#67537 = CIRCLE ( 'NONE', #94746, 0.06509327318403745899 ) ;
#67538 = CARTESIAN_POINT ( 'NONE',  ( 2.049999999999950084, 2.500000000000000000, -6.495190528383302464 ) ) ;
#67539 = ORIENTED_EDGE ( 'NONE', *, *, #20882, .F. ) ;
#67540 = CARTESIAN_POINT ( 'NONE',  ( 14.34999999999989662, 2.500000000000000000, 2.411473670974873862 ) ) ;
#67541 = DIRECTION ( 'NONE',  ( 0.000000000000000000, 1.000000000000000000, 0.000000000000000000 ) ) ;
#67542 = VECTOR ( 'NONE', #57560, 1000.000000000000000 ) ;
#67543 = VECTOR ( 'NONE', #60022, 1000.000000000000000 ) ;
#67545 = EDGE_CURVE ( 'NONE', #69354, #18837, #42435, .T. ) ;
#67544 = AXIS2_PLACEMENT_3D ( 'NONE', #42800, #80770, #3484 ) ;
#67546 = AXIS2_PLACEMENT_3D ( 'NONE', #73770, #3747, #122890 ) ;
#67547 = AXIS2_PLACEMENT_3D ( 'NONE', #89108, #87159, #77355 ) ;
#67548 = ORIENTED_EDGE ( 'NONE', *, *, #100030, .T. ) ;
#67549 = CARTESIAN_POINT ( 'NONE',  ( 185.8333333333333144, 6.668395609140177704, -3.849999999999998312 ) ) ;
#67550 = CARTESIAN_POINT ( 'NONE',  ( 10.59999999999990905, 2.500000000000000000, 4.083716857408420609 ) ) ;
#67551 = DIRECTION ( 'NONE',  ( 0.000000000000000000, 0.000000000000000000, 1.000000000000000000 ) ) ;
#67552 = CARTESIAN_POINT ( 'NONE',  ( 14.14999999999989377, 12.50000000000000000, -1.472243186433550122 ) ) ;
#67553 = EDGE_LOOP ( 'NONE', ( #91649, #44374 ) ) ;
#67555 = EDGE_CURVE ( 'NONE', #46396, #108554, #97084, .T. ) ;
#67554 = AXIS2_PLACEMENT_3D ( 'NONE', #38091, #77373, #35523 ) ;
#67556 = DIRECTION ( 'NONE',  ( 0.000000000000000000, 1.000000000000000000, 0.000000000000000000 ) ) ;
#67557 = DIRECTION ( 'NONE',  ( -0.000000000000000000, 1.000000000000000000, -0.000000000000000000 ) ) ;
#67558 = ORIENTED_EDGE ( 'NONE', *, *, #31029, .F. ) ;
#67559 = EDGE_CURVE ( 'NONE', #15257, #58594, #81694, .T. ) ;
#67560 = EDGE_CURVE ( 'NONE', #59645, #125100, #31332, .T. ) ;
#67561 = EDGE_CURVE ( 'NONE', #67674, #87604, #51135, .T. ) ;
#67563 = EDGE_CURVE ( 'NONE', #125412, #6322, #101352, .T. ) ;
#67562 = CARTESIAN_POINT ( 'NONE',  ( -1.900000000000034106, 2.500000000000000000, -4.083716857408426826 ) ) ;
#67564 = CARTESIAN_POINT ( 'NONE',  ( 6.849999999999927702, 12.50000000000000000, 1.818653347947321475 ) ) ;
#67565 = DIRECTION ( 'NONE',  ( 0.000000000000000000, 0.000000000000000000, 1.000000000000000000 ) ) ;
#67566 = CIRCLE ( 'NONE', #71800, 0.09999999999999999167 ) ;
#67567 = EDGE_LOOP ( 'NONE', ( #99416, #32634 ) ) ;
#67568 = DIRECTION ( 'NONE',  ( 0.000000000000000000, 1.000000000000000000, 0.000000000000000000 ) ) ;
#67569 = ORIENTED_EDGE ( 'NONE', *, *, #77912, .T. ) ;
#67570 = DIRECTION ( 'NONE',  ( 0.000000000000000000, -0.000000000000000000, 1.000000000000000000 ) ) ;
#67571 = DIRECTION ( 'NONE',  ( 0.000000000000000000, 0.000000000000000000, 1.000000000000000000 ) ) ;
#67572 = EDGE_CURVE ( 'NONE', #54801, #120522, #30209, .T. ) ;
#67573 = DIRECTION ( 'NONE',  ( -0.000000000000000000, 1.000000000000000000, -0.000000000000000000 ) ) ;
#67574 = AXIS2_PLACEMENT_3D ( 'NONE', #26047, #13631, #3195 ) ;
#67575 = VERTEX_POINT ( 'NONE', #100059 ) ;
#67577 = EDGE_CURVE ( 'NONE', #25440, #39251, #120081, .T. ) ;
#67576 = AXIS2_PLACEMENT_3D ( 'NONE', #34316, #74869, #95151 ) ;
#67578 = CIRCLE ( 'NONE', #48738, 0.1000000000000000472 ) ;
#67580 = ADVANCED_FACE ( 'NONE', ( #10383 ), #28138, .T. ) ;
#67579 = CARTESIAN_POINT ( 'NONE',  ( -12.04999999999999538, 12.50000000000000000, 6.495190528383297135 ) ) ;
#67581 = DIRECTION ( 'NONE',  ( 0.000000000000000000, 1.000000000000000000, 0.000000000000000000 ) ) ;
#67582 = ORIENTED_EDGE ( 'NONE', *, *, #80130, .T. ) ;
#67583 = DIRECTION ( 'NONE',  ( -4.274815082592931898E-19, -0.9999939076577903929, -0.003490651415223739937 ) ) ;
#67584 = AXIS2_PLACEMENT_3D ( 'NONE', #1274, #30760, #129609 ) ;
#67585 = ORIENTED_EDGE ( 'NONE', *, *, #51074, .F. ) ;
#67586 = AXIS2_PLACEMENT_3D ( 'NONE', #83639, #20846, #62071 ) ;
#67587 = CARTESIAN_POINT ( 'NONE',  ( -9.150000000000009237, 12.50000000000000000, 1.472243186433545459 ) ) ;
#67588 = AXIS2_PLACEMENT_3D ( 'NONE', #88748, #8241, #116897 ) ;
#67589 = AXIS2_PLACEMENT_3D ( 'NONE', #52128, #20088, #91392 ) ;
#67590 = ORIENTED_EDGE ( 'NONE', *, *, #93787, .T. ) ;
#67591 = DIRECTION ( 'NONE',  ( 0.000000000000000000, 1.000000000000000000, 0.000000000000000000 ) ) ;
#67592 = DIRECTION ( 'NONE',  ( 0.000000000000000000, 0.000000000000000000, 1.000000000000000000 ) ) ;
#67593 = VERTEX_POINT ( 'NONE', #50971 ) ;
#67594 = ORIENTED_EDGE ( 'NONE', *, *, #33258, .T. ) ;
#67595 = VECTOR ( 'NONE', #14177, 1000.000000000000000 ) ;
#67596 = DIRECTION ( 'NONE',  ( 0.000000000000000000, -0.9999939076577903929, 0.003490651415223739937 ) ) ;
#67597 = LINE ( 'NONE', #86598, #75641 ) ;
#67598 = ORIENTED_EDGE ( 'NONE', *, *, #108928, .F. ) ;
#67599 = CARTESIAN_POINT ( 'NONE',  ( -10.40000000000000213, 2.500000000000000000, -0.6928203230275541413 ) ) ;
#67600 = DIRECTION ( 'NONE',  ( -0.000000000000000000, 1.000000000000000000, -0.000000000000000000 ) ) ;
#67601 = AXIS2_PLACEMENT_3D ( 'NONE', #30429, #117454, #99795 ) ;
#67602 = CONICAL_SURFACE ( 'NONE', #11176, 0.1000000000000000056, 0.003490658503988666988 ) ;
#67603 = VECTOR ( 'NONE', #118858, 1000.000000000000000 ) ;
#67604 = DIRECTION ( 'NONE',  ( -0.000000000000000000, -1.000000000000000000, -0.000000000000000000 ) ) ;
#67605 = CARTESIAN_POINT ( 'NONE',  ( 3.099999999999945022, 2.500000000000000000, -4.776537180435978414 ) ) ;
#67606 = DIRECTION ( 'NONE',  ( 0.000000000000000000, 0.000000000000000000, 1.000000000000000000 ) ) ;
#67607 = FACE_OUTER_BOUND ( 'NONE', #22289, .T. ) ;
#67608 = ORIENTED_EDGE ( 'NONE', *, *, #115570, .F. ) ;
#67609 = ORIENTED_EDGE ( 'NONE', *, *, #20947, .T. ) ;
#67610 = VERTEX_POINT ( 'NONE', #80426 ) ;
#67611 = ORIENTED_EDGE ( 'NONE', *, *, #3513, .F. ) ;
#67612 = LINE ( 'NONE', #66333, #72609 ) ;
#67613 = CARTESIAN_POINT ( 'NONE',  ( 9.349999999999916156, 2.500000000000000000, 6.841600689897072485 ) ) ;
#67614 = DIRECTION ( 'NONE',  ( -0.000000000000000000, -1.000000000000000000, -0.000000000000000000 ) ) ;
#67615 = ORIENTED_EDGE ( 'NONE', *, *, #54700, .T. ) ;
#67616 = FACE_BOUND ( 'NONE', #74253, .T. ) ;
#67617 = ORIENTED_EDGE ( 'NONE', *, *, #129605, .F. ) ;
#67618 = EDGE_CURVE ( 'NONE', #92344, #118717, #32638, .T. ) ;
#67619 = PLANE ( 'NONE',  #35475 ) ;
#67620 = DIRECTION ( 'NONE',  ( 0.000000000000000000, -0.9999939076577903929, 0.003490651415223739937 ) ) ;
#67621 = EDGE_CURVE ( 'NONE', #20397, #97989, #128417, .T. ) ;
#67622 = CARTESIAN_POINT ( 'NONE',  ( 87.50000000000001421, 0.000000000000000000, 0.000000000000000000 ) ) ;
#67623 = DIRECTION ( 'NONE',  ( -0.000000000000000000, 1.000000000000000000, -0.000000000000000000 ) ) ;
#67624 = EDGE_CURVE ( 'NONE', #91497, #15344, #32275, .T. ) ;
#67625 = CARTESIAN_POINT ( 'NONE',  ( 16.32066102237043737, -2.500000000000000000, 4.877377760480507085 ) ) ;
#67626 = LINE ( 'NONE', #85971, #10030 ) ;
#67627 = DIRECTION ( 'NONE',  ( 0.000000000000000000, 1.000000000000000000, 0.000000000000000000 ) ) ;
#67628 = CARTESIAN_POINT ( 'NONE',  ( 10.39999999999991154, 2.500000000000000000, 3.737306695894644371 ) ) ;
#67629 = AXIS2_PLACEMENT_3D ( 'NONE', #53035, #44492, #43231 ) ;
#67630 = AXIS2_PLACEMENT_3D ( 'NONE', #20232, #99449, #129571 ) ;
#67631 = CARTESIAN_POINT ( 'NONE',  ( -1.050000000000038680, 2.500000000000000000, 2.611473670974873151 ) ) ;
#67633 = EDGE_CURVE ( 'NONE', #106590, #106830, #122146, .T. ) ;
#67632 = DIRECTION ( 'NONE',  ( 0.000000000000000000, 0.000000000000000000, 1.000000000000000000 ) ) ;
#67634 = AXIS2_PLACEMENT_3D ( 'NONE', #99146, #42151, #31687 ) ;
#67636 = ORIENTED_EDGE ( 'NONE', *, *, #42685, .T. ) ;
#67635 = CONICAL_SURFACE ( 'NONE', #46722, 0.09999999999999982514, 0.003490658503988666988 ) ;
#67637 = ORIENTED_EDGE ( 'NONE', *, *, #56224, .F. ) ;
#67638 = ORIENTED_EDGE ( 'NONE', *, *, #34660, .F. ) ;
#67639 = AXIS2_PLACEMENT_3D ( 'NONE', #44441, #84364, #124296 ) ;
#67640 = ORIENTED_EDGE ( 'NONE', *, *, #27569, .F. ) ;
#67642 = AXIS2_PLACEMENT_3D ( 'NONE', #23373, #72504, #82321 ) ;
#67641 = CARTESIAN_POINT ( 'NONE',  ( 16.73289298692360205, -0.7002450284381240841, -5.897165230078514675 ) ) ;
#67643 = CARTESIAN_POINT ( 'NONE',  ( -11.84999999999999609, 2.500000000000000000, 6.048780366869521252 ) ) ;
#67645 = ORIENTED_EDGE ( 'NONE', *, *, #15962, .T. ) ;
#67644 = EDGE_LOOP ( 'NONE', ( #11360, #60414, #2032, #49077 ) ) ;
#67646 = ORIENTED_EDGE ( 'NONE', *, *, #78717, .T. ) ;
#67647 = CARTESIAN_POINT ( 'NONE',  ( 115.5000000000000000, -2.000000000000000000, -1.999999999999997335 ) ) ;
#67648 = AXIS2_PLACEMENT_3D ( 'NONE', #72088, #112008, #121172 ) ;
#67649 = AXIS2_PLACEMENT_3D ( 'NONE', #127866, #192, #89235 ) ;
#67650 = AXIS2_PLACEMENT_3D ( 'NONE', #104318, #97715, #80669 ) ;
#67651 = PLANE ( 'NONE',  #56055 ) ;
#67652 = DIRECTION ( 'NONE',  ( 0.000000000000000000, 1.000000000000000000, 0.000000000000000000 ) ) ;
#67653 = DIRECTION ( 'NONE',  ( -0.000000000000000000, 1.000000000000000000, -0.000000000000000000 ) ) ;
#67654 = DIRECTION ( 'NONE',  ( 0.000000000000000000, 1.000000000000000000, 0.000000000000000000 ) ) ;
#67655 = VECTOR ( 'NONE', #76555, 1000.000000000000000 ) ;
#67656 = DIRECTION ( 'NONE',  ( 0.000000000000000000, 0.000000000000000000, 1.000000000000000000 ) ) ;
#67657 = EDGE_CURVE ( 'NONE', #95313, #115297, #13543, .T. ) ;
#67658 = ORIENTED_EDGE ( 'NONE', *, *, #49920, .F. ) ;
#67659 = CARTESIAN_POINT ( 'NONE',  ( -10.84999999999999964, 12.50000000000000000, 5.802370205355744659 ) ) ;
#67660 = ORIENTED_EDGE ( 'NONE', *, *, #80124, .F. ) ;
#67661 = VERTEX_POINT ( 'NONE', #75734 ) ;
#67662 = ORIENTED_EDGE ( 'NONE', *, *, #33871, .T. ) ;
#67663 = DIRECTION ( 'NONE',  ( 0.000000000000000000, 0.000000000000000000, -1.000000000000000000 ) ) ;
#67664 = EDGE_LOOP ( 'NONE', ( #64222, #51714, #50274, #117383 ) ) ;
#67665 = ORIENTED_EDGE ( 'NONE', *, *, #120914, .T. ) ;
#67666 = CIRCLE ( 'NONE', #32197, 0.06509327318403745899 ) ;
#67667 = LINE ( 'NONE', #118711, #12929 ) ;
#67668 = DIRECTION ( 'NONE',  ( -0.000000000000000000, 1.000000000000000000, -0.000000000000000000 ) ) ;
#67669 = DIRECTION ( 'NONE',  ( -4.274815082592931898E-19, -0.9999939076577903929, -0.003490651415223739937 ) ) ;
#67670 = EDGE_CURVE ( 'NONE', #31226, #3120, #7280, .T. ) ;
#67671 = CARTESIAN_POINT ( 'NONE',  ( 108.0000000000000142, 8.500000000000000000, -0.2500000000000000000 ) ) ;
#67672 = PLANE ( 'NONE',  #16219 ) ;
#67674 = VERTEX_POINT ( 'NONE', #53541 ) ;
#67673 = AXIS2_PLACEMENT_3D ( 'NONE', #122168, #79646, #61310 ) ;
#67675 = DIRECTION ( 'NONE',  ( 0.000000000000000000, 0.000000000000000000, -1.000000000000000000 ) ) ;
#67676 = AXIS2_PLACEMENT_3D ( 'NONE', #62951, #70841, #31567 ) ;
#67677 = CIRCLE ( 'NONE', #34261, 0.06509327318403745899 ) ;
#67678 = VERTEX_POINT ( 'NONE', #54183 ) ;
#67679 = DIRECTION ( 'NONE',  ( 0.000000000000000000, 0.000000000000000000, 1.000000000000000000 ) ) ;
#67680 = EDGE_LOOP ( 'NONE', ( #51556, #42129, #128423, #71351 ) ) ;
#67681 = CARTESIAN_POINT ( 'NONE',  ( 110.2384023472883143, 7.457657641414515481, -4.482797374978448879 ) ) ;
#67682 = DIRECTION ( 'NONE',  ( 0.000000000000000000, 0.000000000000000000, -1.000000000000000000 ) ) ;
#67683 = ORIENTED_EDGE ( 'NONE', *, *, #61871, .T. ) ;
#67684 = DIRECTION ( 'NONE',  ( -4.274815082592931898E-19, -0.9999939076577903929, -0.003490651415223739937 ) ) ;
#67685 = ADVANCED_FACE ( 'NONE', ( #93454 ), #59562, .T. ) ;
#67687 = CONICAL_SURFACE ( 'NONE', #36415, 0.1000000000000002554, 0.003490658503988666988 ) ;
#67686 = DIRECTION ( 'NONE',  ( 0.000000000000000000, -0.9999939076577903929, 0.003490651415223739937 ) ) ;
#67688 = ORIENTED_EDGE ( 'NONE', *, *, #50674, .F. ) ;
#67689 = CIRCLE ( 'NONE', #17196, 0.09999999999999982514 ) ;
#67690 = AXIS2_PLACEMENT_3D ( 'NONE', #104437, #43604, #103800 ) ;
#67691 = LINE ( 'NONE', #108270, #113531 ) ;
#67692 = EDGE_LOOP ( 'NONE', ( #35360, #29536 ) ) ;
#67694 = VERTEX_POINT ( 'NONE', #113751 ) ;
#67693 = EDGE_CURVE ( 'NONE', #67035, #97177, #95130, .T. ) ;
#67695 = PLANE ( 'NONE',  #1672 ) ;
#67696 = CARTESIAN_POINT ( 'NONE',  ( -0.4000000000000331624, 2.500000000000000000, -0.1000000000000000056 ) ) ;
#67697 = CARTESIAN_POINT ( 'NONE',  ( 186.5052083336747444, -6.551208109652278289, 3.782341765624995134 ) ) ;
#67698 = AXIS2_PLACEMENT_3D ( 'NONE', #28533, #336, #9538 ) ;
#67699 = CARTESIAN_POINT ( 'NONE',  ( -5.000000000000023093, 12.50000000000000000, 0.7579135962115869374 ) ) ;
#67700 = CARTESIAN_POINT ( 'NONE',  ( -5.600000000000020073, 2.500000000000000000, 0.3464101615137736845 ) ) ;
#67701 = CIRCLE ( 'NONE', #61471, 0.1000000000000002554 ) ;
#67702 = VECTOR ( 'NONE', #11993, 1000.000000000000000 ) ;
#67703 = AXIS2_PLACEMENT_3D ( 'NONE', #88515, #69524, #78730 ) ;
#67704 = DIRECTION ( 'NONE',  ( 0.000000000000000000, 0.000000000000000000, 1.000000000000000000 ) ) ;
#67705 = AXIS2_PLACEMENT_3D ( 'NONE', #27067, #118656, #159 ) ;
#67706 = ORIENTED_EDGE ( 'NONE', *, *, #97464, .F. ) ;
#67707 = DIRECTION ( 'NONE',  ( 0.000000000000000000, 1.000000000000000000, 0.000000000000000000 ) ) ;
#67708 = LINE ( 'NONE', #48088, #14445 ) ;
#67709 = EDGE_CURVE ( 'NONE', #11527, #99935, #42835, .T. ) ;
#67710 = VERTEX_POINT ( 'NONE', #96030 ) ;
#67711 = DIRECTION ( 'NONE',  ( 0.000000000000000000, 0.000000000000000000, 1.000000000000000000 ) ) ;
#67712 = DIRECTION ( 'NONE',  ( 1.000000000000000000, 0.000000000000000000, 0.000000000000000000 ) ) ;
#67713 = CARTESIAN_POINT ( 'NONE',  ( -8.750000000000008882, 12.50000000000000000, -2.922977105672691422 ) ) ;
#67714 = DIRECTION ( 'NONE',  ( 0.000000000000000000, 0.000000000000000000, 1.000000000000000000 ) ) ;
#67715 = DIRECTION ( 'NONE',  ( 0.000000000000000000, 1.000000000000000000, 0.000000000000000000 ) ) ;
#67716 = ORIENTED_EDGE ( 'NONE', *, *, #49588, .T. ) ;
#67717 = EDGE_CURVE ( 'NONE', #60832, #26300, #14859, .T. ) ;
#67718 = DIRECTION ( 'NONE',  ( -0.000000000000000000, 1.000000000000000000, -0.000000000000000000 ) ) ;
#67719 = CARTESIAN_POINT ( 'NONE',  ( 6.899999999999928413, 12.50000000000000000, -4.676537180435977881 ) ) ;
#67720 = AXIS2_PLACEMENT_3D ( 'NONE', #61756, #218, #40174 ) ;
#67721 = AXIS2_PLACEMENT_3D ( 'NONE', #5047, #26636, #56083 ) ;
#67722 = EDGE_CURVE ( 'NONE', #87229, #23494, #40769, .T. ) ;
#67723 = AXIS2_PLACEMENT_3D ( 'NONE', #71996, #51710, #43191 ) ;
#67724 = ADVANCED_FACE ( 'NONE', ( #45656 ), #65264, .T. ) ;
#67725 = EDGE_CURVE ( 'NONE', #125960, #56674, #109712, .T. ) ;
#67726 = EDGE_CURVE ( 'NONE', #55502, #12752, #43736, .T. ) ;
#67727 = ORIENTED_EDGE ( 'NONE', *, *, #79718, .F. ) ;
#67728 = DIRECTION ( 'NONE',  ( -0.000000000000000000, 1.000000000000000000, -0.000000000000000000 ) ) ;
#67729 = VECTOR ( 'NONE', #117966, 1000.000000000000000 ) ;
#67730 = AXIS2_PLACEMENT_3D ( 'NONE', #99914, #118899, #80274 ) ;
#67731 = ORIENTED_EDGE ( 'NONE', *, *, #58992, .T. ) ;
#67732 = AXIS2_PLACEMENT_3D ( 'NONE', #19925, #121329, #72885 ) ;
#67733 = ORIENTED_EDGE ( 'NONE', *, *, #65325, .T. ) ;
#67734 = DIRECTION ( 'NONE',  ( 0.000000000000000000, -0.000000000000000000, -1.000000000000000000 ) ) ;
#67735 = ADVANCED_FACE ( 'NONE', ( #44346 ), #34507, .T. ) ;
#67736 = EDGE_CURVE ( 'NONE', #20628, #126381, #101392, .T. ) ;
#67737 = ORIENTED_EDGE ( 'NONE', *, *, #41235, .F. ) ;
#67738 = LINE ( 'NONE', #6859, #117545 ) ;
#67739 = CARTESIAN_POINT ( 'NONE',  ( 13.14999999999990088, 12.50000000000000000, 1.818653347947321475 ) ) ;
#67740 = ADVANCED_FACE ( 'NONE', ( #124851 ), #24720, .T. ) ;
#67741 = DIRECTION ( 'NONE',  ( -0.000000000000000000, -1.000000000000000000, -0.000000000000000000 ) ) ;
#67743 = ORIENTED_EDGE ( 'NONE', *, *, #87871, .T. ) ;
#67742 = VECTOR ( 'NONE', #115695, 1000.000000000000000 ) ;
#67744 = EDGE_CURVE ( 'NONE', #9132, #94097, #36560, .T. ) ;
#67745 = AXIS2_PLACEMENT_3D ( 'NONE', #5989, #67477, #25005 ) ;
#67746 = CONICAL_SURFACE ( 'NONE', #11318, 0.09999999999999982514, 0.003490658503988666988 ) ;
#67748 = EDGE_CURVE ( 'NONE', #12970, #120897, #61687, .T. ) ;
#67747 = FACE_OUTER_BOUND ( 'NONE', #46483, .T. ) ;
#67750 = ORIENTED_EDGE ( 'NONE', *, *, #111511, .T. ) ;
#67749 = DIRECTION ( 'NONE',  ( 0.000000000000000000, 0.000000000000000000, 1.000000000000000000 ) ) ;
#67751 = AXIS2_PLACEMENT_3D ( 'NONE', #101360, #39873, #79775 ) ;
#67752 = CARTESIAN_POINT ( 'NONE',  ( -3.300000000000028244, 12.50000000000000000, 4.330127018922196314 ) ) ;
#67753 = CARTESIAN_POINT ( 'NONE',  ( -1.050000000000037792, 12.50000000000000000, 1.818653347947321475 ) ) ;
#67754 = ADVANCED_FACE ( 'NONE', ( #35824 ), #24029, .T. ) ;
#67755 = EDGE_LOOP ( 'NONE', ( #73320, #9002, #9032, #120132 ) ) ;
#67756 = VERTEX_POINT ( 'NONE', #103284 ) ;
#67757 = VERTEX_POINT ( 'NONE', #122926 ) ;
#67759 = CIRCLE ( 'NONE', #17276, 0.06509327318403745899 ) ;
#67758 = PLANE ( 'NONE',  #16941 ) ;
#67760 = DIRECTION ( 'NONE',  ( 0.000000000000000000, 1.000000000000000000, 0.000000000000000000 ) ) ;
#67761 = DIRECTION ( 'NONE',  ( -4.274815082592931898E-19, -0.9999939076577903929, -0.003490651415223739937 ) ) ;
#67762 = FACE_BOUND ( 'NONE', #10393, .T. ) ;
#67763 = ORIENTED_EDGE ( 'NONE', *, *, #127538, .T. ) ;
#67764 = CARTESIAN_POINT ( 'NONE',  ( 4.999999999999969802, 2.500000000000000000, 4.230127018922196669 ) ) ;
#67765 = DIRECTION ( 'NONE',  ( 0.000000000000000000, 0.000000000000000000, 1.000000000000000000 ) ) ;
#67766 = CIRCLE ( 'NONE', #11339, 0.06509327318403745899 ) ;
#67767 = ORIENTED_EDGE ( 'NONE', *, *, #23658, .F. ) ;
#67768 = DIRECTION ( 'NONE',  ( 0.000000000000000000, 1.000000000000000000, 0.000000000000000000 ) ) ;
#67769 = CARTESIAN_POINT ( 'NONE',  ( -12.09999999999999609, 12.50000000000000000, 4.265033745738159077 ) ) ;
#67770 = DIRECTION ( 'NONE',  ( 0.000000000000000000, 1.000000000000000000, 0.000000000000000000 ) ) ;
#67771 = DIRECTION ( 'NONE',  ( 0.000000000000000000, 1.000000000000000000, 0.000000000000000000 ) ) ;
#67772 = DIRECTION ( 'NONE',  ( -0.000000000000000000, 1.000000000000000000, -0.000000000000000000 ) ) ;
#67773 = CIRCLE ( 'NONE', #17590, 0.06509327318403745899 ) ;
#67774 = AXIS2_PLACEMENT_3D ( 'NONE', #122500, #11887, #73382 ) ;
#67775 = ORIENTED_EDGE ( 'NONE', *, *, #113346, .T. ) ;
#67776 = ORIENTED_EDGE ( 'NONE', *, *, #125367, .T. ) ;
#67777 = EDGE_LOOP ( 'NONE', ( #71152, #127580, #105516, #23490 ) ) ;
#67778 = VERTEX_POINT ( 'NONE', #83644 ) ;
#67779 = ORIENTED_EDGE ( 'NONE', *, *, #105190, .T. ) ;
#67780 = CARTESIAN_POINT ( 'NONE',  ( 0.1999999999999576006, 2.500000000000000000, -4.676537180435978769 ) ) ;
#67781 = CARTESIAN_POINT ( 'NONE',  ( -12.29999999999999361, 2.500000000000000000, 3.883716857408420431 ) ) ;
#67782 = ORIENTED_EDGE ( 'NONE', *, *, #87358, .T. ) ;
#67783 = FACE_BOUND ( 'NONE', #29609, .T. ) ;
#67784 = DIRECTION ( 'NONE',  ( 0.000000000000000000, 0.000000000000000000, -1.000000000000000000 ) ) ;
#67785 = AXIS2_PLACEMENT_3D ( 'NONE', #120066, #110241, #81434 ) ;
#67786 = EDGE_CURVE ( 'NONE', #125792, #59408, #9348, .T. ) ;
#67787 = DIRECTION ( 'NONE',  ( 0.000000000000000000, 0.000000000000000000, 1.000000000000000000 ) ) ;
#67788 = EDGE_CURVE ( 'NONE', #101569, #116415, #128604, .T. ) ;
#67789 = CARTESIAN_POINT ( 'NONE',  ( 184.4999999999999716, -3.021901993692428512, 7.049708900599269690 ) ) ;
#67790 = DIRECTION ( 'NONE',  ( 0.000000000000000000, 0.000000000000000000, 1.000000000000000000 ) ) ;
#67791 = CARTESIAN_POINT ( 'NONE',  ( -3.750000000000029310, 2.500000000000000000, -7.188010851410854052 ) ) ;
#67792 = ORIENTED_EDGE ( 'NONE', *, *, #64325, .T. ) ;
#67793 = CARTESIAN_POINT ( 'NONE',  ( 16.98389447545005027, -2.500000000000469402, 5.627887033854102938 ) ) ;
#67794 = EDGE_CURVE ( 'NONE', #62518, #36092, #126437, .T. ) ;
#67795 = ORIENTED_EDGE ( 'NONE', *, *, #30509, .T. ) ;
#67796 = AXIS2_PLACEMENT_3D ( 'NONE', #32208, #13163, #73385 ) ;
#67797 = CIRCLE ( 'NONE', #40729, 0.1000000000000002554 ) ;
#67798 = ORIENTED_EDGE ( 'NONE', *, *, #70124, .F. ) ;
#67799 = ORIENTED_EDGE ( 'NONE', *, *, #117975, .F. ) ;
#67800 = CARTESIAN_POINT ( 'NONE',  ( 97.50000000000000000, -1.500000000000000222, 1.322875655532295136 ) ) ;
#67801 = DIRECTION ( 'NONE',  ( 0.000000000000000000, 0.000000000000000000, 1.000000000000000000 ) ) ;
#67803 = AXIS2_PLACEMENT_3D ( 'NONE', #110133, #820, #40777 ) ;
#67802 = DIRECTION ( 'NONE',  ( -0.000000000000000000, 1.000000000000000000, -0.000000000000000000 ) ) ;
#67804 = ORIENTED_EDGE ( 'NONE', *, *, #60532, .T. ) ;
#67805 = DIRECTION ( 'NONE',  ( 0.000000000000000000, 1.000000000000000000, 0.000000000000000000 ) ) ;
#67806 = VECTOR ( 'NONE', #12838, 1000.000000000000000 ) ;
#67807 = DIRECTION ( 'NONE',  ( -0.000000000000000000, -1.000000000000000000, -0.000000000000000000 ) ) ;
#67808 = DIRECTION ( 'NONE',  ( 0.000000000000000000, 0.000000000000000000, 1.000000000000000000 ) ) ;
#67809 = CARTESIAN_POINT ( 'NONE',  ( 186.1927083336747160, 6.551208109652275624, -3.782341765624998686 ) ) ;
#67810 = DIRECTION ( 'NONE',  ( 0.000000000000000000, 1.000000000000000000, 0.000000000000000000 ) ) ;
#67811 = CARTESIAN_POINT ( 'NONE',  ( 7.899999999999924860, 12.50000000000000000, 4.395220292106234439 ) ) ;
#67812 = CARTESIAN_POINT ( 'NONE',  ( -11.64999999999999680, 2.500000000000000000, 1.472243186433545459 ) ) ;
#67813 = ORIENTED_EDGE ( 'NONE', *, *, #11711, .F. ) ;
#67814 = FACE_OUTER_BOUND ( 'NONE', #10892, .T. ) ;
#67815 = ORIENTED_EDGE ( 'NONE', *, *, #18951, .T. ) ;
#67817 = VERTEX_POINT ( 'NONE', #19387 ) ;
#67816 = AXIS2_PLACEMENT_3D ( 'NONE', #13098, #102151, #3937 ) ;
#67818 = DIRECTION ( 'NONE',  ( -0.000000000000000000, -1.000000000000000000, -0.000000000000000000 ) ) ;
#67819 = CONICAL_SURFACE ( 'NONE', #11386, 0.1000000000000002554, 0.003490658503988666988 ) ;
#67820 = DIRECTION ( 'NONE',  ( -0.000000000000000000, 1.000000000000000000, -0.000000000000000000 ) ) ;
#67821 = AXIS2_PLACEMENT_3D ( 'NONE', #60101, #52193, #72489 ) ;
#67822 = CARTESIAN_POINT ( 'NONE',  ( -6.850000000000013856, 12.50000000000000000, 6.148780366869520897 ) ) ;
#67823 = ORIENTED_EDGE ( 'NONE', *, *, #74731, .T. ) ;
#67824 = VERTEX_POINT ( 'NONE', #18105 ) ;
#67825 = ADVANCED_FACE ( 'NONE', ( #36490 ), #68496, .T. ) ;
#67826 = CARTESIAN_POINT ( 'NONE',  ( 184.9895833340161175, -4.445597072760163471, -7.699999999999919353 ) ) ;
#67827 = AXIS2_PLACEMENT_3D ( 'NONE', #120963, #58827, #98733 ) ;
#67828 = AXIS2_PLACEMENT_3D ( 'NONE', #89698, #59624, #97580 ) ;
#67829 = AXIS2_PLACEMENT_3D ( 'NONE', #42923, #82835, #122742 ) ;
#67830 = DIRECTION ( 'NONE',  ( -0.8660254037844390407, 0.000000000000000000, -0.4999999999999991673 ) ) ;
#67831 = CARTESIAN_POINT ( 'NONE',  ( 4.549999999999937650, 2.500000000000000000, 2.165063509461097713 ) ) ;
#67832 = ORIENTED_EDGE ( 'NONE', *, *, #49932, .F. ) ;
#67833 = ORIENTED_EDGE ( 'NONE', *, *, #7992, .F. ) ;
#67834 = CARTESIAN_POINT ( 'NONE',  ( -0.6000000000000323963, 12.50000000000000000, 0.3464101615137759604 ) ) ;
#67835 = EDGE_LOOP ( 'NONE', ( #76124, #100297 ) ) ;
#67836 = DIRECTION ( 'NONE',  ( 0.000000000000000000, 0.000000000000000000, 1.000000000000000000 ) ) ;
#67837 = CIRCLE ( 'NONE', #95041, 0.09999999999999982514 ) ;
#67838 = CONICAL_SURFACE ( 'NONE', #44875, 0.09999999999999999167, 0.003490658503988666988 ) ;
#67839 = FACE_OUTER_BOUND ( 'NONE', #90107, .T. ) ;
#67840 = VERTEX_POINT ( 'NONE', #77667 ) ;
#67841 = DIRECTION ( 'NONE',  ( 0.000000000000000000, 1.000000000000000000, 0.000000000000000000 ) ) ;
#67842 = FACE_OUTER_BOUND ( 'NONE', #59402, .T. ) ;
#67843 = LINE ( 'NONE', #77657, #51121 ) ;
#67844 = AXIS2_PLACEMENT_3D ( 'NONE', #27941, #5708, #67860 ) ;
#67845 = EDGE_CURVE ( 'NONE', #4262, #109253, #72063, .T. ) ;
#67846 = FACE_OUTER_BOUND ( 'NONE', #54725, .T. ) ;
#67847 = ORIENTED_EDGE ( 'NONE', *, *, #114105, .T. ) ;
#67848 = CARTESIAN_POINT ( 'NONE',  ( 8.349999999999923261, 12.50000000000000000, -5.867463478539787225 ) ) ;
#67849 = VERTEX_POINT ( 'NONE', #108421 ) ;
#67850 = ORIENTED_EDGE ( 'NONE', *, *, #14902, .F. ) ;
#67851 = EDGE_CURVE ( 'NONE', #57277, #25898, #5229, .T. ) ;
#67852 = FACE_OUTER_BOUND ( 'NONE', #99655, .T. ) ;
#67853 = LINE ( 'NONE', #69135, #78423 ) ;
#67854 = DIRECTION ( 'NONE',  ( -4.274815082592931898E-19, -0.9999939076577903929, -0.003490651415223739937 ) ) ;
#67855 = DIRECTION ( 'NONE',  ( -0.000000000000000000, -1.000000000000000000, -0.000000000000000000 ) ) ;
#67856 = VECTOR ( 'NONE', #108422, 1000.000000000000000 ) ;
#67857 = DIRECTION ( 'NONE',  ( -4.274815082592931898E-19, -0.9999939076577903929, -0.003490651415223739937 ) ) ;
#67858 = CARTESIAN_POINT ( 'NONE',  ( -4.400000000000025224, 12.50000000000000000, -0.3464101615137783474 ) ) ;
#67859 = DIRECTION ( 'NONE',  ( 0.000000000000000000, 0.000000000000000000, 1.000000000000000000 ) ) ;
#67860 = DIRECTION ( 'NONE',  ( 0.000000000000000000, 0.000000000000000000, -1.000000000000000000 ) ) ;
#67861 = DIRECTION ( 'NONE',  ( 0.000000000000000000, 1.000000000000000000, 0.000000000000000000 ) ) ;
#67863 = CIRCLE ( 'NONE', #61625, 0.06509327318403745899 ) ;
#67862 = CARTESIAN_POINT ( 'NONE',  ( 7.299999999999927880, 2.500000000000000000, 3.983716857408420964 ) ) ;
#67864 = CIRCLE ( 'NONE', #126366, 0.06509327318403745899 ) ;
#67865 = ORIENTED_EDGE ( 'NONE', *, *, #31123, .T. ) ;
#67866 = DIRECTION ( 'NONE',  ( -0.000000000000000000, 1.000000000000000000, -0.000000000000000000 ) ) ;
#67867 = DIRECTION ( 'NONE',  ( 0.000000000000000000, 1.000000000000000000, 0.000000000000000000 ) ) ;
#67868 = DIRECTION ( 'NONE',  ( 0.000000000000000000, 1.000000000000000000, 0.000000000000000000 ) ) ;
#67869 = CARTESIAN_POINT ( 'NONE',  ( -9.150000000000009237, 2.500000000000000000, 2.857883832488649301 ) ) ;
#67870 = FACE_OUTER_BOUND ( 'NONE', #128721, .T. ) ;
#67871 = EDGE_LOOP ( 'NONE', ( #69975, #25693, #91100, #55209 ) ) ;
#67872 = CARTESIAN_POINT ( 'NONE',  ( -0.4500000000000402012, 12.50000000000000000, 6.495190528383297135 ) ) ;
#67873 = AXIS2_PLACEMENT_3D ( 'NONE', #110719, #21050, #60368 ) ;
#67874 = EDGE_CURVE ( 'NONE', #124382, #86648, #117571, .T. ) ;
#67875 = AXIS2_PLACEMENT_3D ( 'NONE', #19658, #108671, #59608 ) ;
#67876 = CARTESIAN_POINT ( 'NONE',  ( -7.499999999999980460, 2.500000000000000000, -4.330127018922201643 ) ) ;
#67878 = ORIENTED_EDGE ( 'NONE', *, *, #104995, .T. ) ;
#67877 = CARTESIAN_POINT ( 'NONE',  ( -1.650000000000035660, 2.500000000000000000, 2.857883832488649301 ) ) ;
#67879 = ADVANCED_FACE ( 'NONE', ( #98585 ), #118894, .T. ) ;
#67880 = EDGE_CURVE ( 'NONE', #64666, #59157, #3101, .T. ) ;
#67881 = ORIENTED_EDGE ( 'NONE', *, *, #127338, .T. ) ;
#67882 = CONICAL_SURFACE ( 'NONE', #69961, 0.09999999999999982514, 0.003490658503988666988 ) ;
#67883 = CIRCLE ( 'NONE', #1081, 0.1000000000000000056 ) ;
#67884 = ORIENTED_EDGE ( 'NONE', *, *, #92005, .T. ) ;
#67885 = ORIENTED_EDGE ( 'NONE', *, *, #86047, .T. ) ;
#67886 = VERTEX_POINT ( 'NONE', #16794 ) ;
#67887 = CARTESIAN_POINT ( 'NONE',  ( 6.249999999999934275, 2.500000000000000000, -7.188010851410854052 ) ) ;
#67888 = EDGE_CURVE ( 'NONE', #86766, #66020, #67853, .T. ) ;
#67889 = EDGE_CURVE ( 'NONE', #25677, #249, #51227, .T. ) ;
#67890 = VECTOR ( 'NONE', #126398, 1000.000000000000000 ) ;
#67891 = EDGE_CURVE ( 'NONE', #111766, #92201, #8920, .T. ) ;
#67892 = CARTESIAN_POINT ( 'NONE',  ( -5.850000000000021849, 2.500000000000000000, -7.288010851410854585 ) ) ;
#67893 = DIRECTION ( 'NONE',  ( 0.000000000000000000, -0.9999939076577903929, 0.003490651415223739937 ) ) ;
#67894 = VECTOR ( 'NONE', #51370, 1000.000000000000000 ) ;
#67895 = DIRECTION ( 'NONE',  ( 0.000000000000000000, 1.000000000000000000, 0.000000000000000000 ) ) ;
#67896 = VERTEX_POINT ( 'NONE', #48220 ) ;
#67897 = ADVANCED_FACE ( 'NONE', ( #128744 ), #128075, .T. ) ;
#67898 = DIRECTION ( 'NONE',  ( 0.000000000000000000, 1.000000000000000000, 0.000000000000000000 ) ) ;
#67899 = ORIENTED_EDGE ( 'NONE', *, *, #49599, .T. ) ;
#67900 = CARTESIAN_POINT ( 'NONE',  ( 26.75237029040465941, -2.962322469584636409, -2.722363819586870015 ) ) ;
#67901 = DIRECTION ( 'NONE',  ( -0.000000000000000000, 1.000000000000000000, -0.000000000000000000 ) ) ;
#67902 = CARTESIAN_POINT ( 'NONE',  ( 21.15177371151419194, 2.593223176056360213, 4.151029080743461108 ) ) ;
#67903 = CARTESIAN_POINT ( 'NONE',  ( -3.150000000000029665, 12.50000000000000000, 6.906693963081109722 ) ) ;
#67904 = DIRECTION ( 'NONE',  ( -4.274815082592931898E-19, -0.9999939076577903929, -0.003490651415223739937 ) ) ;
#67905 = ADVANCED_FACE ( 'NONE', ( #99268 ), #82528, .T. ) ;
#67906 = EDGE_LOOP ( 'NONE', ( #14306, #24949, #17413, #37296 ) ) ;
#67907 = AXIS2_PLACEMENT_3D ( 'NONE', #28752, #120354, #1847 ) ;
#67908 = ORIENTED_EDGE ( 'NONE', *, *, #83749, .F. ) ;
#67909 = ORIENTED_EDGE ( 'NONE', *, *, #32600, .T. ) ;
#67910 = EDGE_LOOP ( 'NONE', ( #45819, #116471, #24775, #101683 ) ) ;
#67911 = DIRECTION ( 'NONE',  ( -0.000000000000000000, 1.000000000000000000, -0.000000000000000000 ) ) ;
#67912 = CARTESIAN_POINT ( 'NONE',  ( 26.76176526818647972, 1.073658814953058815, 4.445806700279154811 ) ) ;
#67913 = CONICAL_SURFACE ( 'NONE', #42821, 0.1000000000000002554, 0.003490658503988666988 ) ;
#67914 = FACE_OUTER_BOUND ( 'NONE', #56379, .T. ) ;
#67915 = FACE_BOUND ( 'NONE', #35488, .T. ) ;
#67916 = DIRECTION ( 'NONE',  ( -4.274815082592931898E-19, -0.9999939076577903929, -0.003490651415223739937 ) ) ;
#67917 = CARTESIAN_POINT ( 'NONE',  ( 187.2812500006828031, 0.000000000000000000, 7.700000000000000178 ) ) ;
#67918 = FACE_OUTER_BOUND ( 'NONE', #54282, .T. ) ;
#67919 = LINE ( 'NONE', #37820, #64676 ) ;
#67920 = AXIS2_PLACEMENT_3D ( 'NONE', #6315, #75089, #35808 ) ;
#67921 = CIRCLE ( 'NONE', #103439, 0.06509327318403745899 ) ;
#67922 = AXIS2_PLACEMENT_3D ( 'NONE', #38241, #127265, #67675 ) ;
#67923 = CARTESIAN_POINT ( 'NONE',  ( 184.1718750003414016, 9.264065473108010111E-16, -7.564683531250000925 ) ) ;
#67924 = DIRECTION ( 'NONE',  ( 0.000000000000000000, 0.000000000000000000, 1.000000000000000000 ) ) ;
#67925 = CARTESIAN_POINT ( 'NONE',  ( -2.900000000000029221, 2.500000000000000000, -0.6928203230275541413 ) ) ;
#67926 = VECTOR ( 'NONE', #48883, 1000.000000000000000 ) ;
#67927 = AXIS2_PLACEMENT_3D ( 'NONE', #104962, #105637, #15291 ) ;
#67928 = CARTESIAN_POINT ( 'NONE',  ( -5.000000000000023093, 12.50000000000000000, 0.6928203230275494784 ) ) ;
#67929 = ORIENTED_EDGE ( 'NONE', *, *, #82226, .F. ) ;
#67930 = ORIENTED_EDGE ( 'NONE', *, *, #63600, .T. ) ;
#67931 = ORIENTED_EDGE ( 'NONE', *, *, #110324, .F. ) ;
#67932 = ORIENTED_EDGE ( 'NONE', *, *, #45561, .F. ) ;
#67933 = VECTOR ( 'NONE', #12157, 1000.000000000000000 ) ;
#67934 = DIRECTION ( 'NONE',  ( 0.000000000000000000, 0.000000000000000000, 1.000000000000000000 ) ) ;
#67935 = FACE_BOUND ( 'NONE', #46479, .T. ) ;
#67936 = DIRECTION ( 'NONE',  ( -4.274815082592931898E-19, -0.9999939076577903929, -0.003490651415223739937 ) ) ;
#67937 = ADVANCED_FACE ( 'NONE', ( #86185 ), #7636, .T. ) ;
#67938 = ORIENTED_EDGE ( 'NONE', *, *, #87929, .T. ) ;
#67939 = FACE_OUTER_BOUND ( 'NONE', #95648, .T. ) ;
#67940 = CARTESIAN_POINT ( 'NONE',  ( 12.29999999999990479, 2.500000000000000000, 4.676537180435972552 ) ) ;
#67941 = DIRECTION ( 'NONE',  ( 0.000000000000000000, -0.000000000000000000, 1.000000000000000000 ) ) ;
#67943 = ORIENTED_EDGE ( 'NONE', *, *, #25325, .F. ) ;
#67942 = AXIS2_PLACEMENT_3D ( 'NONE', #70855, #10614, #69553 ) ;
#67944 = LINE ( 'NONE', #127522, #97181 ) ;
#67945 = DIRECTION ( 'NONE',  ( 0.000000000000000000, -0.9999939076577903929, 0.003490651415223739937 ) ) ;
#67946 = ADVANCED_FACE ( 'NONE', ( #37123 ), #32373, .T. ) ;
#67947 = ORIENTED_EDGE ( 'NONE', *, *, #125058, .F. ) ;
#67948 = ORIENTED_EDGE ( 'NONE', *, *, #83399, .T. ) ;
#67949 = DIRECTION ( 'NONE',  ( 0.000000000000000000, 0.000000000000000000, 1.000000000000000000 ) ) ;
#67950 = FACE_OUTER_BOUND ( 'NONE', #20467, .T. ) ;
#67951 = AXIS2_PLACEMENT_3D ( 'NONE', #112885, #62510, #103715 ) ;
#67952 = CIRCLE ( 'NONE', #38752, 0.1000000000000002554 ) ;
#67953 = DIRECTION ( 'NONE',  ( 0.000000000000000000, 1.000000000000000000, 0.000000000000000000 ) ) ;
#67954 = FACE_OUTER_BOUND ( 'NONE', #105976, .T. ) ;
#67955 = EDGE_LOOP ( 'NONE', ( #41195, #62515 ) ) ;
#67956 = DIRECTION ( 'NONE',  ( 0.000000000000000000, 1.000000000000000000, 0.000000000000000000 ) ) ;
#67957 = VERTEX_POINT ( 'NONE', #97322 ) ;
#67958 = VERTEX_POINT ( 'NONE', #101835 ) ;
#67959 = DIRECTION ( 'NONE',  ( 0.000000000000000000, 1.000000000000000000, 0.000000000000000000 ) ) ;
#67960 = EDGE_LOOP ( 'NONE', ( #120187, #15684, #25491, #73988 ) ) ;
#67961 = DIRECTION ( 'NONE',  ( 0.000000000000000000, 0.000000000000000000, 1.000000000000000000 ) ) ;
#67962 = FACE_BOUND ( 'NONE', #101614, .T. ) ;
#67963 = EDGE_LOOP ( 'NONE', ( #90005, #118524 ) ) ;
#67964 = CARTESIAN_POINT ( 'NONE',  ( 112.7330628718930967, 7.528728208595681259, 1.645054351054255237 ) ) ;
#67965 = ORIENTED_EDGE ( 'NONE', *, *, #15132, .T. ) ;
#67966 = DIRECTION ( 'NONE',  ( -0.000000000000000000, 1.000000000000000000, -0.000000000000000000 ) ) ;
#67967 = CARTESIAN_POINT ( 'NONE',  ( 10.84999999999991260, 2.500000000000000000, 6.495190528383297135 ) ) ;
#67968 = DIRECTION ( 'NONE',  ( -0.000000000000000000, -1.000000000000000000, -0.000000000000000000 ) ) ;
#67969 = CARTESIAN_POINT ( 'NONE',  ( 0.8499999999999553468, 2.500000000000000000, -2.857883832488653741 ) ) ;
#67970 = PLANE ( 'NONE',  #70435 ) ;
#67971 = ORIENTED_EDGE ( 'NONE', *, *, #100537, .F. ) ;
#67972 = EDGE_LOOP ( 'NONE', ( #110188, #99078, #38309, #124812 ) ) ;
#67974 = ORIENTED_EDGE ( 'NONE', *, *, #44800, .F. ) ;
#67973 = EDGE_CURVE ( 'NONE', #128034, #70146, #49083, .T. ) ;
#67975 = CARTESIAN_POINT ( 'NONE',  ( -6.250000000000017764, 2.500000000000000000, 7.288010851410849256 ) ) ;
#67976 = VECTOR ( 'NONE', #108332, 1000.000000000000000 ) ;
#67977 = AXIS2_PLACEMENT_3D ( 'NONE', #59120, #67623, #68923 ) ;
#67978 = DIRECTION ( 'NONE',  ( 0.000000000000000000, 0.000000000000000000, -1.000000000000000000 ) ) ;
#67979 = DIRECTION ( 'NONE',  ( 0.000000000000000000, -0.000000000000000000, 1.000000000000000000 ) ) ;
#67981 = ORIENTED_EDGE ( 'NONE', *, *, #125950, .F. ) ;
#67980 = VERTEX_POINT ( 'NONE', #71082 ) ;
#67982 = ORIENTED_EDGE ( 'NONE', *, *, #27899, .T. ) ;
#67983 = DIRECTION ( 'NONE',  ( 0.000000000000000000, -0.000000000000000000, 1.000000000000000000 ) ) ;
#67985 = EDGE_CURVE ( 'NONE', #115300, #129059, #90062, .T. ) ;
#67984 = DIRECTION ( 'NONE',  ( -4.274815082592931898E-19, -0.9999939076577903929, -0.003490651415223739937 ) ) ;
#67986 = SHAPE_DEFINITION_REPRESENTATION ( #37649, #71195 ) ;
#67987 = DIRECTION ( 'NONE',  ( 0.000000000000000000, 0.000000000000000000, 1.000000000000000000 ) ) ;
#67988 = DIRECTION ( 'NONE',  ( 0.000000000000000000, 0.000000000000000000, 1.000000000000000000 ) ) ;
#67989 = AXIS2_PLACEMENT_3D ( 'NONE', #4360, #5019, #124162 ) ;
#67990 = CARTESIAN_POINT ( 'NONE',  ( 2.699999999999945555, 12.50000000000000000, 3.918623584224382839 ) ) ;
#67991 = CARTESIAN_POINT ( 'NONE',  ( 8.549999999999918998, 12.50000000000000000, -1.818653347947326138 ) ) ;
#67992 = CARTESIAN_POINT ( 'NONE',  ( -12.69999999999999396, 2.500000000000000000, -3.983716857408423628 ) ) ;
#67993 = EDGE_CURVE ( 'NONE', #101949, #356, #61273, .T. ) ;
#67994 = EDGE_CURVE ( 'NONE', #30373, #55743, #69794, .T. ) ;
#67995 = AXIS2_PLACEMENT_3D ( 'NONE', #34702, #115808, #64771 ) ;
#67996 = CARTESIAN_POINT ( 'NONE',  ( 15.59999999999988951, 2.500000000000000000, -0.4464101615137783252 ) ) ;
#67997 = VERTEX_POINT ( 'NONE', #50805 ) ;
#67998 = ORIENTED_EDGE ( 'NONE', *, *, #126846, .T. ) ;
#67999 = DIRECTION ( 'NONE',  ( -4.274815082592931898E-19, -0.9999939076577903929, -0.003490651415223739937 ) ) ;
#68000 = CIRCLE ( 'NONE', #126502, 0.06509327318403745899 ) ;
#68001 = EDGE_CURVE ( 'NONE', #48532, #67328, #88960, .T. ) ;
#68002 = AXIS2_PLACEMENT_3D ( 'NONE', #84776, #85414, #64483 ) ;
#68003 = FACE_OUTER_BOUND ( 'NONE', #113600, .T. ) ;
#68004 = AXIS2_PLACEMENT_3D ( 'NONE', #63645, #13876, #112095 ) ;
#68005 = ORIENTED_EDGE ( 'NONE', *, *, #10699, .F. ) ;
#68006 = VERTEX_POINT ( 'NONE', #72391 ) ;
#68007 = ADVANCED_FACE ( 'NONE', ( #2319 ), #30399, .T. ) ;
#68008 = CARTESIAN_POINT ( 'NONE',  ( 187.0677083336747444, -4.367472073101514418, -7.564683531250002702 ) ) ;
#68009 = CARTESIAN_POINT ( 'NONE',  ( -6.081641213347104214E-15, 12.50000000000000000, -4.395220292106239768 ) ) ;
#68010 = DIRECTION ( 'NONE',  ( 0.000000000000000000, 0.000000000000000000, -1.000000000000000000 ) ) ;
#68011 = CIRCLE ( 'NONE', #59724, 0.06509327318403745899 ) ;
#68012 = FACE_OUTER_BOUND ( 'NONE', #27687, .T. ) ;
#68013 = CONICAL_SURFACE ( 'NONE', #128691, 0.1000000000000002554, 0.003490658503988666988 ) ;
#68015 = FACE_OUTER_BOUND ( 'NONE', #98514, .T. ) ;
#68014 = CONICAL_SURFACE ( 'NONE', #86790, 0.1000000000000002554, 0.003490658503988666988 ) ;
#68016 = DIRECTION ( 'NONE',  ( 0.000000000000000000, 0.000000000000000000, 1.000000000000000000 ) ) ;
#68017 = DIRECTION ( 'NONE',  ( 0.000000000000000000, 0.000000000000000000, 1.000000000000000000 ) ) ;
#68018 = ORIENTED_EDGE ( 'NONE', *, *, #66742, .T. ) ;
#68019 = CARTESIAN_POINT ( 'NONE',  ( -8.550000000000013145, 2.500000000000000000, 2.411473670974873862 ) ) ;
#68020 = CARTESIAN_POINT ( 'NONE',  ( 3.749999999999978684, 2.500000000000000000, -2.065063509461102065 ) ) ;
#68021 = CIRCLE ( 'NONE', #103536, 0.06509327318403745899 ) ;
#68022 = VECTOR ( 'NONE', #109498, 1000.000000000000000 ) ;
#68023 = ORIENTED_EDGE ( 'NONE', *, *, #40367, .T. ) ;
#68024 = VECTOR ( 'NONE', #30991, 1000.000000000000000 ) ;
#68025 = ORIENTED_EDGE ( 'NONE', *, *, #109262, .T. ) ;
#68026 = EDGE_LOOP ( 'NONE', ( #77839, #59922, #79933, #116077 ) ) ;
#68027 = ORIENTED_EDGE ( 'NONE', *, *, #101293, .T. ) ;
#68028 = CARTESIAN_POINT ( 'NONE',  ( 11.24999999999990763, 2.500000000000000000, 1.472243186433545459 ) ) ;
#68029 = LINE ( 'NONE', #39883, #75112 ) ;
#68030 = ORIENTED_EDGE ( 'NONE', *, *, #43262, .F. ) ;
#68031 = CARTESIAN_POINT ( 'NONE',  ( 11.64999999999990798, 2.500000000000000000, -1.472243186433550122 ) ) ;
#68032 = EDGE_CURVE ( 'NONE', #99852, #35495, #11584, .T. ) ;
#68033 = CARTESIAN_POINT ( 'NONE',  ( 6.249999999999965361, 2.500000000000000000, 2.065063509461097624 ) ) ;
#68034 = DIRECTION ( 'NONE',  ( 0.000000000000000000, 1.000000000000000000, 0.000000000000000000 ) ) ;
#68036 = ORIENTED_EDGE ( 'NONE', *, *, #704, .F. ) ;
#68035 = DIRECTION ( 'NONE',  ( 0.000000000000000000, 0.000000000000000000, -1.000000000000000000 ) ) ;
#68037 = DIRECTION ( 'NONE',  ( -0.000000000000000000, 1.000000000000000000, -0.000000000000000000 ) ) ;
#68038 = CIRCLE ( 'NONE', #111972, 0.1000000000000002554 ) ;
#68039 = ADVANCED_FACE ( 'NONE', ( #121457 ), #76350, .T. ) ;
#68040 = FACE_OUTER_BOUND ( 'NONE', #129189, .T. ) ;
#68041 = VERTEX_POINT ( 'NONE', #110358 ) ;
#68042 = EDGE_LOOP ( 'NONE', ( #23158, #104257 ) ) ;
#68043 = ORIENTED_EDGE ( 'NONE', *, *, #128758, .F. ) ;
#68044 = CARTESIAN_POINT ( 'NONE',  ( 7.699999999999925571, 2.500000000000000000, -4.676537180435978769 ) ) ;
#68045 = ADVANCED_FACE ( 'NONE', ( #51461 ), #51324, .T. ) ;
#68046 = ADVANCED_FACE ( 'NONE', ( #12148 ), #42277, .T. ) ;
#68047 = CIRCLE ( 'NONE', #11615, 0.06509327318403745899 ) ;
#68048 = EDGE_CURVE ( 'NONE', #26341, #31641, #31813, .T. ) ;
#68049 = CARTESIAN_POINT ( 'NONE',  ( -10.00000000000000533, 2.500000000000000000, 0.7928203230275495672 ) ) ;
#68050 = AXIS2_PLACEMENT_3D ( 'NONE', #120107, #48794, #108966 ) ;
#68051 = ADVANCED_FACE ( 'NONE', ( #82198 ), #40866, .T. ) ;
#68052 = ORIENTED_EDGE ( 'NONE', *, *, #99226, .F. ) ;
#68053 = LINE ( 'NONE', #107979, #49527 ) ;
#68054 = CARTESIAN_POINT ( 'NONE',  ( 8.349999999999919709, 12.50000000000000000, 5.867463478539781896 ) ) ;
#68055 = DIRECTION ( 'NONE',  ( 0.000000000000000000, 1.000000000000000000, 0.000000000000000000 ) ) ;
#68056 = CARTESIAN_POINT ( 'NONE',  ( 9.399999999999918643, 12.50000000000000000, -0.4115034346978156399 ) ) ;
#68057 = EDGE_CURVE ( 'NONE', #129352, #25026, #113999, .T. ) ;
#68058 = VERTEX_POINT ( 'NONE', #99906 ) ;
#68059 = ADVANCED_FACE ( 'NONE', ( #22006 ), #34601, .T. ) ;
#68060 = CARTESIAN_POINT ( 'NONE',  ( 179.5000000000000000, -1.375000000000000000, 7.576237522675751457 ) ) ;
#68061 = CONICAL_SURFACE ( 'NONE', #78554, 0.1000000000000002554, 0.003490658503988666988 ) ;
#68062 = VERTEX_POINT ( 'NONE', #62570 ) ;
#68063 = ORIENTED_EDGE ( 'NONE', *, *, #120671, .F. ) ;
#68064 = CARTESIAN_POINT ( 'NONE',  ( -10.00000000000000355, 12.50000000000000000, -0.6277270498435166823 ) ) ;
#68065 = DIRECTION ( 'NONE',  ( 0.000000000000000000, 1.000000000000000000, 0.000000000000000000 ) ) ;
#68066 = FACE_BOUND ( 'NONE', #28823, .T. ) ;
#68067 = CARTESIAN_POINT ( 'NONE',  ( -10.65000000000000213, 2.500000000000000000, 6.941600689897073018 ) ) ;
#68068 = CARTESIAN_POINT ( 'NONE',  ( 0.5999999999999560130, 12.50000000000000000, -4.048810130592463530 ) ) ;
#68069 = CARTESIAN_POINT ( 'NONE',  ( 129.5000000000000000, 0.000000000000000000, 0.000000000000000000 ) ) ;
#68070 = CIRCLE ( 'NONE', #72296, 0.06509327318403745899 ) ;
#68071 = VECTOR ( 'NONE', #121896, 1000.000000000000000 ) ;
#68072 = ORIENTED_EDGE ( 'NONE', *, *, #69034, .F. ) ;
#68073 = CARTESIAN_POINT ( 'NONE',  ( 1.899999999999951283, 2.500000000000000000, -4.776537180435977525 ) ) ;
#68074 = CARTESIAN_POINT ( 'NONE',  ( 10.84999999999990905, 2.500000000000000000, -7.088010851410853519 ) ) ;
#68075 = CARTESIAN_POINT ( 'NONE',  ( -0.4500000000000402012, 2.500000000000000000, 2.165063509461097713 ) ) ;
#68076 = DIRECTION ( 'NONE',  ( 1.000000000000000000, 0.000000000000000000, -0.000000000000000000 ) ) ;
#68077 = ORIENTED_EDGE ( 'NONE', *, *, #31590, .T. ) ;
#68078 = DIRECTION ( 'NONE',  ( 0.000000000000000000, 1.000000000000000000, 0.000000000000000000 ) ) ;
#68079 = FACE_OUTER_BOUND ( 'NONE', #9251, .T. ) ;
#68080 = ORIENTED_EDGE ( 'NONE', *, *, #3599, .T. ) ;
#68081 = VERTEX_POINT ( 'NONE', #9587 ) ;
#68082 = DIRECTION ( 'NONE',  ( 0.000000000000000000, 0.000000000000000000, 1.000000000000000000 ) ) ;
#68083 = PLANE ( 'NONE',  #425 ) ;
#68084 = FACE_BOUND ( 'NONE', #86327, .T. ) ;
#68085 = DIRECTION ( 'NONE',  ( 0.000000000000000000, 1.000000000000000000, 0.000000000000000000 ) ) ;
#68086 = AXIS2_PLACEMENT_3D ( 'NONE', #121261, #11298, #110154 ) ;
#68087 = VERTEX_POINT ( 'NONE', #109725 ) ;
#68088 = CARTESIAN_POINT ( 'NONE',  ( -1.850000000000033396, 2.500000000000000000, -1.718653347947325827 ) ) ;
#68089 = AXIS2_PLACEMENT_3D ( 'NONE', #124554, #104883, #105555 ) ;
#68090 = ORIENTED_EDGE ( 'NONE', *, *, #70911, .T. ) ;
#68091 = ORIENTED_EDGE ( 'NONE', *, *, #114881, .F. ) ;
#68092 = FACE_OUTER_BOUND ( 'NONE', #61251, .T. ) ;
#68093 = CARTESIAN_POINT ( 'NONE',  ( 184.4635416670080588, -4.367472073101519747, 7.564683531249999149 ) ) ;
#68094 = ORIENTED_EDGE ( 'NONE', *, *, #83463, .T. ) ;
#68095 = FACE_OUTER_BOUND ( 'NONE', #86582, .T. ) ;
#68096 = CARTESIAN_POINT ( 'NONE',  ( -8.150000000000009237, 12.50000000000000000, 6.841600689897072485 ) ) ;
#68097 = ADVANCED_FACE ( 'NONE', ( #39722 ), #15683, .T. ) ;
#68098 = AXIS2_PLACEMENT_3D ( 'NONE', #108294, #51340, #59879 ) ;
#68099 = DIRECTION ( 'NONE',  ( -0.000000000000000000, -1.000000000000000000, -0.000000000000000000 ) ) ;
#68100 = CARTESIAN_POINT ( 'NONE',  ( 12.69999999999990159, 2.500000000000000000, -3.883716857408426648 ) ) ;
#68101 = AXIS2_PLACEMENT_3D ( 'NONE', #59193, #60489, #100395 ) ;
#68102 = CONICAL_SURFACE ( 'NONE', #78318, 0.1000000000000002554, 0.003490658503988666988 ) ;
#68103 = ORIENTED_EDGE ( 'NONE', *, *, #74468, .F. ) ;
#68104 = CONICAL_SURFACE ( 'NONE', #70279, 0.09999999999999999167, 0.003490658503988666988 ) ;
#68105 = DIRECTION ( 'NONE',  ( -0.000000000000000000, 1.000000000000000000, -0.000000000000000000 ) ) ;
#68106 = LINE ( 'NONE', #106107, #28883 ) ;
#68107 = CARTESIAN_POINT ( 'NONE',  ( 8.149999999999923972, 2.500000000000000000, 1.918653347947321564 ) ) ;
#68108 = CIRCLE ( 'NONE', #78324, 0.09999999999999982514 ) ;
#68109 = CARTESIAN_POINT ( 'NONE',  ( 6.849999999999929479, 2.500000000000000000, -1.918653347947326004 ) ) ;
#68110 = ORIENTED_EDGE ( 'NONE', *, *, #123424, .F. ) ;
#68111 = DIRECTION ( 'NONE',  ( 0.000000000000000000, 1.000000000000000000, 0.000000000000000000 ) ) ;
#68112 = ORIENTED_EDGE ( 'NONE', *, *, #68730, .F. ) ;
#68113 = CARTESIAN_POINT ( 'NONE',  ( 16.88398462908685005, 2.500000000000000000, 4.430583899588694585 ) ) ;
#68114 = ORIENTED_EDGE ( 'NONE', *, *, #123517, .F. ) ;
#68115 = DIRECTION ( 'NONE',  ( 0.000000000000000000, 1.000000000000000000, 0.000000000000000000 ) ) ;
#68116 = DIRECTION ( 'NONE',  ( 0.000000000000000000, 1.000000000000000000, -1.846105847067148761E-16 ) ) ;
#68117 = DIRECTION ( 'NONE',  ( 0.000000000000000000, 0.000000000000000000, -1.000000000000000000 ) ) ;
#68118 = CARTESIAN_POINT ( 'NONE',  ( -8.350000000000010303, 2.500000000000000000, 6.595190528383296780 ) ) ;
#68119 = EDGE_LOOP ( 'NONE', ( #21716, #125209, #122583, #18746 ) ) ;
#68120 = CARTESIAN_POINT ( 'NONE',  ( 10.59999999999990905, 2.500000000000000000, 4.576537180435972019 ) ) ;
#68121 = DIRECTION ( 'NONE',  ( 0.000000000000000000, 1.000000000000000000, 0.000000000000000000 ) ) ;
#68122 = FACE_OUTER_BOUND ( 'NONE', #53156, .T. ) ;
#68123 = CARTESIAN_POINT ( 'NONE',  ( 185.0260416670080588, -6.551208109652273848, -3.782341765625003571 ) ) ;
#68124 = DIRECTION ( 'NONE',  ( -4.274815082592931898E-19, -0.9999939076577903929, -0.003490651415223739937 ) ) ;
#68125 = CARTESIAN_POINT ( 'NONE',  ( -13.09999999999999076, 12.50000000000000000, 4.676537180435972552 ) ) ;
#68126 = VERTEX_POINT ( 'NONE', #80267 ) ;
#68127 = ORIENTED_EDGE ( 'NONE', *, *, #66364, .F. ) ;
#68128 = PLANE ( 'NONE',  #116355 ) ;
#68129 = VERTEX_POINT ( 'NONE', #10845 ) ;
#68130 = DIRECTION ( 'NONE',  ( 0.000000000000000000, -0.9999939076577903929, 0.003490651415223739937 ) ) ;
#68132 = EDGE_LOOP ( 'NONE', ( #85354, #113545 ) ) ;
#68131 = ORIENTED_EDGE ( 'NONE', *, *, #62762, .T. ) ;
#68133 = AXIS2_PLACEMENT_3D ( 'NONE', #73273, #54916, #3254 ) ;
#68134 = ORIENTED_EDGE ( 'NONE', *, *, #43972, .F. ) ;
#68135 = DIRECTION ( 'NONE',  ( 0.000000000000000000, 0.000000000000000000, 1.000000000000000000 ) ) ;
#68136 = VECTOR ( 'NONE', #122523, 1000.000000000000000 ) ;
#68137 = CIRCLE ( 'NONE', #11708, 0.06509327318403745899 ) ;
#68139 = EDGE_CURVE ( 'NONE', #115197, #114185, #120266, .T. ) ;
#68138 = DIRECTION ( 'NONE',  ( -0.000000000000000000, 1.000000000000000000, -0.000000000000000000 ) ) ;
#68140 = CARTESIAN_POINT ( 'NONE',  ( -13.09999999999999076, 2.500000000000000000, 3.883716857408421319 ) ) ;
#68141 = AXIS2_PLACEMENT_3D ( 'NONE', #29467, #119773, #71308 ) ;
#68142 = DIRECTION ( 'NONE',  ( 0.000000000000000000, 0.000000000000000000, -1.000000000000000000 ) ) ;
#68143 = LINE ( 'NONE', #99564, #73134 ) ;
#68144 = DIRECTION ( 'NONE',  ( 0.000000000000000000, 0.000000000000000000, 1.000000000000000000 ) ) ;
#68145 = PLANE ( 'NONE',  #42432 ) ;
#68146 = EDGE_CURVE ( 'NONE', #83529, #23572, #38815, .T. ) ;
#68147 = EDGE_CURVE ( 'NONE', #115955, #74459, #101484, .T. ) ;
#68148 = FACE_OUTER_BOUND ( 'NONE', #97190, .T. ) ;
#68149 = ORIENTED_EDGE ( 'NONE', *, *, #34383, .T. ) ;
#68150 = AXIS2_PLACEMENT_3D ( 'NONE', #47006, #47646, #37188 ) ;
#68151 = ORIENTED_EDGE ( 'NONE', *, *, #18915, .T. ) ;
#68152 = ORIENTED_EDGE ( 'NONE', *, *, #39967, .T. ) ;
#68154 = AXIS2_PLACEMENT_3D ( 'NONE', #112730, #72804, #42720 ) ;
#68153 = VECTOR ( 'NONE', #42573, 1000.000000000000000 ) ;
#68155 = EDGE_CURVE ( 'NONE', #10727, #12562, #32464, .T. ) ;
#68157 = ADVANCED_FACE ( 'NONE', ( #75581 ), #105598, .T. ) ;
#68156 = FACE_OUTER_BOUND ( 'NONE', #110532, .T. ) ;
#68159 = EDGE_LOOP ( 'NONE', ( #102194, #35022, #77798, #119520 ) ) ;
#68158 = EDGE_CURVE ( 'NONE', #86861, #101388, #19919, .T. ) ;
#68160 = ORIENTED_EDGE ( 'NONE', *, *, #128961, .T. ) ;
#68161 = EDGE_CURVE ( 'NONE', #6400, #38652, #68021, .T. ) ;
#68162 = DIRECTION ( 'NONE',  ( 0.000000000000000000, 1.000000000000000000, 0.000000000000000000 ) ) ;
#68163 = DIRECTION ( 'NONE',  ( -4.274815082592931898E-19, -0.9999939076577903929, -0.003490651415223739937 ) ) ;
#68164 = DIRECTION ( 'NONE',  ( 0.000000000000000000, 0.000000000000000000, -1.000000000000000000 ) ) ;
#68165 = DIRECTION ( 'NONE',  ( 0.000000000000000000, 0.000000000000000000, 1.000000000000000000 ) ) ;
#68166 = CARTESIAN_POINT ( 'NONE',  ( 1.649999999999951950, 2.500000000000000000, -7.188010851410854052 ) ) ;
#68167 = ORIENTED_EDGE ( 'NONE', *, *, #10129, .F. ) ;
#68168 = CARTESIAN_POINT ( 'NONE',  ( -7.100000000000014744, 12.50000000000000000, 4.330127018922196314 ) ) ;
#68169 = EDGE_LOOP ( 'NONE', ( #116841, #28134, #122762, #125414 ) ) ;
#68170 = CARTESIAN_POINT ( 'NONE',  ( 12.89999999999990088, 2.500000000000000000, -4.230127018922201998 ) ) ;
#68171 = ORIENTED_EDGE ( 'NONE', *, *, #104429, .T. ) ;
#68172 = DIRECTION ( 'NONE',  ( -0.000000000000000000, -1.000000000000000000, -0.000000000000000000 ) ) ;
#68173 = ORIENTED_EDGE ( 'NONE', *, *, #79429, .T. ) ;
#68174 = ORIENTED_EDGE ( 'NONE', *, *, #86649, .T. ) ;
#68175 = CARTESIAN_POINT ( 'NONE',  ( -15.19999999999998153, 2.500000000000000000, -0.4464101615137759382 ) ) ;
#68176 = DIRECTION ( 'NONE',  ( 0.000000000000000000, 0.000000000000000000, 1.000000000000000000 ) ) ;
#68177 = CONICAL_SURFACE ( 'NONE', #126683, 0.1000000000000002554, 0.003490658503988666988 ) ;
#68178 = FACE_OUTER_BOUND ( 'NONE', #32880, .T. ) ;
#68180 = DIRECTION ( 'NONE',  ( -0.000000000000000000, -1.000000000000000000, -0.000000000000000000 ) ) ;
#68179 = AXIS2_PLACEMENT_3D ( 'NONE', #10548, #50489, #90396 ) ;
#68181 = DIRECTION ( 'NONE',  ( 0.000000000000000000, -0.000000000000000000, 1.000000000000000000 ) ) ;
#68182 = ORIENTED_EDGE ( 'NONE', *, *, #114864, .T. ) ;
#68183 = DIRECTION ( 'NONE',  ( -4.274815082592931898E-19, -0.9999939076577903929, -0.003490651415223739937 ) ) ;
#68184 = DIRECTION ( 'NONE',  ( -1.000000000000000000, -0.000000000000000000, -0.000000000000000000 ) ) ;
#68185 = ADVANCED_FACE ( 'NONE', ( #74314 ), #114234, .T. ) ;
#68186 = DIRECTION ( 'NONE',  ( -4.274815082592931898E-19, -0.9999939076577903929, -0.003490651415223739937 ) ) ;
#68187 = DIRECTION ( 'NONE',  ( 0.000000000000000000, -0.9999939076577903929, 0.003490651415223739937 ) ) ;
#68189 = CIRCLE ( 'NONE', #20087, 0.06509327318403745899 ) ;
#68188 = CIRCLE ( 'NONE', #20372, 0.06509327318403745899 ) ;
#68190 = CARTESIAN_POINT ( 'NONE',  ( 5.399999999999934630, 2.500000000000000000, 0.7928203230275495672 ) ) ;
#68191 = ORIENTED_EDGE ( 'NONE', *, *, #23892, .F. ) ;
#68192 = ORIENTED_EDGE ( 'NONE', *, *, #87597, .F. ) ;
#68193 = EDGE_CURVE ( 'NONE', #102955, #118684, #109796, .T. ) ;
#68194 = DIRECTION ( 'NONE',  ( 0.000000000000000000, 0.000000000000000000, -1.000000000000000000 ) ) ;
#68195 = EDGE_CURVE ( 'NONE', #34456, #40951, #5312, .T. ) ;
#68196 = EDGE_CURVE ( 'NONE', #62111, #46500, #45057, .T. ) ;
#68197 = ORIENTED_EDGE ( 'NONE', *, *, #54661, .T. ) ;
#68198 = CIRCLE ( 'NONE', #118377, 0.06509327318403745899 ) ;
#68199 = FACE_OUTER_BOUND ( 'NONE', #58994, .T. ) ;
#68200 = CARTESIAN_POINT ( 'NONE',  ( 4.199999999999941558, 2.500000000000000000, -4.330127018922201643 ) ) ;
#68201 = AXIS2_PLACEMENT_3D ( 'NONE', #56865, #18248, #105349 ) ;
#68202 = EDGE_CURVE ( 'NONE', #74641, #17512, #3197, .T. ) ;
#68203 = ORIENTED_EDGE ( 'NONE', *, *, #56485, .T. ) ;
#68204 = CARTESIAN_POINT ( 'NONE',  ( 184.7500000000000000, 9.429780353434619030E-16, -7.700000000000000178 ) ) ;
#68205 = CARTESIAN_POINT ( 'NONE',  ( -10.20000000000000284, 12.50000000000000000, -0.4115034346978156399 ) ) ;
#68206 = EDGE_CURVE ( 'NONE', #17430, #109569, #95223, .T. ) ;
#68207 = DIRECTION ( 'NONE',  ( -4.274815082592931898E-19, -0.9999939076577903929, -0.003490651415223739937 ) ) ;
#68208 = CARTESIAN_POINT ( 'NONE',  ( -14.14999999999998614, 12.50000000000000000, -2.099970236277062252 ) ) ;
#68209 = ORIENTED_EDGE ( 'NONE', *, *, #4075, .F. ) ;
#68210 = EDGE_CURVE ( 'NONE', #101786, #49149, #82613, .T. ) ;
#68211 = EDGE_CURVE ( 'NONE', #129348, #35861, #99335, .T. ) ;
#68212 = EDGE_CURVE ( 'NONE', #114052, #37015, #36656, .T. ) ;
#68213 = CARTESIAN_POINT ( 'NONE',  ( 4.799999999999937650, 12.50000000000000000, -3.983716857408426293 ) ) ;
#68214 = ORIENTED_EDGE ( 'NONE', *, *, #40890, .F. ) ;
#68215 = PLANE ( 'NONE',  #96596 ) ;
#68216 = AXIS2_PLACEMENT_3D ( 'NONE', #103232, #41751, #121564 ) ;
#68217 = DIRECTION ( 'NONE',  ( 0.000000000000000000, -0.9999939076577903929, 0.003490651415223739937 ) ) ;
#68218 = ADVANCED_FACE ( 'NONE', ( #54647 ), #114861, .T. ) ;
#68219 = FACE_OUTER_BOUND ( 'NONE', #61270, .T. ) ;
#68220 = EDGE_LOOP ( 'NONE', ( #96790, #91935 ) ) ;
#68221 = CIRCLE ( 'NONE', #55702, 0.06509327318403745899 ) ;
#68222 = VECTOR ( 'NONE', #15347, 1000.000000000000000 ) ;
#68223 = LINE ( 'NONE', #25722, #67729 ) ;
#68224 = AXIS2_PLACEMENT_3D ( 'NONE', #77769, #128188, #107887 ) ;
#68225 = VERTEX_POINT ( 'NONE', #23256 ) ;
#68226 = LINE ( 'NONE', #9313, #62597 ) ;
#68227 = CARTESIAN_POINT ( 'NONE',  ( -3.550000000000027356, 2.500000000000000000, -2.511473670974877948 ) ) ;
#68228 = AXIS2_PLACEMENT_3D ( 'NONE', #114620, #24959, #125716 ) ;
#68229 = DIRECTION ( 'NONE',  ( 0.000000000000000000, 0.000000000000000000, 1.000000000000000000 ) ) ;
#68230 = VECTOR ( 'NONE', #102244, 1000.000000000000000 ) ;
#68231 = ORIENTED_EDGE ( 'NONE', *, *, #1378, .T. ) ;
#68232 = FACE_OUTER_BOUND ( 'NONE', #17112, .T. ) ;
#68233 = CIRCLE ( 'NONE', #78726, 0.09999999999999982514 ) ;
#68234 = CARTESIAN_POINT ( 'NONE',  ( 11.24999999999994493, 12.50000000000000000, -2.165063509461101710 ) ) ;
#68235 = ORIENTED_EDGE ( 'NONE', *, *, #37426, .F. ) ;
#68236 = DIRECTION ( 'NONE',  ( -4.274815082592931898E-19, -0.9999939076577903929, -0.003490651415223739937 ) ) ;
#68237 = ORIENTED_EDGE ( 'NONE', *, *, #54295, .T. ) ;
#68239 = CIRCLE ( 'NONE', #18064, 0.1000000000000002554 ) ;
#68238 = DIRECTION ( 'NONE',  ( 0.000000000000000000, 0.000000000000000000, -1.000000000000000000 ) ) ;
#68241 = AXIS2_PLACEMENT_3D ( 'NONE', #74729, #45278, #77303 ) ;
#68240 = CIRCLE ( 'NONE', #126754, 0.1000000000000002554 ) ;
#68242 = VERTEX_POINT ( 'NONE', #63847 ) ;
#68243 = FACE_OUTER_BOUND ( 'NONE', #31809, .T. ) ;
#68244 = DIRECTION ( 'NONE',  ( 0.000000000000000000, 1.000000000000000000, 0.000000000000000000 ) ) ;
#68245 = ORIENTED_EDGE ( 'NONE', *, *, #22119, .F. ) ;
#68246 = EDGE_LOOP ( 'NONE', ( #33232, #31552 ) ) ;
#68247 = DIRECTION ( 'NONE',  ( 0.000000000000000000, 0.000000000000000000, 1.000000000000000000 ) ) ;
#68248 = DIRECTION ( 'NONE',  ( 0.000000000000000000, 0.000000000000000000, -1.000000000000000000 ) ) ;
#68249 = EDGE_LOOP ( 'NONE', ( #109348, #64960, #18649, #30612 ) ) ;
#68250 = FACE_OUTER_BOUND ( 'NONE', #93327, .T. ) ;
#68251 = CARTESIAN_POINT ( 'NONE',  ( -9.350000000000008527, 12.50000000000000000, -6.083687093685483660 ) ) ;
#68252 = EDGE_CURVE ( 'NONE', #121281, #38892, #82857, .T. ) ;
#68253 = CARTESIAN_POINT ( 'NONE',  ( 108.0000000000000142, 7.119691004531020440, 5.000000000000004441 ) ) ;
#68254 = CARTESIAN_POINT ( 'NONE',  ( 3.549999999999941203, 2.500000000000000000, 6.248780366869521430 ) ) ;
#68255 = CARTESIAN_POINT ( 'NONE',  ( -1.900000000000034994, 2.500000000000000000, -4.576537180435978236 ) ) ;
#68256 = DIRECTION ( 'NONE',  ( 0.000000000000000000, 0.000000000000000000, 1.000000000000000000 ) ) ;
#68257 = ORIENTED_EDGE ( 'NONE', *, *, #124497, .T. ) ;
#68258 = ORIENTED_EDGE ( 'NONE', *, *, #57402, .T. ) ;
#68259 = ORIENTED_EDGE ( 'NONE', *, *, #12348, .T. ) ;
#68260 = ORIENTED_EDGE ( 'NONE', *, *, #56749, .T. ) ;
#68261 = DIRECTION ( 'NONE',  ( 0.000000000000000000, 1.000000000000000000, 0.000000000000000000 ) ) ;
#68262 = CARTESIAN_POINT ( 'NONE',  ( -10.00000000000000533, 2.500000000000000000, 4.922947341949748257 ) ) ;
#68263 = DIRECTION ( 'NONE',  ( 0.000000000000000000, 0.000000000000000000, 1.000000000000000000 ) ) ;
#68264 = VERTEX_POINT ( 'NONE', #3630 ) ;
#68265 = ADVANCED_FACE ( 'NONE', ( #14074 ), #24115, .T. ) ;
#68266 = FACE_BOUND ( 'NONE', #94116, .T. ) ;
#68267 = ORIENTED_EDGE ( 'NONE', *, *, #49311, .F. ) ;
#68268 = DIRECTION ( 'NONE',  ( 0.000000000000000000, 0.000000000000000000, 1.000000000000000000 ) ) ;
#68269 = DIRECTION ( 'NONE',  ( -0.000000000000000000, 1.000000000000000000, -0.000000000000000000 ) ) ;
#68270 = DIRECTION ( 'NONE',  ( 0.000000000000000000, 0.000000000000000000, 1.000000000000000000 ) ) ;
#68271 = AXIS2_PLACEMENT_3D ( 'NONE', #1962, #70713, #42566 ) ;
#68272 = CARTESIAN_POINT ( 'NONE',  ( 12.89999999999990266, 12.50000000000000000, 3.637306695894644726 ) ) ;
#68273 = CONICAL_SURFACE ( 'NONE', #89213, 0.09999999999999982514, 0.003490658503988666988 ) ;
#68274 = DIRECTION ( 'NONE',  ( -4.274815082592931898E-19, -0.9999939076577903929, -0.003490651415223739937 ) ) ;
#68275 = DIRECTION ( 'NONE',  ( -0.000000000000000000, -1.000000000000000000, -0.000000000000000000 ) ) ;
#68276 = PLANE ( 'NONE',  #49912 ) ;
#68277 = FACE_OUTER_BOUND ( 'NONE', #12599, .T. ) ;
#68278 = DIRECTION ( 'NONE',  ( -4.274815082592931898E-19, -0.9999939076577903929, -0.003490651415223739937 ) ) ;
#68279 = CARTESIAN_POINT ( 'NONE',  ( 3.749999999999978684, 2.500000000000000000, -2.065063509461102065 ) ) ;
#68281 = CIRCLE ( 'NONE', #107995, 3.000000000000000444 ) ;
#68280 = AXIS2_PLACEMENT_3D ( 'NONE', #53091, #104738, #14428 ) ;
#68282 = VERTEX_POINT ( 'NONE', #6820 ) ;
#68283 = EDGE_LOOP ( 'NONE', ( #33909, #116139 ) ) ;
#68284 = EDGE_LOOP ( 'NONE', ( #46399, #65751, #68257, #30006 ) ) ;
#68285 = EDGE_LOOP ( 'NONE', ( #20374, #129063 ) ) ;
#68286 = FACE_OUTER_BOUND ( 'NONE', #82641, .T. ) ;
#68287 = DIRECTION ( 'NONE',  ( 0.000000000000000000, 0.000000000000000000, -1.000000000000000000 ) ) ;
#68289 = ORIENTED_EDGE ( 'NONE', *, *, #61082, .T. ) ;
#68288 = ORIENTED_EDGE ( 'NONE', *, *, #7478, .T. ) ;
#68290 = ORIENTED_EDGE ( 'NONE', *, *, #88566, .F. ) ;
#68291 = FACE_OUTER_BOUND ( 'NONE', #100096, .T. ) ;
#68292 = AXIS2_PLACEMENT_3D ( 'NONE', #128974, #59592, #28822 ) ;
#68294 = EDGE_CURVE ( 'NONE', #60265, #73054, #7371, .T. ) ;
#68293 = CIRCLE ( 'NONE', #116403, 0.1000000000000000472 ) ;
#68295 = CARTESIAN_POINT ( 'NONE',  ( -4.121192902244064579E-14, 2.500000000000000000, 3.537306695894645081 ) ) ;
#68296 = CARTESIAN_POINT ( 'NONE',  ( 1.649999999999948841, 2.500000000000000000, 6.595190528383296780 ) ) ;
#68297 = FACE_OUTER_BOUND ( 'NONE', #18617, .T. ) ;
#68298 = DIRECTION ( 'NONE',  ( -4.274815082592931898E-19, -0.9999939076577903929, -0.003490651415223739937 ) ) ;
#68299 = CARTESIAN_POINT ( 'NONE',  ( -1.050000000000038680, 12.50000000000000000, 6.841600689897072485 ) ) ;
#68300 = DIRECTION ( 'NONE',  ( -0.000000000000000000, 1.000000000000000000, -0.000000000000000000 ) ) ;
#68301 = ORIENTED_EDGE ( 'NONE', *, *, #66804, .T. ) ;
#68302 = EDGE_CURVE ( 'NONE', #123305, #26624, #74374, .T. ) ;
#68303 = DIRECTION ( 'NONE',  ( -0.000000000000000000, 1.000000000000000000, -0.000000000000000000 ) ) ;
#68304 = ORIENTED_EDGE ( 'NONE', *, *, #34235, .F. ) ;
#68305 = ORIENTED_EDGE ( 'NONE', *, *, #31437, .T. ) ;
#68306 = VERTEX_POINT ( 'NONE', #17957 ) ;
#68307 = ADVANCED_FACE ( 'NONE', ( #36340 ), #105772, .T. ) ;
#68309 = ADVANCED_FACE ( 'NONE', ( #76887 ), #118737, .T. ) ;
#68308 = DIRECTION ( 'NONE',  ( 0.000000000000000000, -0.9999939076577903929, 0.003490651415223739937 ) ) ;
#68311 = ORIENTED_EDGE ( 'NONE', *, *, #41031, .F. ) ;
#68310 = EDGE_CURVE ( 'NONE', #48350, #104335, #30490, .T. ) ;
#68312 = ADVANCED_FACE ( 'NONE', ( #66410 ), #124561, .T. ) ;
#68313 = CIRCLE ( 'NONE', #74579, 0.06509327318403745899 ) ;
#68315 = EDGE_LOOP ( 'NONE', ( #35986, #98887, #112482, #59805 ) ) ;
#68314 = EDGE_CURVE ( 'NONE', #64309, #59989, #97168, .T. ) ;
#68316 = AXIS2_PLACEMENT_3D ( 'NONE', #57678, #4671, #45283 ) ;
#68317 = DIRECTION ( 'NONE',  ( 0.000000000000000000, 0.000000000000000000, 1.000000000000000000 ) ) ;
#68318 = PLANE ( 'NONE',  #66377 ) ;
#68320 = AXIS2_PLACEMENT_3D ( 'NONE', #21223, #52616, #91260 ) ;
#68319 = DIRECTION ( 'NONE',  ( -0.000000000000000000, -1.000000000000000000, -0.000000000000000000 ) ) ;
#68321 = DIRECTION ( 'NONE',  ( -4.274815082592931898E-19, -0.9999939076577903929, -0.003490651415223739937 ) ) ;
#68322 = CARTESIAN_POINT ( 'NONE',  ( -7.050000000000016698, 12.50000000000000000, -6.430097255199264339 ) ) ;
#68323 = ADVANCED_FACE ( 'NONE', ( #87330 ), #13722, .T. ) ;
#68324 = CIRCLE ( 'NONE', #60034, 0.09999999999999982514 ) ;
#68325 = VERTEX_POINT ( 'NONE', #67696 ) ;
#68327 = AXIS2_PLACEMENT_3D ( 'NONE', #80996, #18194, #98050 ) ;
#68326 = DIRECTION ( 'NONE',  ( -0.000000000000000000, 1.000000000000000000, -0.000000000000000000 ) ) ;
#68328 = ADVANCED_FACE ( 'NONE', ( #38261 ), #107636, .F. ) ;
#68329 = EDGE_CURVE ( 'NONE', #15286, #111656, #55947, .T. ) ;
#68330 = EDGE_LOOP ( 'NONE', ( #125571, #9144 ) ) ;
#68331 = CIRCLE ( 'NONE', #83023, 0.1000000000000000056 ) ;
#68332 = CARTESIAN_POINT ( 'NONE',  ( -3.150000000000032330, 12.50000000000000000, -6.148780366869526226 ) ) ;
#68333 = EDGE_LOOP ( 'NONE', ( #74903, #78133 ) ) ;
#68334 = CARTESIAN_POINT ( 'NONE',  ( 1.449999999999952660, 12.50000000000000000, -6.906693963081115939 ) ) ;
#68335 = CARTESIAN_POINT ( 'NONE',  ( 3.749999999999942268, 12.50000000000000000, 1.537336459617582918 ) ) ;
#68336 = ORIENTED_EDGE ( 'NONE', *, *, #44274, .T. ) ;
#68337 = DIRECTION ( 'NONE',  ( 0.000000000000000000, 0.000000000000000000, -1.000000000000000000 ) ) ;
#68338 = CONICAL_SURFACE ( 'NONE', #118502, 0.09999999999999982514, 0.003490658503988666988 ) ;
#68339 = CARTESIAN_POINT ( 'NONE',  ( 12.09999999999990550, 2.500000000000000000, -4.430127018922202176 ) ) ;
#68340 = ORIENTED_EDGE ( 'NONE', *, *, #3345, .T. ) ;
#68341 = CIRCLE ( 'NONE', #74605, 0.06509327318403745899 ) ;
#68343 = CIRCLE ( 'NONE', #28647, 0.06509327318403745899 ) ;
#68342 = AXIS2_PLACEMENT_3D ( 'NONE', #129363, #28561, #108398 ) ;
#68344 = PLANE ( 'NONE',  #80175 ) ;
#68345 = ORIENTED_EDGE ( 'NONE', *, *, #27666, .F. ) ;
#68346 = VERTEX_POINT ( 'NONE', #65763 ) ;
#68347 = CARTESIAN_POINT ( 'NONE',  ( 4.599999999999935696, 2.500000000000000000, 5.022947341949748790 ) ) ;
#68348 = DIRECTION ( 'NONE',  ( 0.000000000000000000, 0.000000000000000000, -1.000000000000000000 ) ) ;
#68349 = CARTESIAN_POINT ( 'NONE',  ( 186.5885416670080872, -6.551208109652273848, -3.782341765625003571 ) ) ;
#68350 = LINE ( 'NONE', #30385, #122311 ) ;
#68351 = CARTESIAN_POINT ( 'NONE',  ( 2.949999999999946887, 2.500000000000000000, -6.495190528383302464 ) ) ;
#68352 = DIRECTION ( 'NONE',  ( 0.000000000000000000, 0.000000000000000000, 1.000000000000000000 ) ) ;
#68353 = AXIS2_PLACEMENT_3D ( 'NONE', #125446, #97915, #16111 ) ;
#68354 = ORIENTED_EDGE ( 'NONE', *, *, #101548, .F. ) ;
#68355 = CARTESIAN_POINT ( 'NONE',  ( 12.94999999999989981, 2.500000000000000000, -2.165063509461101710 ) ) ;
#68356 = CARTESIAN_POINT ( 'NONE',  ( -7.500000000000016875, 12.50000000000000000, 0.6277270498435120194 ) ) ;
#68357 = VERTEX_POINT ( 'NONE', #78840 ) ;
#68358 = CARTESIAN_POINT ( 'NONE',  ( -14.34999999999998543, 2.500000000000000000, 1.818653347947325472 ) ) ;
#68359 = CARTESIAN_POINT ( 'NONE',  ( -10.60000000000000320, 2.500000000000000000, -4.676537180435973440 ) ) ;
#68360 = DIRECTION ( 'NONE',  ( -0.000000000000000000, 1.000000000000000000, -0.000000000000000000 ) ) ;
#68361 = EDGE_CURVE ( 'NONE', #120638, #63670, #91101, .T. ) ;
#68362 = FACE_OUTER_BOUND ( 'NONE', #67295, .T. ) ;
#68363 = CARTESIAN_POINT ( 'NONE',  ( -7.500000000000016875, 2.500000000000000000, 0.7928203230275495672 ) ) ;
#68364 = ORIENTED_EDGE ( 'NONE', *, *, #95264, .T. ) ;
#68365 = EDGE_CURVE ( 'NONE', #51796, #79506, #36736, .T. ) ;
#68366 = AXIS2_PLACEMENT_3D ( 'NONE', #115789, #56216, #96147 ) ;
#68367 = AXIS2_PLACEMENT_3D ( 'NONE', #106990, #64025, #56598 ) ;
#68368 = EDGE_CURVE ( 'NONE', #67262, #27243, #34692, .T. ) ;
#68369 = DIRECTION ( 'NONE',  ( 0.000000000000000000, 0.000000000000000000, -1.000000000000000000 ) ) ;
#68370 = LINE ( 'NONE', #36989, #35075 ) ;
#68371 = ORIENTED_EDGE ( 'NONE', *, *, #122981, .F. ) ;
#68372 = EDGE_CURVE ( 'NONE', #15536, #92369, #6191, .T. ) ;
#68374 = AXIS2_PLACEMENT_3D ( 'NONE', #81717, #52276, #3176 ) ;
#68373 = AXIS2_PLACEMENT_3D ( 'NONE', #58254, #35383, #107334 ) ;
#68375 = CARTESIAN_POINT ( 'NONE',  ( 1.449999999999951328, 12.50000000000000000, -1.818653347947326138 ) ) ;
#68376 = ORIENTED_EDGE ( 'NONE', *, *, #66156, .F. ) ;
#68377 = VERTEX_POINT ( 'NONE', #116151 ) ;
#68378 = DIRECTION ( 'NONE',  ( 0.000000000000000000, 0.000000000000000000, 1.000000000000000000 ) ) ;
#68379 = ORIENTED_EDGE ( 'NONE', *, *, #31477, .F. ) ;
#68380 = CARTESIAN_POINT ( 'NONE',  ( 12.09999999999990550, 2.500000000000000000, -5.122947341949753763 ) ) ;
#68381 = CARTESIAN_POINT ( 'NONE',  ( 4.399999999999939071, 12.50000000000000000, 0.3464101615137736845 ) ) ;
#68383 = VECTOR ( 'NONE', #120417, 1000.000000000000000 ) ;
#68382 = AXIS2_PLACEMENT_3D ( 'NONE', #98601, #39736, #128093 ) ;
#68384 = LINE ( 'NONE', #60369, #112818 ) ;
#68385 = ORIENTED_EDGE ( 'NONE', *, *, #98468, .T. ) ;
#68386 = CIRCLE ( 'NONE', #76715, 0.1000000000000002554 ) ;
#68387 = DIRECTION ( 'NONE',  ( 0.000000000000000000, 0.000000000000000000, -1.000000000000000000 ) ) ;
#68389 = VERTEX_POINT ( 'NONE', #26505 ) ;
#68388 = CARTESIAN_POINT ( 'NONE',  ( -3.950000000000024603, 2.500000000000000000, 1.818653347947321475 ) ) ;
#68390 = FACE_OUTER_BOUND ( 'NONE', #127334, .T. ) ;
#68391 = DIRECTION ( 'NONE',  ( 0.000000000000000000, 1.000000000000000000, 0.000000000000000000 ) ) ;
#68392 = ADVANCED_FACE ( 'NONE', ( #56578 ), #84831, .T. ) ;
#68393 = VERTEX_POINT ( 'NONE', #86702 ) ;
#68394 = VERTEX_POINT ( 'NONE', #126637 ) ;
#68395 = EDGE_LOOP ( 'NONE', ( #108454, #75842, #122509, #110165 ) ) ;
#68396 = LINE ( 'NONE', #57302, #102739 ) ;
#68397 = CARTESIAN_POINT ( 'NONE',  ( -4.150000000000028777, 2.500000000000000000, -5.702370205355749455 ) ) ;
#68398 = CARTESIAN_POINT ( 'NONE',  ( -3.950000000000026379, 12.50000000000000000, 2.511473670974873507 ) ) ;
#68399 = FACE_BOUND ( 'NONE', #45477, .T. ) ;
#68400 = ORIENTED_EDGE ( 'NONE', *, *, #24859, .F. ) ;
#68401 = DIRECTION ( 'NONE',  ( 0.000000000000000000, 1.000000000000000000, 0.000000000000000000 ) ) ;
#68402 = DIRECTION ( 'NONE',  ( 0.000000000000000000, 0.000000000000000000, -1.000000000000000000 ) ) ;
#68403 = EDGE_LOOP ( 'NONE', ( #13999, #28920 ) ) ;
#68404 = DIRECTION ( 'NONE',  ( 0.000000000000000000, 0.000000000000000000, 1.000000000000000000 ) ) ;
#68405 = CARTESIAN_POINT ( 'NONE',  ( 12.49999999999993605, 2.500000000000000000, -0.1000000000000022815 ) ) ;
#68406 = AXIS2_PLACEMENT_3D ( 'NONE', #51975, #110237, #20573 ) ;
#68407 = EDGE_CURVE ( 'NONE', #75029, #39867, #28417, .T. ) ;
#68408 = LINE ( 'NONE', #50094, #98755 ) ;
#68409 = DIRECTION ( 'NONE',  ( -0.000000000000000000, 1.000000000000000000, -0.000000000000000000 ) ) ;
#68410 = FACE_OUTER_BOUND ( 'NONE', #106763, .T. ) ;
#68411 = CARTESIAN_POINT ( 'NONE',  ( 6.049999999999934097, 2.500000000000000000, -2.611473670974877592 ) ) ;
#68412 = AXIS2_PLACEMENT_3D ( 'NONE', #62508, #13379, #63788 ) ;
#68413 = CARTESIAN_POINT ( 'NONE',  ( 0.8499999999999545697, 2.500000000000000000, 2.757883832488649656 ) ) ;
#68414 = AXIS2_PLACEMENT_3D ( 'NONE', #54111, #13529, #121547 ) ;
#68415 = CIRCLE ( 'NONE', #37137, 0.09999999999999982514 ) ;
#68416 = AXIS2_PLACEMENT_3D ( 'NONE', #100107, #71945, #51662 ) ;
#68417 = VERTEX_POINT ( 'NONE', #110217 ) ;
#68418 = EDGE_LOOP ( 'NONE', ( #88696, #25262 ) ) ;
#68419 = ORIENTED_EDGE ( 'NONE', *, *, #13941, .T. ) ;
#68420 = ORIENTED_EDGE ( 'NONE', *, *, #93314, .F. ) ;
#68421 = ORIENTED_EDGE ( 'NONE', *, *, #101434, .T. ) ;
#68422 = DIRECTION ( 'NONE',  ( 0.000000000000000000, -0.9999939076577903929, 0.003490651415223739937 ) ) ;
#68423 = DIRECTION ( 'NONE',  ( 0.000000000000000000, 0.000000000000000000, -1.000000000000000000 ) ) ;
#68424 = AXIS2_PLACEMENT_3D ( 'NONE', #128874, #119025, #28069 ) ;
#68425 = ORIENTED_EDGE ( 'NONE', *, *, #4776, .F. ) ;
#68426 = EDGE_CURVE ( 'NONE', #61737, #128722, #47192, .T. ) ;
#68427 = FACE_BOUND ( 'NONE', #40772, .T. ) ;
#68428 = DIRECTION ( 'NONE',  ( -0.000000000000000000, 1.000000000000000000, -0.000000000000000000 ) ) ;
#68429 = AXIS2_PLACEMENT_3D ( 'NONE', #108245, #27744, #78811 ) ;
#68430 = DIRECTION ( 'NONE',  ( 0.000000000000000000, 0.000000000000000000, -1.000000000000000000 ) ) ;
#68431 = DIRECTION ( 'NONE',  ( 0.000000000000000000, 0.000000000000000000, 1.000000000000000000 ) ) ;
#68432 = DIRECTION ( 'NONE',  ( -0.000000000000000000, 1.000000000000000000, -0.000000000000000000 ) ) ;
#68433 = CARTESIAN_POINT ( 'NONE',  ( 5.849999999999933031, 12.50000000000000000, -1.472243186433550122 ) ) ;
#68434 = VERTEX_POINT ( 'NONE', #61108 ) ;
#68435 = EDGE_LOOP ( 'NONE', ( #108250, #28311 ) ) ;
#68436 = ORIENTED_EDGE ( 'NONE', *, *, #103486, .F. ) ;
#68437 = EDGE_LOOP ( 'NONE', ( #53188, #103118 ) ) ;
#68438 = DIRECTION ( 'NONE',  ( 0.000000000000000000, -0.9999939076577903929, 0.003490651415223739937 ) ) ;
#68439 = DIRECTION ( 'NONE',  ( 0.000000000000000000, 1.000000000000000000, 0.000000000000000000 ) ) ;
#68440 = DIRECTION ( 'NONE',  ( -0.000000000000000000, 1.000000000000000000, -0.000000000000000000 ) ) ;
#68441 = ORIENTED_EDGE ( 'NONE', *, *, #12365, .T. ) ;
#68442 = AXIS2_PLACEMENT_3D ( 'NONE', #69097, #98543, #8882 ) ;
#68443 = CARTESIAN_POINT ( 'NONE',  ( 14.79999999999989235, 2.500000000000000000, 0.3464101615137735735 ) ) ;
#68444 = DIRECTION ( 'NONE',  ( 0.000000000000000000, -0.9999939076577903929, 0.003490651415223739937 ) ) ;
#68445 = EDGE_CURVE ( 'NONE', #119116, #34711, #19909, .T. ) ;
#68446 = CARTESIAN_POINT ( 'NONE',  ( -6.900000000000019007, 2.500000000000000000, -3.983716857408426293 ) ) ;
#68447 = CARTESIAN_POINT ( 'NONE',  ( 185.6093750003413732, 9.264065473108010111E-16, -7.564683531250000925 ) ) ;
#68448 = LINE ( 'NONE', #79577, #115655 ) ;
#68449 = CARTESIAN_POINT ( 'NONE',  ( 10.39999999999991154, 12.50000000000000000, -3.637306695894650055 ) ) ;
#68450 = DIRECTION ( 'NONE',  ( -4.274815082592931898E-19, -0.9999939076577903929, -0.003490651415223739937 ) ) ;
#68451 = ORIENTED_EDGE ( 'NONE', *, *, #49900, .F. ) ;
#68452 = CARTESIAN_POINT ( 'NONE',  ( -5.450000000000023270, 12.50000000000000000, -2.165063509461101710 ) ) ;
#68453 = ADVANCED_FACE ( 'NONE', ( #40189 ), #82029, .T. ) ;
#68454 = CONICAL_SURFACE ( 'NONE', #118629, 0.1000000000000000472, 0.003490658503988666988 ) ;
#68455 = ORIENTED_EDGE ( 'NONE', *, *, #125046, .T. ) ;
#68456 = VERTEX_POINT ( 'NONE', #899 ) ;
#68457 = DIRECTION ( 'NONE',  ( 0.000000000000000000, 1.000000000000000000, 0.000000000000000000 ) ) ;
#68458 = EDGE_CURVE ( 'NONE', #55788, #99080, #40958, .T. ) ;
#68459 = LINE ( 'NONE', #16764, #67603 ) ;
#68461 = EDGE_CURVE ( 'NONE', #97339, #98598, #38908, .T. ) ;
#68460 = FACE_OUTER_BOUND ( 'NONE', #65909, .T. ) ;
#68462 = ADVANCED_FACE ( 'NONE', ( #80761 ), #80648, .T. ) ;
#68463 = EDGE_CURVE ( 'NONE', #84736, #117651, #93174, .T. ) ;
#68464 = VERTEX_POINT ( 'NONE', #120681 ) ;
#68466 = ORIENTED_EDGE ( 'NONE', *, *, #96973, .F. ) ;
#68465 = CIRCLE ( 'NONE', #120704, 0.06509327318403745899 ) ;
#68467 = CARTESIAN_POINT ( 'NONE',  ( 8.349999999999919709, 12.50000000000000000, 7.253104124594885960 ) ) ;
#68468 = AXIS2_PLACEMENT_3D ( 'NONE', #86498, #74760, #53823 ) ;
#68469 = DIRECTION ( 'NONE',  ( -4.274815082592931898E-19, -0.9999939076577903929, -0.003490651415223739937 ) ) ;
#68470 = ADVANCED_FACE ( 'NONE', ( #51946 ), #32646, .T. ) ;
#68471 = DIRECTION ( 'NONE',  ( -0.000000000000000000, 1.000000000000000000, -0.000000000000000000 ) ) ;
#68472 = ORIENTED_EDGE ( 'NONE', *, *, #110712, .T. ) ;
#68473 = ORIENTED_EDGE ( 'NONE', *, *, #60957, .F. ) ;
#68474 = ADVANCED_FACE ( 'NONE', ( #79478 ), #112035, .T. ) ;
#68475 = DIRECTION ( 'NONE',  ( 0.000000000000000000, -0.000000000000000000, 1.000000000000000000 ) ) ;
#68476 = EDGE_CURVE ( 'NONE', #51418, #11992, #70932, .T. ) ;
#68477 = AXIS2_PLACEMENT_3D ( 'NONE', #9454, #125982, #36354 ) ;
#68478 = ORIENTED_EDGE ( 'NONE', *, *, #124814, .F. ) ;
#68479 = DIRECTION ( 'NONE',  ( 0.000000000000000000, 1.000000000000000000, 0.000000000000000000 ) ) ;
#68480 = EDGE_CURVE ( 'NONE', #28877, #35030, #69639, .T. ) ;
#68481 = AXIS2_PLACEMENT_3D ( 'NONE', #62961, #74716, #93083 ) ;
#68482 = EDGE_CURVE ( 'NONE', #116451, #103569, #86887, .T. ) ;
#68483 = ORIENTED_EDGE ( 'NONE', *, *, #66722, .F. ) ;
#68484 = DIRECTION ( 'NONE',  ( 0.000000000000000000, 1.000000000000000000, 0.000000000000000000 ) ) ;
#68485 = CARTESIAN_POINT ( 'NONE',  ( -2.900000000000029665, 12.50000000000000000, 3.637306695894644726 ) ) ;
#68486 = DIRECTION ( 'NONE',  ( 1.000000000000000000, 0.000000000000000000, 0.000000000000000000 ) ) ;
#68488 = ADVANCED_FACE ( 'NONE', ( #2179 ), #32543, .T. ) ;
#68487 = FACE_OUTER_BOUND ( 'NONE', #62699, .T. ) ;
#68489 = VERTEX_POINT ( 'NONE', #129237 ) ;
#68491 = AXIS2_PLACEMENT_3D ( 'NONE', #91951, #71662, #111588 ) ;
#68490 = DIRECTION ( 'NONE',  ( 0.000000000000000000, 0.000000000000000000, 1.000000000000000000 ) ) ;
#68492 = CONICAL_SURFACE ( 'NONE', #5777, 0.1000000000000002554, 0.003490658503988666988 ) ;
#68493 = EDGE_LOOP ( 'NONE', ( #1582, #71537, #36614, #84481 ) ) ;
#68494 = ORIENTED_EDGE ( 'NONE', *, *, #25060, .T. ) ;
#68495 = FACE_OUTER_BOUND ( 'NONE', #55588, .T. ) ;
#68496 = PLANE ( 'NONE',  #128509 ) ;
#68497 = CARTESIAN_POINT ( 'NONE',  ( -1.050000000000037792, 2.500000000000000000, 6.248780366869520542 ) ) ;
#68498 = DIRECTION ( 'NONE',  ( -0.000000000000000000, 1.000000000000000000, -0.000000000000000000 ) ) ;
#68499 = CIRCLE ( 'NONE', #112523, 0.1000000000000002554 ) ;
#68501 = AXIS2_PLACEMENT_3D ( 'NONE', #109771, #27985, #17503 ) ;
#68500 = CARTESIAN_POINT ( 'NONE',  ( 0.3999999999999628852, 2.500000000000000000, -0.5928203230275519431 ) ) ;
#68502 = CARTESIAN_POINT ( 'NONE',  ( -14.39999999999998614, 2.500000000000000000, 0.4464101615137758272 ) ) ;
#68503 = CARTESIAN_POINT ( 'NONE',  ( -0.4000000000000396572, 2.500000000000000000, 3.637306695894644726 ) ) ;
#68504 = DIRECTION ( 'NONE',  ( -0.000000000000000000, 1.000000000000000000, -0.000000000000000000 ) ) ;
#68505 = CARTESIAN_POINT ( 'NONE',  ( 5.849999999999935696, 2.500000000000000000, -7.188010851410854052 ) ) ;
#68506 = CIRCLE ( 'NONE', #85240, 0.09999999999999982514 ) ;
#68507 = AXIS2_PLACEMENT_3D ( 'NONE', #101130, #102421, #82795 ) ;
#68508 = FACE_OUTER_BOUND ( 'NONE', #31968, .T. ) ;
#68509 = CIRCLE ( 'NONE', #85244, 0.06509327318403745899 ) ;
#68510 = VERTEX_POINT ( 'NONE', #59854 ) ;
#68511 = LINE ( 'NONE', #8297, #42210 ) ;
#68512 = LINE ( 'NONE', #49542, #4000 ) ;
#68513 = CARTESIAN_POINT ( 'NONE',  ( 0.8499999999999527933, 12.50000000000000000, 7.188010851410848723 ) ) ;
#68514 = DIRECTION ( 'NONE',  ( -0.000000000000000000, -1.000000000000000000, -0.000000000000000000 ) ) ;
#68515 = CARTESIAN_POINT ( 'NONE',  ( -3.469446951953614189E-14, 2.500000000000000000, -0.6928203230275519209 ) ) ;
#68516 = EDGE_LOOP ( 'NONE', ( #1323, #27140, #120428, #102373 ) ) ;
#68517 = DIRECTION ( 'NONE',  ( 0.000000000000000000, 1.000000000000000000, 0.000000000000000000 ) ) ;
#68518 = EDGE_CURVE ( 'NONE', #68896, #107669, #99112, .T. ) ;
#68520 = VECTOR ( 'NONE', #116675, 1000.000000000000000 ) ;
#68519 = AXIS2_PLACEMENT_3D ( 'NONE', #34871, #83930, #5375 ) ;
#68521 = EDGE_CURVE ( 'NONE', #90590, #60385, #105686, .T. ) ;
#68522 = DIRECTION ( 'NONE',  ( -0.000000000000000000, 1.000000000000000000, -0.000000000000000000 ) ) ;
#68524 = EDGE_LOOP ( 'NONE', ( #105119, #44161, #129090, #64088 ) ) ;
#68523 = CARTESIAN_POINT ( 'NONE',  ( 9.999999999999912959, 2.500000000000000000, -5.122947341949753763 ) ) ;
#68525 =( BOUNDED_SURFACE ( )  B_SPLINE_SURFACE ( 3, 2, ( 
 ( #54750, #94683, #45607 ),
 ( #97266, #75056, #75678 ),
 ( #14808, #17396, #124804 ),
 ( #116889, #46890, #96602 ),
 ( #77615, #5008, #44958 ),
 ( #6922, #84867, #114958 ),
 ( #7588, #117520, #107073 ),
 ( #95339, #35150, #27883 ),
 ( #87437, #27231, #105144 ),
 ( #65211, #15473, #95983 ),
 ( #126736, #65871, #85515 ),
 ( #57346, #35775, #55417 ),
 ( #5649, #105803, #115602 ),
 ( #127383, #25959, #6284 ),
 ( #86133, #126072, #36440 ),
 ( #76348, #76986, #47534 ) ),
 .UNSPECIFIED., .F., .F., .F. ) 
 B_SPLINE_SURFACE_WITH_KNOTS ( ( 4, 2, 2, 2, 2, 2, 2, 4 ),
 ( 3, 3 ),
 ( 0.000000000000000000, 0.003502803217043997438, 0.007005606434087994876, 0.008757008042609993811, 0.01050840965113199188, 0.01225981125965399168, 0.01313551206391498985, 0.01401121286817598975 ),
 ( 0.000000000000000000, 1.000000000000000000 ),
 .UNSPECIFIED. ) 
 GEOMETRIC_REPRESENTATION_ITEM ( )  RATIONAL_B_SPLINE_SURFACE ( (
 ( 1.000000000000000000, 0.7071067811865477948, 1.000000000000000000),
 ( 1.000000000000000000, 0.7071067811865477948, 1.000000000000000000),
 ( 1.000000000000000000, 0.7071067811865476838, 1.000000000000000000),
 ( 1.000000000000000000, 0.7071067811865476838, 1.000000000000000000),
 ( 1.000000000000000000, 0.7071067811865476838, 1.000000000000000000),
 ( 1.000000000000000000, 0.7071067811865476838, 1.000000000000000000),
 ( 1.000000000000000000, 0.7071067811865473507, 1.000000000000000000),
 ( 1.000000000000000000, 0.7071067811865473507, 1.000000000000000000),
 ( 1.000000000000000000, 0.7071067811865475727, 1.000000000000000000),
 ( 1.000000000000000000, 0.7071067811865475727, 1.000000000000000000),
 ( 1.000000000000000000, 0.7071067811865477948, 1.000000000000000000),
 ( 1.000000000000000000, 0.7071067811865477948, 1.000000000000000000),
 ( 1.000000000000000000, 0.7071067811865476838, 1.000000000000000000),
 ( 1.000000000000000000, 0.7071067811865476838, 1.000000000000000000),
 ( 1.000000000000000000, 0.7071067811865476838, 1.000000000000000000),
 ( 1.000000000000000000, 0.7071067811865476838, 1.000000000000000000) ) ) 
 REPRESENTATION_ITEM ( '' )  SURFACE ( )  );
#68526 = ORIENTED_EDGE ( 'NONE', *, *, #2067, .F. ) ;
#68527 = EDGE_CURVE ( 'NONE', #1406, #71123, #103630, .T. ) ;
#68528 = CARTESIAN_POINT ( 'NONE',  ( 10.39999999999991154, 2.500000000000000000, 3.637306695894644726 ) ) ;
#68529 = ADVANCED_FACE ( 'NONE', ( #242 ), #126620, .T. ) ;
#68530 = VERTEX_POINT ( 'NONE', #122615 ) ;
#68531 = ORIENTED_EDGE ( 'NONE', *, *, #50913, .F. ) ;
#68532 = ORIENTED_EDGE ( 'NONE', *, *, #38811, .T. ) ;
#68533 = CARTESIAN_POINT ( 'NONE',  ( 14.34999999999989306, 2.500000000000000000, -2.611473670974877592 ) ) ;
#68534 = DIRECTION ( 'NONE',  ( 0.000000000000000000, 0.000000000000000000, 1.000000000000000000 ) ) ;
#68535 = CARTESIAN_POINT ( 'NONE',  ( -1.850000000000033396, 12.50000000000000000, -2.511473670974877948 ) ) ;
#68536 = CARTESIAN_POINT ( 'NONE',  ( -4.150000000000024336, 12.50000000000000000, -2.857883832488653741 ) ) ;
#68537 = ORIENTED_EDGE ( 'NONE', *, *, #99979, .F. ) ;
#68538 = CARTESIAN_POINT ( 'NONE',  ( 2.899999999999946620, 12.50000000000000000, 0.6277270498435120194 ) ) ;
#68539 = ORIENTED_EDGE ( 'NONE', *, *, #101532, .F. ) ;
#68540 = FACE_OUTER_BOUND ( 'NONE', #109165, .T. ) ;
#68541 = FACE_OUTER_BOUND ( 'NONE', #68981, .T. ) ;
#68542 = AXIS2_PLACEMENT_3D ( 'NONE', #75052, #25281, #45602 ) ;
#68543 = CARTESIAN_POINT ( 'NONE',  ( 3.349999999999941025, 2.500000000000000000, 7.188010851410848723 ) ) ;
#68544 = CARTESIAN_POINT ( 'NONE',  ( -9.800000000000004263, 12.50000000000000000, -0.3464101615137783474 ) ) ;
#68545 = DIRECTION ( 'NONE',  ( 0.000000000000000000, 0.000000000000000000, -1.000000000000000000 ) ) ;
#68546 = ORIENTED_EDGE ( 'NONE', *, *, #97544, .T. ) ;
#68547 = CONICAL_SURFACE ( 'NONE', #110325, 0.09999999999999982514, 0.003490658503988666988 ) ;
#68548 = CIRCLE ( 'NONE', #12116, 0.06509327318403745899 ) ;
#68549 = EDGE_LOOP ( 'NONE', ( #23113, #124724, #119326, #122733 ) ) ;
#68550 = ORIENTED_EDGE ( 'NONE', *, *, #123170, .F. ) ;
#68551 = ORIENTED_EDGE ( 'NONE', *, *, #129499, .F. ) ;
#68552 = ORIENTED_EDGE ( 'NONE', *, *, #63070, .T. ) ;
#68553 = CARTESIAN_POINT ( 'NONE',  ( 11.84999999999990727, 2.500000000000000000, 6.148780366869520009 ) ) ;
#68554 = DIRECTION ( 'NONE',  ( -0.000000000000000000, 1.000000000000000000, -0.000000000000000000 ) ) ;
#68555 = CARTESIAN_POINT ( 'NONE',  ( 11.84999999999990727, 2.500000000000000000, -2.511473670974877948 ) ) ;
#68556 = FACE_BOUND ( 'NONE', #128911, .T. ) ;
#68557 = DIRECTION ( 'NONE',  ( 0.000000000000000000, 1.000000000000000000, 0.000000000000000000 ) ) ;
#68558 = CARTESIAN_POINT ( 'NONE',  ( 186.7395833340161175, 4.445597072760117285, 7.699999999999999289 ) ) ;
#68559 = CONICAL_SURFACE ( 'NONE', #112397, 0.09999999999999982514, 0.003490658503988666988 ) ;
#68560 = DIRECTION ( 'NONE',  ( -1.000000000000000000, -0.000000000000000000, -0.000000000000000000 ) ) ;
#68561 = CARTESIAN_POINT ( 'NONE',  ( -6.250000000000015987, 12.50000000000000000, 5.737276932171707422 ) ) ;
#68562 = ADVANCED_FACE ( 'NONE', ( #112149 ), #13813, .T. ) ;
#68563 = AXIS2_PLACEMENT_3D ( 'NONE', #82536, #113264, #1367 ) ;
#68564 = CARTESIAN_POINT ( 'NONE',  ( 185.2552083336747444, 6.551208109652275624, -3.782341765624998686 ) ) ;
#68565 = DIRECTION ( 'NONE',  ( -4.274815082592931898E-19, -0.9999939076577903929, -0.003490651415223739937 ) ) ;
#68566 = DIRECTION ( 'NONE',  ( -0.000000000000000000, -1.000000000000000000, -0.000000000000000000 ) ) ;
#68567 = VECTOR ( 'NONE', #36083, 1000.000000000000000 ) ;
#68568 = CARTESIAN_POINT ( 'NONE',  ( -10.60000000000000142, 2.500000000000000000, 3.983716857408420964 ) ) ;
#68569 = ORIENTED_EDGE ( 'NONE', *, *, #88887, .T. ) ;
#68570 = EDGE_LOOP ( 'NONE', ( #68290, #22520, #116765, #15647 ) ) ;
#68571 = ORIENTED_EDGE ( 'NONE', *, *, #39379, .F. ) ;
#68572 = EDGE_LOOP ( 'NONE', ( #102576, #127057, #4769, #61846 ) ) ;
#68573 = EDGE_CURVE ( 'NONE', #63096, #113352, #32325, .T. ) ;
#68574 = AXIS2_PLACEMENT_3D ( 'NONE', #19908, #128591, #88636 ) ;
#68575 = DIRECTION ( 'NONE',  ( 0.000000000000000000, 0.000000000000000000, -1.000000000000000000 ) ) ;
#68576 = DIRECTION ( 'NONE',  ( 0.000000000000000000, 0.000000000000000000, 1.000000000000000000 ) ) ;
#68577 = ADVANCED_FACE ( 'NONE', ( #22500 ), #24408, .T. ) ;
#68578 = FACE_BOUND ( 'NONE', #116888, .T. ) ;
#68579 = FACE_OUTER_BOUND ( 'NONE', #4428, .T. ) ;
#68580 = VECTOR ( 'NONE', #108486, 1000.000000000000000 ) ;
#68581 = CIRCLE ( 'NONE', #37212, 0.1000000000000002554 ) ;
#68582 = ORIENTED_EDGE ( 'NONE', *, *, #47858, .T. ) ;
#68583 = DIRECTION ( 'NONE',  ( -0.000000000000000000, -1.000000000000000000, -0.000000000000000000 ) ) ;
#68584 = DIRECTION ( 'NONE',  ( -0.000000000000000000, -1.000000000000000000, -0.000000000000000000 ) ) ;
#68585 = EDGE_CURVE ( 'NONE', #21407, #75499, #92494, .T. ) ;
#68586 = CARTESIAN_POINT ( 'NONE',  ( -5.400000000000019895, 12.50000000000000000, -0.6928203230275541413 ) ) ;
#68587 = FACE_OUTER_BOUND ( 'NONE', #46973, .T. ) ;
#68588 = VECTOR ( 'NONE', #93753, 1000.000000000000000 ) ;
#68589 = VERTEX_POINT ( 'NONE', #84621 ) ;
#68590 = AXIS2_PLACEMENT_3D ( 'NONE', #42581, #2615, #113216 ) ;
#68591 = LINE ( 'NONE', #7075, #93128 ) ;
#68592 = ORIENTED_EDGE ( 'NONE', *, *, #103539, .T. ) ;
#68593 = ORIENTED_EDGE ( 'NONE', *, *, #82357, .T. ) ;
#68594 = FACE_OUTER_BOUND ( 'NONE', #24738, .T. ) ;
#68595 = CARTESIAN_POINT ( 'NONE',  ( -3.150000000000029665, 12.50000000000000000, 6.841600689897072485 ) ) ;
#68596 = AXIS2_PLACEMENT_3D ( 'NONE', #83895, #82633, #54437 ) ;
#68597 = ORIENTED_EDGE ( 'NONE', *, *, #66576, .F. ) ;
#68598 = LINE ( 'NONE', #118994, #5024 ) ;
#68599 = DIRECTION ( 'NONE',  ( 0.000000000000000000, 0.000000000000000000, -1.000000000000000000 ) ) ;
#68600 = VERTEX_POINT ( 'NONE', #113431 ) ;
#68601 = CARTESIAN_POINT ( 'NONE',  ( 8.149999999999923972, 12.50000000000000000, -6.148780366869526226 ) ) ;
#68602 = ORIENTED_EDGE ( 'NONE', *, *, #94674, .T. ) ;
#68603 = AXIS2_PLACEMENT_3D ( 'NONE', #110438, #52175, #40441 ) ;
#68604 = CARTESIAN_POINT ( 'NONE',  ( -6.249999999999984901, 12.50000000000000000, -6.495190528383302464 ) ) ;
#68605 = ORIENTED_EDGE ( 'NONE', *, *, #2129, .F. ) ;
#68606 = CARTESIAN_POINT ( 'NONE',  ( 186.5312500006828031, 9.429780353434619030E-16, -7.700000000000000178 ) ) ;
#68607 = FACE_BOUND ( 'NONE', #89198, .T. ) ;
#68608 = ADVANCED_FACE ( 'NONE', ( #64331 ), #55163, .T. ) ;
#68609 = VECTOR ( 'NONE', #11664, 1000.000000000000000 ) ;
#68610 = ORIENTED_EDGE ( 'NONE', *, *, #36480, .T. ) ;
#68611 = CARTESIAN_POINT ( 'NONE',  ( 111.7537803698471777, 6.952973673849077940, 3.318088645774402323 ) ) ;
#68612 = ORIENTED_EDGE ( 'NONE', *, *, #101872, .F. ) ;
#68613 = DIRECTION ( 'NONE',  ( 1.000000000000000000, -0.000000000000000000, -0.000000000000000000 ) ) ;
#68614 = DIRECTION ( 'NONE',  ( 0.000000000000000000, 1.000000000000000000, 0.000000000000000000 ) ) ;
#68615 = DIRECTION ( 'NONE',  ( 0.000000000000000000, 1.000000000000000000, 0.000000000000000000 ) ) ;
#68617 = EDGE_CURVE ( 'NONE', #26322, #8359, #32725, .T. ) ;
#68616 = DIRECTION ( 'NONE',  ( 0.000000000000000000, 0.000000000000000000, 1.000000000000000000 ) ) ;
#68618 = EDGE_CURVE ( 'NONE', #13662, #3435, #72421, .T. ) ;
#68619 = DIRECTION ( 'NONE',  ( 0.000000000000000000, -0.9999939076577903929, 0.003490651415223739937 ) ) ;
#68620 = EDGE_CURVE ( 'NONE', #88669, #118375, #59771, .T. ) ;
#68621 = ORIENTED_EDGE ( 'NONE', *, *, #74565, .F. ) ;
#68622 = ORIENTED_EDGE ( 'NONE', *, *, #21257, .F. ) ;
#68623 = EDGE_LOOP ( 'NONE', ( #57633, #87079, #62610, #46122 ) ) ;
#68624 = DIRECTION ( 'NONE',  ( 0.000000000000000000, 0.000000000000000000, -1.000000000000000000 ) ) ;
#68625 = DIRECTION ( 'NONE',  ( 0.000000000000000000, 0.000000000000000000, 1.000000000000000000 ) ) ;
#68626 = ADVANCED_FACE ( 'NONE', ( #14571 ), #128881, .T. ) ;
#68627 = DIRECTION ( 'NONE',  ( -0.000000000000000000, -1.000000000000000000, -0.000000000000000000 ) ) ;
#68630 = ORIENTED_EDGE ( 'NONE', *, *, #107475, .F. ) ;
#68629 = EDGE_LOOP ( 'NONE', ( #118009, #41440, #68932, #93557 ) ) ;
#68628 = AXIS2_PLACEMENT_3D ( 'NONE', #32222, #119938, #72132 ) ;
#68631 = EDGE_CURVE ( 'NONE', #101262, #96780, #54501, .T. ) ;
#68632 = EDGE_LOOP ( 'NONE', ( #125516, #36767, #94941, #22364 ) ) ;
#68633 = ADVANCED_FACE ( 'NONE', ( #45350 ), #122597, .T. ) ;
#68634 = DIRECTION ( 'NONE',  ( 0.000000000000000000, 0.000000000000000000, -1.000000000000000000 ) ) ;
#68635 = DIRECTION ( 'NONE',  ( -0.000000000000000000, 1.000000000000000000, -0.000000000000000000 ) ) ;
#68636 = PRODUCT_CONTEXT ( 'NONE', #119053, 'mechanical' ) ;
#68637 = EDGE_CURVE ( 'NONE', #87604, #67674, #51497, .T. ) ;
#68638 = CARTESIAN_POINT ( 'NONE',  ( -12.04999999999999538, 12.50000000000000000, 2.230156782645134950 ) ) ;
#68639 = CARTESIAN_POINT ( 'NONE',  ( 1.049999999999954081, 2.500000000000000000, -6.048780366869526581 ) ) ;
#68640 = CIRCLE ( 'NONE', #118815, 0.06509327318403743123 ) ;
#68641 = DIRECTION ( 'NONE',  ( 0.000000000000000000, 0.000000000000000000, 1.000000000000000000 ) ) ;
#68642 = DIRECTION ( 'NONE',  ( 0.000000000000000000, 0.000000000000000000, 1.000000000000000000 ) ) ;
#68643 = DIRECTION ( 'NONE',  ( 0.000000000000000000, 0.000000000000000000, 1.000000000000000000 ) ) ;
#68644 = EDGE_CURVE ( 'NONE', #103825, #65666, #103730, .T. ) ;
#68646 = EDGE_CURVE ( 'NONE', #49853, #42996, #124655, .T. ) ;
#68645 = DIRECTION ( 'NONE',  ( 0.000000000000000000, 0.000000000000000000, -1.000000000000000000 ) ) ;
#68647 = VECTOR ( 'NONE', #55109, 1000.000000000000000 ) ;
#68648 = ORIENTED_EDGE ( 'NONE', *, *, #111733, .F. ) ;
#68650 = EDGE_LOOP ( 'NONE', ( #40347, #129468 ) ) ;
#68649 = AXIS2_PLACEMENT_3D ( 'NONE', #5200, #63502, #4538 ) ;
#68652 = CARTESIAN_POINT ( 'NONE',  ( 4.349999999999941025, 12.50000000000000000, -6.148780366869526226 ) ) ;
#68651 = CIRCLE ( 'NONE', #83237, 0.06509327318403745899 ) ;
#68653 = CARTESIAN_POINT ( 'NONE',  ( 10.39999999999991154, 12.50000000000000000, -5.022947341949754119 ) ) ;
#68654 = ORIENTED_EDGE ( 'NONE', *, *, #69040, .T. ) ;
#68655 = VERTEX_POINT ( 'NONE', #4740 ) ;
#68656 = FACE_OUTER_BOUND ( 'NONE', #8955, .T. ) ;
#68657 = DIRECTION ( 'NONE',  ( 0.000000000000000000, 0.000000000000000000, 1.000000000000000000 ) ) ;
#68658 = CARTESIAN_POINT ( 'NONE',  ( -11.64999999999999680, 12.50000000000000000, 5.802370205355744659 ) ) ;
#68659 = VECTOR ( 'NONE', #57461, 1000.000000000000000 ) ;
#68660 = CARTESIAN_POINT ( 'NONE',  ( 8.349999999999923261, 12.50000000000000000, -5.802370205355749988 ) ) ;
#68661 = AXIS2_PLACEMENT_3D ( 'NONE', #56274, #5871, #105384 ) ;
#68662 = DIRECTION ( 'NONE',  ( -0.000000000000000000, -1.000000000000000000, -0.000000000000000000 ) ) ;
#68663 = CARTESIAN_POINT ( 'NONE',  ( 0.3999999999999628852, 2.500000000000000000, -0.5928203230275519431 ) ) ;
#68664 = CARTESIAN_POINT ( 'NONE',  ( 6.699999999999928235, 12.50000000000000000, -2.276824562219559311E-15 ) ) ;
#68665 = DIRECTION ( 'NONE',  ( 0.000000000000000000, 1.000000000000000000, 0.000000000000000000 ) ) ;
#68666 = CIRCLE ( 'NONE', #127178, 0.09999999999999982514 ) ;
#68667 = ORIENTED_EDGE ( 'NONE', *, *, #101903, .F. ) ;
#68668 = EDGE_LOOP ( 'NONE', ( #48118, #55462, #10343, #62159 ) ) ;
#68669 = CLOSED_SHELL ( 'NONE', ( #16276, #48807, #67059, #118857, #59212, #126596, #85161, #11728, #18489, #102884, #52200, #104542, #70470, #107654, #101771, #34781, #34787, #100184, #51471, #113671 ) ) ;
#68670 = CONICAL_SURFACE ( 'NONE', #120898, 0.09999999999999982514, 0.003490658503988666988 ) ;
#68671 = ORIENTED_EDGE ( 'NONE', *, *, #72415, .F. ) ;
#68672 = ORIENTED_EDGE ( 'NONE', *, *, #103174, .T. ) ;
#68673 = CARTESIAN_POINT ( 'NONE',  ( 12.89999999999990266, 12.50000000000000000, -5.022947341949754119 ) ) ;
#68674 = CARTESIAN_POINT ( 'NONE',  ( -5.200000000000020606, 12.50000000000000000, 3.983716857408420964 ) ) ;
#68675 = CIRCLE ( 'NONE', #22639, 0.06509327318403745899 ) ;
#68676 = VERTEX_POINT ( 'NONE', #123256 ) ;
#68677 = DIRECTION ( 'NONE',  ( 0.000000000000000000, -0.9999939076577903929, 0.003490651415223739937 ) ) ;
#68678 = EDGE_CURVE ( 'NONE', #62565, #59648, #76533, .T. ) ;
#68679 = CARTESIAN_POINT ( 'NONE',  ( -3.350000000000031619, 2.500000000000000000, -7.188010851410854052 ) ) ;
#68680 = EDGE_CURVE ( 'NONE', #81291, #49092, #30576, .T. ) ;
#68681 = DIRECTION ( 'NONE',  ( -4.274815082592931898E-19, -0.9999939076577903929, -0.003490651415223739937 ) ) ;
#68683 = VERTEX_POINT ( 'NONE', #85885 ) ;
#68682 = DIRECTION ( 'NONE',  ( 0.000000000000000000, 0.000000000000000000, 1.000000000000000000 ) ) ;
#68684 = DIRECTION ( 'NONE',  ( 0.000000000000000000, 0.000000000000000000, 1.000000000000000000 ) ) ;
#68685 = CIRCLE ( 'NONE', #54029, 0.06509327318403745899 ) ;
#68686 = DIRECTION ( 'NONE',  ( 0.000000000000000000, 0.000000000000000000, 1.000000000000000000 ) ) ;
#68687 = ORIENTED_EDGE ( 'NONE', *, *, #52846, .F. ) ;
#68688 = AXIS2_PLACEMENT_3D ( 'NONE', #58419, #48589, #88496 ) ;
#68689 = EDGE_LOOP ( 'NONE', ( #12851, #18348, #29684, #40073 ) ) ;
#68690 = ORIENTED_EDGE ( 'NONE', *, *, #2421, .F. ) ;
#68691 = ORIENTED_EDGE ( 'NONE', *, *, #104752, .T. ) ;
#68692 = CARTESIAN_POINT ( 'NONE',  ( -5.400000000000019895, 2.500000000000000000, 3.537306695894645081 ) ) ;
#68693 = CIRCLE ( 'NONE', #122991, 0.1000000000000002554 ) ;
#68694 = CARTESIAN_POINT ( 'NONE',  ( -12.49999999999995914, 2.500000000000000000, -4.330127018922198978 ) ) ;
#68695 = CIRCLE ( 'NONE', #45727, 0.06509327318403745899 ) ;
#68696 = EDGE_LOOP ( 'NONE', ( #56910, #22823, #108614, #123225 ) ) ;
#68697 = DIRECTION ( 'NONE',  ( -4.274815082592931898E-19, -0.9999939076577903929, -0.003490651415223739937 ) ) ;
#68699 = AXIS2_PLACEMENT_3D ( 'NONE', #93389, #23337, #65187 ) ;
#68698 = CARTESIAN_POINT ( 'NONE',  ( 1.249999999999950262, 12.50000000000000000, 7.188010851410848723 ) ) ;
#68700 = DIRECTION ( 'NONE',  ( 0.000000000000000000, 0.000000000000000000, -1.000000000000000000 ) ) ;
#68701 = CARTESIAN_POINT ( 'NONE',  ( -4.550000000000022915, 2.500000000000000000, 6.395190528383296602 ) ) ;
#68702 = ORIENTED_EDGE ( 'NONE', *, *, #63218, .F. ) ;
#68704 = AXIS2_PLACEMENT_3D ( 'NONE', #17493, #65964, #16200 ) ;
#68703 = AXIS2_PLACEMENT_3D ( 'NONE', #2922, #122685, #83418 ) ;
#68705 = CARTESIAN_POINT ( 'NONE',  ( -10.40000000000000213, 2.500000000000000000, -0.1000000000000022815 ) ) ;
#68706 = ORIENTED_EDGE ( 'NONE', *, *, #12521, .T. ) ;
#68707 = ORIENTED_EDGE ( 'NONE', *, *, #55152, .T. ) ;
#68708 = DIRECTION ( 'NONE',  ( -0.000000000000000000, 1.000000000000000000, -0.000000000000000000 ) ) ;
#68709 = DIRECTION ( 'NONE',  ( 0.000000000000000000, 0.000000000000000000, 1.000000000000000000 ) ) ;
#68710 = FACE_BOUND ( 'NONE', #20429, .T. ) ;
#68711 = DIRECTION ( 'NONE',  ( -0.000000000000000000, 1.000000000000000000, -0.000000000000000000 ) ) ;
#68712 = DIRECTION ( 'NONE',  ( -0.000000000000000000, 1.000000000000000000, -0.000000000000000000 ) ) ;
#68713 = CARTESIAN_POINT ( 'NONE',  ( -0.8000000000000376810, 2.500000000000000000, -4.230127018922201998 ) ) ;
#68714 = EDGE_CURVE ( 'NONE', #114690, #22290, #57747, .T. ) ;
#68715 = AXIS2_PLACEMENT_3D ( 'NONE', #25425, #37215, #97405 ) ;
#68716 = ORIENTED_EDGE ( 'NONE', *, *, #6553, .F. ) ;
#68717 = LINE ( 'NONE', #100126, #19134 ) ;
#68718 = CARTESIAN_POINT ( 'NONE',  ( -12.09999999999999609, 2.500000000000000000, 4.330127018922196314 ) ) ;
#68719 = DIRECTION ( 'NONE',  ( 0.000000000000000000, 0.000000000000000000, 1.000000000000000000 ) ) ;
#68720 = DIRECTION ( 'NONE',  ( 0.000000000000000000, 1.000000000000000000, 0.000000000000000000 ) ) ;
#68721 = EDGE_LOOP ( 'NONE', ( #8104, #61240 ) ) ;
#68722 = ADVANCED_FACE ( 'NONE', ( #37464 ), #99522, .T. ) ;
#68723 = PLANE ( 'NONE',  #11456 ) ;
#68724 = AXIS2_PLACEMENT_3D ( 'NONE', #75279, #115178, #25523 ) ;
#68725 = AXIS2_PLACEMENT_3D ( 'NONE', #93622, #36655, #54975 ) ;
#68726 = CARTESIAN_POINT ( 'NONE',  ( -6.700000000000019718, 2.500000000000000000, -4.230127018922201998 ) ) ;
#68727 = AXIS2_PLACEMENT_3D ( 'NONE', #82341, #120956, #122262 ) ;
#68728 = EDGE_LOOP ( 'NONE', ( #72480, #17896, #61350, #49152 ) ) ;
#68729 = ORIENTED_EDGE ( 'NONE', *, *, #121219, .T. ) ;
#68730 = EDGE_CURVE ( 'NONE', #7606, #64073, #107480, .T. ) ;
#68731 = FACE_OUTER_BOUND ( 'NONE', #58587, .T. ) ;
#68733 = EDGE_CURVE ( 'NONE', #36724, #96060, #59837, .T. ) ;
#68732 = DIRECTION ( 'NONE',  ( -0.000000000000000000, -1.000000000000000000, -0.000000000000000000 ) ) ;
#68734 = FACE_BOUND ( 'NONE', #112741, .T. ) ;
#68735 = CARTESIAN_POINT ( 'NONE',  ( 11.74779829714320378, -2.500000000000001776, -7.682567038344338073 ) ) ;
#68736 = VECTOR ( 'NONE', #64337, 1000.000000000000000 ) ;
#68737 = CIRCLE ( 'NONE', #83425, 0.06509327318403745899 ) ;
#68738 = VECTOR ( 'NONE', #79599, 1000.000000000000000 ) ;
#68739 = ORIENTED_EDGE ( 'NONE', *, *, #124329, .F. ) ;
#68740 = DIRECTION ( 'NONE',  ( 0.000000000000000000, 0.000000000000000000, 1.000000000000000000 ) ) ;
#68741 = VERTEX_POINT ( 'NONE', #106198 ) ;
#68742 = EDGE_LOOP ( 'NONE', ( #23918, #67638 ) ) ;
#68743 = DIRECTION ( 'NONE',  ( 0.000000000000000000, 0.000000000000000000, 1.000000000000000000 ) ) ;
#68744 = EDGE_CURVE ( 'NONE', #86614, #32914, #1300, .T. ) ;
#68745 = CARTESIAN_POINT ( 'NONE',  ( 184.4218750003414016, 0.000000000000000000, 7.564683531250000925 ) ) ;
#68746 = ORIENTED_EDGE ( 'NONE', *, *, #74034, .T. ) ;
#68747 = DIRECTION ( 'NONE',  ( -0.000000000000000000, 1.000000000000000000, -0.000000000000000000 ) ) ;
#68748 = CARTESIAN_POINT ( 'NONE',  ( -2.100000000000033840, 2.500000000000000000, 4.922947341949748257 ) ) ;
#68749 = AXIS2_PLACEMENT_3D ( 'NONE', #59536, #60168, #79787 ) ;
#68750 = PLANE ( 'NONE',  #10993 ) ;
#68751 = DIRECTION ( 'NONE',  ( 0.000000000000000000, -0.9999939076577903929, 0.003490651415223739937 ) ) ;
#68752 = EDGE_LOOP ( 'NONE', ( #32428, #26911 ) ) ;
#68753 = DIRECTION ( 'NONE',  ( -0.000000000000000000, -1.000000000000000000, -0.000000000000000000 ) ) ;
#68754 = CARTESIAN_POINT ( 'NONE',  ( 8.349999999999919709, 2.500000000000000000, -2.065063509461102065 ) ) ;
#68755 = CARTESIAN_POINT ( 'NONE',  ( -2.050000000000033129, 12.50000000000000000, 6.495190528383297135 ) ) ;
#68756 = AXIS2_PLACEMENT_3D ( 'NONE', #90393, #100864, #30226 ) ;
#68757 = FACE_OUTER_BOUND ( 'NONE', #74935, .T. ) ;
#68758 = ORIENTED_EDGE ( 'NONE', *, *, #37457, .F. ) ;
#68759 = ORIENTED_EDGE ( 'NONE', *, *, #15834, .F. ) ;
#68760 = LINE ( 'NONE', #108688, #116157 ) ;
#68761 = ORIENTED_EDGE ( 'NONE', *, *, #70740, .F. ) ;
#68762 = DIRECTION ( 'NONE',  ( 0.000000000000000000, -0.9999939076577903929, 0.003490651415223739937 ) ) ;
#68763 = CARTESIAN_POINT ( 'NONE',  ( 87.50000000000001421, -6.099025433955698183, -4.412011999988000532 ) ) ;
#68764 = EDGE_CURVE ( 'NONE', #95676, #6638, #95734, .T. ) ;
#68765 = CARTESIAN_POINT ( 'NONE',  ( -10.40000000000000213, 2.500000000000000000, -0.5928203230275541635 ) ) ;
#68766 = DIRECTION ( 'NONE',  ( -0.000000000000000000, 1.000000000000000000, -0.000000000000000000 ) ) ;
#68767 = ORIENTED_EDGE ( 'NONE', *, *, #60584, .T. ) ;
#68768 = AXIS2_PLACEMENT_3D ( 'NONE', #84772, #106342, #93951 ) ;
#68769 = DIRECTION ( 'NONE',  ( -0.000000000000000000, 1.000000000000000000, -0.000000000000000000 ) ) ;
#68770 = LINE ( 'NONE', #58963, #14629 ) ;
#68771 = CARTESIAN_POINT ( 'NONE',  ( 10.59999999999990905, 2.500000000000000000, 3.983716857408420076 ) ) ;
#68772 = CARTESIAN_POINT ( 'NONE',  ( 185.0677083336747160, -4.367472073101514418, -7.564683531250002702 ) ) ;
#68773 = CARTESIAN_POINT ( 'NONE',  ( -11.64999999999999680, 12.50000000000000000, 2.165063509461097713 ) ) ;
#68774 = EDGE_CURVE ( 'NONE', #93079, #74476, #41043, .T. ) ;
#68775 = VECTOR ( 'NONE', #63824, 1000.000000000000000 ) ;
#68776 = DIRECTION ( 'NONE',  ( -4.274815082592931898E-19, -0.9999939076577903929, -0.003490651415223739937 ) ) ;
#68777 = EDGE_CURVE ( 'NONE', #78711, #127931, #68198, .T. ) ;
#68779 = ORIENTED_EDGE ( 'NONE', *, *, #117054, .F. ) ;
#68778 = CIRCLE ( 'NONE', #52073, 0.09999999999999982514 ) ;
#68780 = EDGE_LOOP ( 'NONE', ( #38734, #107160, #61740, #7937 ) ) ;
#68781 = DIRECTION ( 'NONE',  ( 0.000000000000000000, 0.000000000000000000, -1.000000000000000000 ) ) ;
#68782 = ORIENTED_EDGE ( 'NONE', *, *, #118786, .T. ) ;
#68783 = DIRECTION ( 'NONE',  ( 0.000000000000000000, 0.000000000000000000, 1.000000000000000000 ) ) ;
#68784 = EDGE_CURVE ( 'NONE', #44544, #2580, #7977, .T. ) ;
#68786 = ORIENTED_EDGE ( 'NONE', *, *, #92089, .F. ) ;
#68785 = EDGE_LOOP ( 'NONE', ( #18210, #118059 ) ) ;
#68787 = EDGE_CURVE ( 'NONE', #94775, #36193, #61955, .T. ) ;
#68788 = ORIENTED_EDGE ( 'NONE', *, *, #100547, .T. ) ;
#68789 = CIRCLE ( 'NONE', #79273, 0.06509327318403745899 ) ;
#68790 = ADVANCED_FACE ( 'NONE', ( #6039 ), #26351, .T. ) ;
#68791 = DIRECTION ( 'NONE',  ( 0.000000000000000000, 0.000000000000000000, 1.000000000000000000 ) ) ;
#68792 = ADVANCED_FACE ( 'NONE', ( #115336 ), #53551, .T. ) ;
#68793 = LINE ( 'NONE', #108713, #12980 ) ;
#68794 = DIRECTION ( 'NONE',  ( 0.000000000000000000, 0.000000000000000000, 1.000000000000000000 ) ) ;
#68797 = EDGE_CURVE ( 'NONE', #48784, #80079, #5498, .T. ) ;
#68796 = CONICAL_SURFACE ( 'NONE', #26945, 0.09999999999999982514, 0.003490658503988666988 ) ;
#68795 = CIRCLE ( 'NONE', #85517, 0.06509327318403745899 ) ;
#68798 = CARTESIAN_POINT ( 'NONE',  ( -5.200000000000025935, 2.500000000000000000, -3.983716857408426293 ) ) ;
#68799 = CARTESIAN_POINT ( 'NONE',  ( 185.8333333333333144, 6.668395609140177704, -3.849999999999998312 ) ) ;
#68800 = LINE ( 'NONE', #108718, #70625 ) ;
#68801 = CARTESIAN_POINT ( 'NONE',  ( -12.09999999999999609, 2.500000000000000000, -3.637306695894647390 ) ) ;
#68802 = AXIS2_PLACEMENT_3D ( 'NONE', #1616, #50108, #30467 ) ;
#68804 = ADVANCED_FACE ( 'NONE', ( #76089 ), #15960, .T. ) ;
#68803 = DIRECTION ( 'NONE',  ( 0.000000000000000000, 0.000000000000000000, 1.000000000000000000 ) ) ;
#68805 = ORIENTED_EDGE ( 'NONE', *, *, #47965, .T. ) ;
#68807 = CIRCLE ( 'NONE', #77217, 0.06509327318403745899 ) ;
#68806 = CIRCLE ( 'NONE', #123195, 0.06509327318403745899 ) ;
#68808 = EDGE_LOOP ( 'NONE', ( #65558, #16371 ) ) ;
#68809 = ORIENTED_EDGE ( 'NONE', *, *, #74650, .F. ) ;
#68810 = CARTESIAN_POINT ( 'NONE',  ( 4.549999999999937650, 2.500000000000000000, 2.165063509461097713 ) ) ;
#68811 = ORIENTED_EDGE ( 'NONE', *, *, #76671, .F. ) ;
#68812 = ORIENTED_EDGE ( 'NONE', *, *, #34477, .T. ) ;
#68813 = CARTESIAN_POINT ( 'NONE',  ( -4.800000000000028244, 2.500000000000000000, -4.083716857408426826 ) ) ;
#68814 = CARTESIAN_POINT ( 'NONE',  ( 2.499999999999983569, 2.500000000000000000, -4.430127018922202176 ) ) ;
#68815 = DIRECTION ( 'NONE',  ( 0.000000000000000000, 1.000000000000000000, 0.000000000000000000 ) ) ;
#68816 = FACE_OUTER_BOUND ( 'NONE', #118751, .T. ) ;
#68818 = AXIS2_PLACEMENT_3D ( 'NONE', #128524, #97734, #66968 ) ;
#68817 = CARTESIAN_POINT ( 'NONE',  ( -10.80000000000000071, 2.500000000000000000, 4.330127018922196314 ) ) ;
#68819 = ORIENTED_EDGE ( 'NONE', *, *, #127672, .T. ) ;
#68820 = EDGE_LOOP ( 'NONE', ( #87518, #27928, #47441, #6720 ) ) ;
#68822 = FACE_OUTER_BOUND ( 'NONE', #43767, .T. ) ;
#68821 = CIRCLE ( 'NONE', #60533, 0.06509327318403745899 ) ;
#68824 = ORIENTED_EDGE ( 'NONE', *, *, #116660, .T. ) ;
#68823 = AXIS2_PLACEMENT_3D ( 'NONE', #92834, #20220, #91535 ) ;
#68825 = DIRECTION ( 'NONE',  ( 0.000000000000000000, -0.9999939076577903929, 0.003490651415223739937 ) ) ;
#68826 = ORIENTED_EDGE ( 'NONE', *, *, #95085, .T. ) ;
#68827 = ORIENTED_EDGE ( 'NONE', *, *, #38307, .T. ) ;
#68829 = CIRCLE ( 'NONE', #27073, 0.06509327318403745899 ) ;
#68828 = CARTESIAN_POINT ( 'NONE',  ( -6.249999999999981348, 2.500000000000000000, 6.395190528383296602 ) ) ;
#68830 = CARTESIAN_POINT ( 'NONE',  ( -1.450000000000036371, 2.500000000000000000, 6.941600689897073018 ) ) ;
#68831 = CIRCLE ( 'NONE', #123226, 0.06509327318403743123 ) ;
#68832 = CARTESIAN_POINT ( 'NONE',  ( 2.699999999999946443, 2.500000000000000000, -3.883716857408426648 ) ) ;
#68833 = ADVANCED_FACE ( 'NONE', ( #35530 ), #7553, .T. ) ;
#68834 = DIRECTION ( 'NONE',  ( -0.000000000000000000, 1.000000000000000000, -0.000000000000000000 ) ) ;
#68835 = CARTESIAN_POINT ( 'NONE',  ( 4.999999999999969802, 2.500000000000000000, 4.330127018922196314 ) ) ;
#68836 = ORIENTED_EDGE ( 'NONE', *, *, #120806, .F. ) ;
#68837 = CARTESIAN_POINT ( 'NONE',  ( -6.250000000000017764, 2.500000000000000000, 7.088010851410848190 ) ) ;
#68838 = FACE_OUTER_BOUND ( 'NONE', #29422, .T. ) ;
#68839 = CARTESIAN_POINT ( 'NONE',  ( -13.54999999999999005, 12.50000000000000000, 2.511473670974877503 ) ) ;
#68840 = DIRECTION ( 'NONE',  ( 0.000000000000000000, 1.000000000000000000, 0.000000000000000000 ) ) ;
#68841 = VECTOR ( 'NONE', #59902, 1000.000000000000000 ) ;
#68843 = ADVANCED_FACE ( 'NONE', ( #46617 ), #26363, .T. ) ;
#68842 = DIRECTION ( 'NONE',  ( 0.000000000000000000, 0.000000000000000000, 1.000000000000000000 ) ) ;
#68844 = AXIS2_PLACEMENT_3D ( 'NONE', #82715, #64343, #72250 ) ;
#68845 = EDGE_LOOP ( 'NONE', ( #66793, #73763 ) ) ;
#68846 = AXIS2_PLACEMENT_3D ( 'NONE', #27027, #17162, #87855 ) ;
#68847 = ORIENTED_EDGE ( 'NONE', *, *, #62911, .F. ) ;
#68848 = CARTESIAN_POINT ( 'NONE',  ( 14.14999999999989733, 2.500000000000000000, 1.472243186433545459 ) ) ;
#68849 = ORIENTED_EDGE ( 'NONE', *, *, #5210, .T. ) ;
#68850 = DIRECTION ( 'NONE',  ( 0.000000000000000000, 1.000000000000000000, 0.000000000000000000 ) ) ;
#68851 = LINE ( 'NONE', #98959, #41858 ) ;
#68852 = AXIS2_PLACEMENT_3D ( 'NONE', #98600, #38440, #8298 ) ;
#68853 = ORIENTED_EDGE ( 'NONE', *, *, #41582, .T. ) ;
#68854 = CARTESIAN_POINT ( 'NONE',  ( 185.7083333333333428, -4.445597072760115509, -7.700000000000001954 ) ) ;
#68855 = DIRECTION ( 'NONE',  ( -0.000000000000000000, 1.000000000000000000, -0.000000000000000000 ) ) ;
#68856 = CARTESIAN_POINT ( 'NONE',  ( -8.950000000000009948, 2.500000000000000000, -6.841600689897072485 ) ) ;
#68857 = CARTESIAN_POINT ( 'NONE',  ( -8.550000000000013145, 2.500000000000000000, -6.741600689897072840 ) ) ;
#68858 = ORIENTED_EDGE ( 'NONE', *, *, #101448, .F. ) ;
#68859 = CARTESIAN_POINT ( 'NONE',  ( -3.750000000000027978, 2.500000000000000000, 7.188010851410848723 ) ) ;
#68860 = ORIENTED_EDGE ( 'NONE', *, *, #111943, .T. ) ;
#68861 = DIRECTION ( 'NONE',  ( -0.000000000000000000, -1.000000000000000000, -0.000000000000000000 ) ) ;
#68862 = CIRCLE ( 'NONE', #22912, 0.06509327318403745899 ) ;
#68863 = FACE_OUTER_BOUND ( 'NONE', #103316, .T. ) ;
#68864 = CARTESIAN_POINT ( 'NONE',  ( 3.949999999999938005, 12.50000000000000000, 6.841600689897072485 ) ) ;
#68865 = EDGE_CURVE ( 'NONE', #30644, #103084, #36818, .T. ) ;
#68866 = ORIENTED_EDGE ( 'NONE', *, *, #49073, .T. ) ;
#68867 = CARTESIAN_POINT ( 'NONE',  ( 13.94999999999989804, 2.500000000000000000, 1.818653347947321475 ) ) ;
#68868 = ORIENTED_EDGE ( 'NONE', *, *, #113293, .F. ) ;
#68870 = AXIS2_PLACEMENT_3D ( 'NONE', #19862, #99714, #1491 ) ;
#68869 = DIRECTION ( 'NONE',  ( 1.000000000000000000, 0.000000000000000000, 0.000000000000000000 ) ) ;
#68871 = DIRECTION ( 'NONE',  ( 0.000000000000000000, -0.9999939076577903929, 0.003490651415223739937 ) ) ;
#68872 = DIRECTION ( 'NONE',  ( 0.000000000000000000, 1.000000000000000000, 0.000000000000000000 ) ) ;
#68873 = ORIENTED_EDGE ( 'NONE', *, *, #98744, .T. ) ;
#68874 = EDGE_CURVE ( 'NONE', #120570, #124699, #70276, .T. ) ;
#68875 = LINE ( 'NONE', #8019, #11264 ) ;
#68876 = CARTESIAN_POINT ( 'NONE',  ( 12.49999999999990585, 12.50000000000000000, -4.957854068765716882 ) ) ;
#68878 = EDGE_CURVE ( 'NONE', #66105, #35393, #24296, .T. ) ;
#68877 = AXIS2_PLACEMENT_3D ( 'NONE', #166, #30315, #826 ) ;
#68879 = ORIENTED_EDGE ( 'NONE', *, *, #125522, .T. ) ;
#68880 = EDGE_CURVE ( 'NONE', #31883, #100718, #108753, .T. ) ;
#68881 = DIRECTION ( 'NONE',  ( 0.000000000000000000, 0.000000000000000000, 1.000000000000000000 ) ) ;
#68882 = EDGE_CURVE ( 'NONE', #13198, #39312, #30671, .T. ) ;
#68883 = ORIENTED_EDGE ( 'NONE', *, *, #10967, .F. ) ;
#68884 = CARTESIAN_POINT ( 'NONE',  ( 2.499999999999947153, 2.500000000000000000, 3.637306695894644726 ) ) ;
#68886 = CIRCLE ( 'NONE', #70955, 0.09999999999999982514 ) ;
#68885 = VECTOR ( 'NONE', #61774, 1000.000000000000000 ) ;
#68887 = EDGE_LOOP ( 'NONE', ( #62423, #27135, #101424, #52166 ) ) ;
#68888 = DIRECTION ( 'NONE',  ( -1.000000000000000000, -0.000000000000000000, -0.000000000000000000 ) ) ;
#68889 = DIRECTION ( 'NONE',  ( 0.000000000000000000, 1.000000000000000000, 0.000000000000000000 ) ) ;
#68890 = EDGE_CURVE ( 'NONE', #46014, #98786, #5580, .T. ) ;
#68891 = ORIENTED_EDGE ( 'NONE', *, *, #49644, .F. ) ;
#68892 = ORIENTED_EDGE ( 'NONE', *, *, #16446, .F. ) ;
#68893 = ADVANCED_FACE ( 'NONE', ( #68838 ), #66143, .T. ) ;
#68894 = DIRECTION ( 'NONE',  ( -4.274815082592931898E-19, -0.9999939076577903929, -0.003490651415223739937 ) ) ;
#68895 = FACE_OUTER_BOUND ( 'NONE', #126146, .T. ) ;
#68896 = VERTEX_POINT ( 'NONE', #21024 ) ;
#68897 = DIRECTION ( 'NONE',  ( 0.000000000000000000, -0.000000000000000000, 1.000000000000000000 ) ) ;
#68898 = CARTESIAN_POINT ( 'NONE',  ( 2.299999999999948752, 12.50000000000000000, 0.3464101615137735735 ) ) ;
#68899 = FACE_OUTER_BOUND ( 'NONE', #62459, .T. ) ;
#68900 = CARTESIAN_POINT ( 'NONE',  ( 104.2422576842260895, 8.047964328330300177, 3.313773385403227412 ) ) ;
#68901 = CONICAL_SURFACE ( 'NONE', #38406, 0.1000000000000000472, 0.003490658503988666988 ) ;
#68902 = CARTESIAN_POINT ( 'NONE',  ( 8.949999999999919353, 12.50000000000000000, 2.511473670974873507 ) ) ;
#68903 = DIRECTION ( 'NONE',  ( 0.000000000000000000, 0.000000000000000000, -1.000000000000000000 ) ) ;
#68904 = DIRECTION ( 'NONE',  ( 0.000000000000000000, 0.000000000000000000, 1.000000000000000000 ) ) ;
#68905 = AXIS2_PLACEMENT_3D ( 'NONE', #82054, #113453, #112172 ) ;
#68906 = CIRCLE ( 'NONE', #54250, 0.09999999999999982514 ) ;
#68907 = EDGE_LOOP ( 'NONE', ( #37960, #84185, #124708, #17683 ) ) ;
#68908 = EDGE_LOOP ( 'NONE', ( #122644, #54350, #72660, #13486 ) ) ;
#68909 = VERTEX_POINT ( 'NONE', #60947 ) ;
#68910 = ORIENTED_EDGE ( 'NONE', *, *, #50875, .T. ) ;
#68911 = DIRECTION ( 'NONE',  ( 0.000000000000000000, 0.000000000000000000, 1.000000000000000000 ) ) ;
#68912 = DIRECTION ( 'NONE',  ( 0.000000000000000000, 1.000000000000000000, 0.000000000000000000 ) ) ;
#68913 = CARTESIAN_POINT ( 'NONE',  ( 12.89999999999989910, 12.50000000000000000, -0.6277270498435167934 ) ) ;
#68914 = ORIENTED_EDGE ( 'NONE', *, *, #17539, .T. ) ;
#68915 = FACE_BOUND ( 'NONE', #28195, .T. ) ;
#68916 = EDGE_LOOP ( 'NONE', ( #95239, #55429, #13224, #100612 ) ) ;
#68917 = CARTESIAN_POINT ( 'NONE',  ( -12.29999999999999716, 2.500000000000000000, -4.083716857408424161 ) ) ;
#68918 = CARTESIAN_POINT ( 'NONE',  ( 8.949999999999919353, 2.500000000000000000, 2.411473670974873862 ) ) ;
#68919 = CIRCLE ( 'NONE', #125073, 0.06509327318403745899 ) ;
#68921 = CIRCLE ( 'NONE', #117017, 0.06509327318403745899 ) ;
#68920 = CIRCLE ( 'NONE', #106295, 0.1000000000000002554 ) ;
#68922 = CARTESIAN_POINT ( 'NONE',  ( -14.14999999999998614, 2.500000000000000000, -2.265063509461099578 ) ) ;
#68923 = DIRECTION ( 'NONE',  ( 0.000000000000000000, 0.000000000000000000, -1.000000000000000000 ) ) ;
#68924 = DIRECTION ( 'NONE',  ( 0.000000000000000000, 0.000000000000000000, 1.000000000000000000 ) ) ;
#68925 = CARTESIAN_POINT ( 'NONE',  ( -2.900000000000029221, 12.50000000000000000, -5.022947341949754119 ) ) ;
#68926 = DIRECTION ( 'NONE',  ( 0.000000000000000000, 0.000000000000000000, 1.000000000000000000 ) ) ;
#68927 = DIRECTION ( 'NONE',  ( 0.000000000000000000, 0.000000000000000000, -1.000000000000000000 ) ) ;
#68928 = DIRECTION ( 'NONE',  ( -0.000000000000000000, 1.000000000000000000, -0.000000000000000000 ) ) ;
#68929 = AXIS2_PLACEMENT_3D ( 'NONE', #103517, #85155, #42688 ) ;
#68930 = DIRECTION ( 'NONE',  ( -0.000000000000000000, 1.000000000000000000, -0.000000000000000000 ) ) ;
#68931 = EDGE_LOOP ( 'NONE', ( #114893, #17936, #70014, #18044 ) ) ;
#68932 = ORIENTED_EDGE ( 'NONE', *, *, #40722, .T. ) ;
#68933 = AXIS2_PLACEMENT_3D ( 'NONE', #11881, #41998, #95609 ) ;
#68934 = ORIENTED_EDGE ( 'NONE', *, *, #45927, .T. ) ;
#68935 = ORIENTED_EDGE ( 'NONE', *, *, #16568, .F. ) ;
#68936 = DIRECTION ( 'NONE',  ( 0.000000000000000000, 0.000000000000000000, 1.000000000000000000 ) ) ;
#68937 = ADVANCED_FACE ( 'NONE', ( #128434 ), #57853, .T. ) ;
#68938 = DIRECTION ( 'NONE',  ( 0.000000000000000000, -0.000000000000000000, 1.000000000000000000 ) ) ;
#68939 = EDGE_CURVE ( 'NONE', #26454, #22443, #22349, .T. ) ;
#68941 = ORIENTED_EDGE ( 'NONE', *, *, #87938, .T. ) ;
#68940 = EDGE_LOOP ( 'NONE', ( #89714, #24745 ) ) ;
#68942 = EDGE_LOOP ( 'NONE', ( #124548, #84861 ) ) ;
#68943 = ADVANCED_FACE ( 'NONE', ( #51150 ), #78790, .T. ) ;
#68944 = CARTESIAN_POINT ( 'NONE',  ( 185.2500000000000000, 9.429780353434619030E-16, -7.700000000000000178 ) ) ;
#68946 = EDGE_CURVE ( 'NONE', #70149, #32170, #95485, .T. ) ;
#68945 = CIRCLE ( 'NONE', #20922, 0.1000000000000002554 ) ;
#68947 = FACE_OUTER_BOUND ( 'NONE', #7244, .T. ) ;
#68948 = CARTESIAN_POINT ( 'NONE',  ( 185.8750000000000000, 8.891194145520236347, 5.444286225454521982E-16 ) ) ;
#68949 = CARTESIAN_POINT ( 'NONE',  ( -4.400000000000025224, 2.500000000000000000, 3.883716857408420431 ) ) ;
#68950 = EDGE_CURVE ( 'NONE', #78428, #80892, #91058, .T. ) ;
#68951 = CARTESIAN_POINT ( 'NONE',  ( -9.150000000000009237, 2.500000000000000000, -2.165063509461101710 ) ) ;
#68952 = AXIS2_PLACEMENT_3D ( 'NONE', #92449, #32916, #13882 ) ;
#68953 = DIRECTION ( 'NONE',  ( 0.000000000000000000, 0.000000000000000000, 1.000000000000000000 ) ) ;
#68954 = CARTESIAN_POINT ( 'NONE',  ( -7.300000000000016698, 12.50000000000000000, -4.676537180435978769 ) ) ;
#68955 = EDGE_LOOP ( 'NONE', ( #37627, #23666, #24104, #24398 ) ) ;
#68957 = EDGE_CURVE ( 'NONE', #58927, #122539, #49535, .T. ) ;
#68956 = CARTESIAN_POINT ( 'NONE',  ( -7.100000000000017408, 2.500000000000000000, -0.6928203230275542523 ) ) ;
#68958 = ORIENTED_EDGE ( 'NONE', *, *, #122653, .T. ) ;
#68959 = ADVANCED_FACE ( 'NONE', ( #71399 ), #9920, .T. ) ;
#68960 = ORIENTED_EDGE ( 'NONE', *, *, #97444, .F. ) ;
#68961 = ORIENTED_EDGE ( 'NONE', *, *, #101108, .F. ) ;
#68962 = CARTESIAN_POINT ( 'NONE',  ( 12.04999999999990834, 2.500000000000000000, 6.595190528383296780 ) ) ;
#68963 = VERTEX_POINT ( 'NONE', #88466 ) ;
#68964 = ORIENTED_EDGE ( 'NONE', *, *, #110729, .F. ) ;
#68965 = EDGE_CURVE ( 'NONE', #5027, #61413, #19072, .T. ) ;
#68966 = DIRECTION ( 'NONE',  ( 0.000000000000000000, -0.9999939076577903929, 0.003490651415223739937 ) ) ;
#68967 = CARTESIAN_POINT ( 'NONE',  ( 3.949999999999938893, 12.50000000000000000, 6.213873640053558134 ) ) ;
#68968 = DIRECTION ( 'NONE',  ( 0.000000000000000000, 1.000000000000000000, 0.000000000000000000 ) ) ;
#68969 = DIRECTION ( 'NONE',  ( 0.000000000000000000, 0.000000000000000000, -1.000000000000000000 ) ) ;
#68970 = FACE_OUTER_BOUND ( 'NONE', #105400, .T. ) ;
#68971 = CIRCLE ( 'NONE', #25059, 0.1000000000000002554 ) ;
#68972 = ORIENTED_EDGE ( 'NONE', *, *, #48216, .T. ) ;
#68973 = CARTESIAN_POINT ( 'NONE',  ( -5.400000000000023448, 2.500000000000000000, -4.330127018922201643 ) ) ;
#68974 = ORIENTED_EDGE ( 'NONE', *, *, #102033, .F. ) ;
#68975 = DIRECTION ( 'NONE',  ( 0.000000000000000000, 0.000000000000000000, 1.000000000000000000 ) ) ;
#68977 = VECTOR ( 'NONE', #90624, 1000.000000000000000 ) ;
#68976 = AXIS2_PLACEMENT_3D ( 'NONE', #80933, #120846, #21351 ) ;
#68978 = ORIENTED_EDGE ( 'NONE', *, *, #74426, .F. ) ;
#68979 = DIRECTION ( 'NONE',  ( -0.000000000000000000, 1.000000000000000000, -0.000000000000000000 ) ) ;
#68980 = CARTESIAN_POINT ( 'NONE',  ( -15.39999999999997904, 2.500000000000000000, 0.000000000000000000 ) ) ;
#68981 = EDGE_LOOP ( 'NONE', ( #70489, #102427, #23689, #3722 ) ) ;
#68982 = DIRECTION ( 'NONE',  ( 0.000000000000000000, 0.000000000000000000, -1.000000000000000000 ) ) ;
#68983 = DIRECTION ( 'NONE',  ( -4.274815082592931898E-19, -0.9999939076577903929, -0.003490651415223739937 ) ) ;
#68984 = EDGE_LOOP ( 'NONE', ( #7399, #54195, #87544, #67060 ) ) ;
#68986 = CIRCLE ( 'NONE', #18802, 0.06509327318403745899 ) ;
#68985 = VECTOR ( 'NONE', #87820, 1000.000000000000000 ) ;
#68987 = DIRECTION ( 'NONE',  ( 0.000000000000000000, -0.9999939076577903929, 0.003490651415223739937 ) ) ;
#68988 = EDGE_LOOP ( 'NONE', ( #53440, #80710, #35454, #85758 ) ) ;
#68989 = ORIENTED_EDGE ( 'NONE', *, *, #74976, .T. ) ;
#68990 = LINE ( 'NONE', #78839, #37203 ) ;
#68991 = CARTESIAN_POINT ( 'NONE',  ( 7.699999999999925571, 2.500000000000000000, 3.983716857408420076 ) ) ;
#68992 = CARTESIAN_POINT ( 'NONE',  ( 1.699999999999951994, 2.500000000000000000, -0.1000000000000022815 ) ) ;
#68993 = DIRECTION ( 'NONE',  ( -4.274815082592931898E-19, -0.9999939076577903929, -0.003490651415223739937 ) ) ;
#68995 = EDGE_CURVE ( 'NONE', #3294, #18103, #70356, .T. ) ;
#68994 = LINE ( 'NONE', #120684, #108539 ) ;
#68996 = EDGE_LOOP ( 'NONE', ( #127458, #19144, #9971, #41631 ) ) ;
#68997 = DIRECTION ( 'NONE',  ( 0.000000000000000000, 0.000000000000000000, -1.000000000000000000 ) ) ;
#68998 = ORIENTED_EDGE ( 'NONE', *, *, #91826, .T. ) ;
#68999 = CARTESIAN_POINT ( 'NONE',  ( -7.300000000000018474, 12.50000000000000000, 0.4115034346978109769 ) ) ;
#69000 = CARTESIAN_POINT ( 'NONE',  ( 11.04999999999991189, 2.500000000000000000, 6.248780366869521430 ) ) ;
#69001 = CIRCLE ( 'NONE', #83682, 0.09999999999999999167 ) ;
#69002 = ORIENTED_EDGE ( 'NONE', *, *, #90174, .T. ) ;
#69003 = DIRECTION ( 'NONE',  ( -0.000000000000000000, -1.000000000000000000, -0.000000000000000000 ) ) ;
#69004 = CARTESIAN_POINT ( 'NONE',  ( -10.40000000000000213, 2.500000000000000000, 3.637306695894644726 ) ) ;
#69005 = CARTESIAN_POINT ( 'NONE',  ( -8.100000000000010303, 2.500000000000000000, 3.883716857408421319 ) ) ;
#69006 = CARTESIAN_POINT ( 'NONE',  ( -7.050000000000016698, 12.50000000000000000, -2.165063509461101710 ) ) ;
#69007 = DIRECTION ( 'NONE',  ( 0.000000000000000000, 1.000000000000000000, 0.000000000000000000 ) ) ;
#69008 = VERTEX_POINT ( 'NONE', #9280 ) ;
#69009 = AXIS2_PLACEMENT_3D ( 'NONE', #111860, #71272, #22203 ) ;
#69010 = CARTESIAN_POINT ( 'NONE',  ( 5.849999999999932143, 12.50000000000000000, 2.165063509461097713 ) ) ;
#69011 = DIRECTION ( 'NONE',  ( 0.000000000000000000, -0.000000000000000000, 1.000000000000000000 ) ) ;
#69012 = DIRECTION ( 'NONE',  ( 0.000000000000000000, 1.000000000000000000, 0.000000000000000000 ) ) ;
#69013 = CONICAL_SURFACE ( 'NONE', #71085, 0.09999999999999982514, 0.003490658503988666988 ) ;
#69014 = ORIENTED_EDGE ( 'NONE', *, *, #739, .F. ) ;
#69015 = CARTESIAN_POINT ( 'NONE',  ( 11.04999999999991189, 2.500000000000000000, 6.148780366869520897 ) ) ;
#69016 = AXIS2_PLACEMENT_3D ( 'NONE', #45204, #85109, #35380 ) ;
#69017 = AXIS2_PLACEMENT_3D ( 'NONE', #49255, #12368, #109445 ) ;
#69018 = VERTEX_POINT ( 'NONE', #28933 ) ;
#69019 = ORIENTED_EDGE ( 'NONE', *, *, #125890, .F. ) ;
#69020 = DIRECTION ( 'NONE',  ( -0.000000000000000000, 1.000000000000000000, -0.000000000000000000 ) ) ;
#69021 = EDGE_LOOP ( 'NONE', ( #67706, #15746, #98547, #43164 ) ) ;
#69022 = FACE_OUTER_BOUND ( 'NONE', #74100, .T. ) ;
#69023 = DIRECTION ( 'NONE',  ( 0.000000000000000000, 0.000000000000000000, 1.000000000000000000 ) ) ;
#69024 = AXIS2_PLACEMENT_3D ( 'NONE', #30105, #70648, #68709 ) ;
#69025 = VERTEX_POINT ( 'NONE', #129079 ) ;
#69026 = EDGE_CURVE ( 'NONE', #70467, #23771, #39411, .T. ) ;
#69027 = FACE_OUTER_BOUND ( 'NONE', #34474, .T. ) ;
#69029 = ORIENTED_EDGE ( 'NONE', *, *, #127009, .F. ) ;
#69028 = CARTESIAN_POINT ( 'NONE',  ( -12.09999999999999609, 2.500000000000000000, 1.734723475976807094E-15 ) ) ;
#69030 = CONICAL_SURFACE ( 'NONE', #117040, 0.1000000000000000056, 0.003490658503988666988 ) ;
#69031 = DIRECTION ( 'NONE',  ( 0.000000000000000000, 1.000000000000000000, 0.000000000000000000 ) ) ;
#69032 = ADVANCED_FACE ( 'NONE', ( #29560 ), #7647, .T. ) ;
#69033 = CARTESIAN_POINT ( 'NONE',  ( -3.750000000000027534, 2.500000000000000000, 2.757883832488649656 ) ) ;
#69034 = EDGE_CURVE ( 'NONE', #74274, #124700, #40036, .T. ) ;
#69035 = EDGE_LOOP ( 'NONE', ( #12297, #13917 ) ) ;
#69036 = ORIENTED_EDGE ( 'NONE', *, *, #72941, .F. ) ;
#69037 = ORIENTED_EDGE ( 'NONE', *, *, #89742, .T. ) ;
#69038 = CARTESIAN_POINT ( 'NONE',  ( -0.2000000000000339284, 2.500000000000000000, -0.2464101615137759549 ) ) ;
#69039 = CARTESIAN_POINT ( 'NONE',  ( 2.899999999999946620, 2.500000000000000000, -3.737306695894649700 ) ) ;
#69040 = EDGE_CURVE ( 'NONE', #82957, #79548, #24392, .T. ) ;
#69041 = ADVANCED_FACE ( 'NONE', ( #113270 ), #97536, .T. ) ;
#69042 = LINE ( 'NONE', #17349, #29597 ) ;
#69043 = EDGE_CURVE ( 'NONE', #24381, #64833, #65998, .T. ) ;
#69044 = FACE_BOUND ( 'NONE', #62617, .T. ) ;
#69046 = EDGE_CURVE ( 'NONE', #16687, #108686, #128969, .T. ) ;
#69045 = ORIENTED_EDGE ( 'NONE', *, *, #32754, .F. ) ;
#69047 = EDGE_CURVE ( 'NONE', #52849, #81743, #32158, .T. ) ;
#69048 = DIRECTION ( 'NONE',  ( 1.000000000000000000, 0.000000000000000000, 0.000000000000000000 ) ) ;
#69049 = DIRECTION ( 'NONE',  ( 0.000000000000000000, 0.000000000000000000, 1.000000000000000000 ) ) ;
#69050 = EDGE_LOOP ( 'NONE', ( #48327, #46387 ) ) ;
#69051 = CARTESIAN_POINT ( 'NONE',  ( 7.099999999999927702, 2.500000000000000000, -3.537306695894649966 ) ) ;
#69052 = CARTESIAN_POINT ( 'NONE',  ( 17.34779069867720480, 2.317761454549635669, 4.873653559263563473 ) ) ;
#69054 = CARTESIAN_POINT ( 'NONE',  ( 2.049999999999950084, 2.500000000000000000, 2.065063509461097624 ) ) ;
#69053 = CIRCLE ( 'NONE', #23099, 0.09999999999999982514 ) ;
#69055 = DIRECTION ( 'NONE',  ( 0.000000000000000000, 0.000000000000000000, 1.000000000000000000 ) ) ;
#69056 = CARTESIAN_POINT ( 'NONE',  ( 0.3999999999999628852, 12.50000000000000000, -0.6277270498435145729 ) ) ;
#69057 = VECTOR ( 'NONE', #24053, 1000.000000000000000 ) ;
#69058 = ADVANCED_FACE ( 'NONE', ( #72080 ), #83184, .T. ) ;
#69059 = CARTESIAN_POINT ( 'NONE',  ( 2.699999999999945555, 12.50000000000000000, 3.983716857408420076 ) ) ;
#69060 = CARTESIAN_POINT ( 'NONE',  ( 5.599999999999933031, 2.500000000000000000, -0.3464101615137783474 ) ) ;
#69062 = CIRCLE ( 'NONE', #43948, 0.06509327318403745899 ) ;
#69061 = CONICAL_SURFACE ( 'NONE', #33581, 0.1000000000000002554, 0.003490658503988666988 ) ;
#69063 = VERTEX_POINT ( 'NONE', #14415 ) ;
#69064 = ORIENTED_EDGE ( 'NONE', *, *, #23201, .F. ) ;
#69065 = ORIENTED_EDGE ( 'NONE', *, *, #78260, .F. ) ;
#69066 = EDGE_LOOP ( 'NONE', ( #35600, #106891, #8295, #74311 ) ) ;
#69067 = ORIENTED_EDGE ( 'NONE', *, *, #83136, .T. ) ;
#69068 = DIRECTION ( 'NONE',  ( -0.000000000000000000, 1.000000000000000000, -0.000000000000000000 ) ) ;
#69069 = DIRECTION ( 'NONE',  ( 0.000000000000000000, 0.000000000000000000, 1.000000000000000000 ) ) ;
#69070 = ORIENTED_EDGE ( 'NONE', *, *, #128490, .F. ) ;
#69071 = FACE_BOUND ( 'NONE', #59341, .T. ) ;
#69072 = DIRECTION ( 'NONE',  ( 0.000000000000000000, -0.9999939076577903929, 0.003490651415223739937 ) ) ;
#69073 = DIRECTION ( 'NONE',  ( -0.000000000000000000, -1.000000000000000000, -0.000000000000000000 ) ) ;
#69074 = CARTESIAN_POINT ( 'NONE',  ( 13.34999999999989662, 12.50000000000000000, -2.230156782645139391 ) ) ;
#69075 = DIRECTION ( 'NONE',  ( 0.000000000000000000, 1.000000000000000000, 0.000000000000000000 ) ) ;
#69076 = DIRECTION ( 'NONE',  ( 0.000000000000000000, 1.000000000000000000, 0.000000000000000000 ) ) ;
#69077 = DIRECTION ( 'NONE',  ( 0.000000000000000000, 0.000000000000000000, 1.000000000000000000 ) ) ;
#69078 = ORIENTED_EDGE ( 'NONE', *, *, #58600, .T. ) ;
#69079 = ORIENTED_EDGE ( 'NONE', *, *, #120909, .T. ) ;
#69080 = VERTEX_POINT ( 'NONE', #43906 ) ;
#69081 = ORIENTED_EDGE ( 'NONE', *, *, #34631, .T. ) ;
#69082 = EDGE_CURVE ( 'NONE', #40465, #49054, #32816, .T. ) ;
#69083 = CARTESIAN_POINT ( 'NONE',  ( 10.79999999999991367, 12.50000000000000000, -2.385244779468109755E-15 ) ) ;
#69084 = DIRECTION ( 'NONE',  ( 0.000000000000000000, 0.000000000000000000, 1.000000000000000000 ) ) ;
#69085 = ADVANCED_FACE ( 'NONE', ( #53707 ), #51592, .T. ) ;
#69086 = VERTEX_POINT ( 'NONE', #72710 ) ;
#69087 = DIRECTION ( 'NONE',  ( 0.000000000000000000, 0.000000000000000000, 1.000000000000000000 ) ) ;
#69088 = ADVANCED_FACE ( 'NONE', ( #24254 ), #76621, .T. ) ;
#69089 = AXIS2_PLACEMENT_3D ( 'NONE', #52409, #112631, #22959 ) ;
#69090 = CARTESIAN_POINT ( 'NONE',  ( -0.6500000000000403233, 12.50000000000000000, 1.753560074763284016 ) ) ;
#69091 = AXIS2_PLACEMENT_3D ( 'NONE', #77653, #105835, #75721 ) ;
#69092 = EDGE_CURVE ( 'NONE', #39004, #23927, #33445, .T. ) ;
#69093 = FACE_OUTER_BOUND ( 'NONE', #49412, .T. ) ;
#69094 = CARTESIAN_POINT ( 'NONE',  ( 184.5677083336747444, -4.367472073101514418, -7.564683531250002702 ) ) ;
#69095 = CARTESIAN_POINT ( 'NONE',  ( -11.24999999999996270, 2.500000000000000000, 2.165063509461097713 ) ) ;
#69096 = CARTESIAN_POINT ( 'NONE',  ( 106.0514428414850272, 8.500000000000000000, -1.125000000000000222 ) ) ;
#69097 = CARTESIAN_POINT ( 'NONE',  ( -8.150000000000012790, 12.50000000000000000, -2.511473670974877948 ) ) ;
#69098 = EDGE_CURVE ( 'NONE', #36428, #118039, #124730, .T. ) ;
#69099 = ORIENTED_EDGE ( 'NONE', *, *, #6977, .F. ) ;
#69100 = CARTESIAN_POINT ( 'NONE',  ( 8.099999999999921485, 2.500000000000000000, -0.4464101615137783252 ) ) ;
#69101 = CIRCLE ( 'NONE', #85819, 0.06509327318403745899 ) ;
#69102 = ADVANCED_FACE ( 'NONE', ( #54351 ), #9722, .T. ) ;
#69103 = ADVANCED_FACE ( 'NONE', ( #24895 ), #64091, .T. ) ;
#69104 = ORIENTED_EDGE ( 'NONE', *, *, #28583, .T. ) ;
#69105 = EDGE_CURVE ( 'NONE', #93656, #47134, #85013, .T. ) ;
#69106 = ORIENTED_EDGE ( 'NONE', *, *, #33421, .T. ) ;
#69107 = CARTESIAN_POINT ( 'NONE',  ( -8.950000000000011724, 12.50000000000000000, -6.148780366869520897 ) ) ;
#69108 = FACE_OUTER_BOUND ( 'NONE', #62227, .T. ) ;
#69109 = DIRECTION ( 'NONE',  ( 0.000000000000000000, 0.000000000000000000, 1.000000000000000000 ) ) ;
#69110 = ORIENTED_EDGE ( 'NONE', *, *, #2874, .T. ) ;
#69111 = EDGE_CURVE ( 'NONE', #58857, #43682, #110072, .T. ) ;
#69112 = VERTEX_POINT ( 'NONE', #42624 ) ;
#69113 = CIRCLE ( 'NONE', #12581, 0.06509327318403745899 ) ;
#69114 = DIRECTION ( 'NONE',  ( 0.000000000000000000, 0.000000000000000000, 1.000000000000000000 ) ) ;
#69115 = AXIS2_PLACEMENT_3D ( 'NONE', #113803, #44410, #24134 ) ;
#69116 = DIRECTION ( 'NONE',  ( 0.000000000000000000, 0.000000000000000000, 1.000000000000000000 ) ) ;
#69117 = LINE ( 'NONE', #109027, #54485 ) ;
#69118 = ORIENTED_EDGE ( 'NONE', *, *, #86632, .T. ) ;
#69119 = CARTESIAN_POINT ( 'NONE',  ( 6.649999999999930189, 2.500000000000000000, -1.372243186433550033 ) ) ;
#69120 = CIRCLE ( 'NONE', #64995, 0.06509327318403745899 ) ;
#69121 = ORIENTED_EDGE ( 'NONE', *, *, #125363, .T. ) ;
#69122 = CARTESIAN_POINT ( 'NONE',  ( 0.5999999999999555689, 12.50000000000000000, 4.611443907251934426 ) ) ;
#69123 = ORIENTED_EDGE ( 'NONE', *, *, #108410, .T. ) ;
#69124 = CARTESIAN_POINT ( 'NONE',  ( -3.749999999999991118, 2.500000000000000000, 2.165063509461097713 ) ) ;
#69125 = CARTESIAN_POINT ( 'NONE',  ( 1.649999999999951950, 2.500000000000000000, -5.802370205355749988 ) ) ;
#69126 = CONICAL_SURFACE ( 'NONE', #123409, 0.1000000000000002554, 0.003490658503988666988 ) ;
#69127 = DIRECTION ( 'NONE',  ( 0.000000000000000000, -0.9999939076577903929, 0.003490651415223739937 ) ) ;
#69128 = EDGE_CURVE ( 'NONE', #126487, #70798, #13909, .T. ) ;
#69129 = DIRECTION ( 'NONE',  ( -0.000000000000000000, -1.000000000000000000, -0.000000000000000000 ) ) ;
#69130 = ORIENTED_EDGE ( 'NONE', *, *, #117673, .F. ) ;
#69131 = DIRECTION ( 'NONE',  ( -0.000000000000000000, -1.000000000000000000, -0.000000000000000000 ) ) ;
#69132 = VERTEX_POINT ( 'NONE', #22968 ) ;
#69133 = VERTEX_POINT ( 'NONE', #62891 ) ;
#69134 = CARTESIAN_POINT ( 'NONE',  ( -10.85000000000000142, 2.500000000000000000, -2.957883832488649833 ) ) ;
#69135 = CARTESIAN_POINT ( 'NONE',  ( 7.049999999999928768, 2.500000000000000000, -2.265063509461101798 ) ) ;
#69136 = DIRECTION ( 'NONE',  ( -4.274815082592931898E-19, -0.9999939076577903929, -0.003490651415223739937 ) ) ;
#69137 = CARTESIAN_POINT ( 'NONE',  ( -2.300000000000033573, 12.50000000000000000, 0.3464101615137735735 ) ) ;
#69138 = DIRECTION ( 'NONE',  ( 0.000000000000000000, 0.000000000000000000, -1.000000000000000000 ) ) ;
#69139 = DIRECTION ( 'NONE',  ( 0.000000000000000000, 0.000000000000000000, -1.000000000000000000 ) ) ;
#69141 = EDGE_CURVE ( 'NONE', #125929, #18925, #87069, .T. ) ;
#69140 = CARTESIAN_POINT ( 'NONE',  ( 12.49999999999990408, 2.500000000000000000, 5.022947341949748790 ) ) ;
#69142 = PLANE ( 'NONE',  #32377 ) ;
#69143 = DIRECTION ( 'NONE',  ( 0.000000000000000000, 0.000000000000000000, 1.000000000000000000 ) ) ;
#69144 = CIRCLE ( 'NONE', #62898, 0.09999999999999982514 ) ;
#69145 = AXIS2_PLACEMENT_3D ( 'NONE', #33583, #94409, #4727 ) ;
#69146 = COLOUR_RGB ( '', 0.31764706, 0.68627451, 0.89019608) ;
#69147 = ORIENTED_EDGE ( 'NONE', *, *, #70427, .F. ) ;
#69148 = DIRECTION ( 'NONE',  ( 0.000000000000000000, 0.000000000000000000, 1.000000000000000000 ) ) ;
#69149 = CIRCLE ( 'NONE', #37857, 0.06509327318403745899 ) ;
#69150 = ADVANCED_FACE ( 'NONE', ( #45195 ), #1487, .T. ) ;
#69151 = DIRECTION ( 'NONE',  ( 0.000000000000000000, -0.000000000000000000, 1.000000000000000000 ) ) ;
#69152 = CARTESIAN_POINT ( 'NONE',  ( 6.249999999999967137, 2.500000000000000000, -2.165063509461101710 ) ) ;
#69153 = CARTESIAN_POINT ( 'NONE',  ( -11.64999999999999680, 12.50000000000000000, -2.165063509461097713 ) ) ;
#69154 = DIRECTION ( 'NONE',  ( 0.000000000000000000, 0.000000000000000000, -1.000000000000000000 ) ) ;
#69155 = EDGE_LOOP ( 'NONE', ( #121023, #126840, #21228, #44612 ) ) ;
#69156 = CARTESIAN_POINT ( 'NONE',  ( -3.750000000000027534, 12.50000000000000000, -1.472243186433550122 ) ) ;
#69157 = PLANE ( 'NONE',  #97176 ) ;
#69159 = ORIENTED_EDGE ( 'NONE', *, *, #29001, .F. ) ;
#69158 = DIRECTION ( 'NONE',  ( 0.000000000000000000, -0.9999939076577903929, 0.003490651415223739937 ) ) ;
#69160 = VERTEX_POINT ( 'NONE', #9601 ) ;
#69161 = LINE ( 'NONE', #36019, #92752 ) ;
#69162 = AXIS2_PLACEMENT_3D ( 'NONE', #76517, #46390, #108548 ) ;
#69163 = ORIENTED_EDGE ( 'NONE', *, *, #97919, .F. ) ;
#69164 = ORIENTED_EDGE ( 'NONE', *, *, #18496, .T. ) ;
#69165 = EDGE_LOOP ( 'NONE', ( #59131, #122514, #2943, #117248 ) ) ;
#69166 = PLANE ( 'NONE',  #65397 ) ;
#69167 = CARTESIAN_POINT ( 'NONE',  ( 6.449999999999930012, 12.50000000000000000, 6.841600689897072485 ) ) ;
#69168 = CARTESIAN_POINT ( 'NONE',  ( 8.349999999999923261, 2.500000000000000000, -6.595190528383302109 ) ) ;
#69169 = DIRECTION ( 'NONE',  ( -0.000000000000000000, -1.000000000000000000, -0.000000000000000000 ) ) ;
#69170 = AXIS2_PLACEMENT_3D ( 'NONE', #34734, #84456, #26183 ) ;
#69171 = ORIENTED_EDGE ( 'NONE', *, *, #89470, .T. ) ;
#69172 = CONICAL_SURFACE ( 'NONE', #12738, 0.1000000000000000472, 0.003490658503988666988 ) ;
#69173 = EDGE_CURVE ( 'NONE', #103444, #39915, #118559, .T. ) ;
#69174 = CARTESIAN_POINT ( 'NONE',  ( -5.400000000000019895, 12.50000000000000000, -0.06509327318403970719 ) ) ;
#69175 = ORIENTED_EDGE ( 'NONE', *, *, #106022, .F. ) ;
#69176 = CARTESIAN_POINT ( 'NONE',  ( -7.100000000000017408, 12.50000000000000000, -0.6928203230275542523 ) ) ;
#69177 = FACE_OUTER_BOUND ( 'NONE', #78482, .T. ) ;
#69178 = DIRECTION ( 'NONE',  ( 0.000000000000000000, 0.000000000000000000, 1.000000000000000000 ) ) ;
#69179 = DIRECTION ( 'NONE',  ( -0.000000000000000000, 1.000000000000000000, -0.000000000000000000 ) ) ;
#69180 = AXIS2_PLACEMENT_3D ( 'NONE', #106688, #57608, #36026 ) ;
#69181 = ORIENTED_EDGE ( 'NONE', *, *, #85327, .T. ) ;
#69182 = EDGE_LOOP ( 'NONE', ( #75568, #36748, #58863, #118588 ) ) ;
#69183 = ORIENTED_EDGE ( 'NONE', *, *, #105921, .T. ) ;
#69184 = ORIENTED_EDGE ( 'NONE', *, *, #34808, .T. ) ;
#69185 = VERTEX_POINT ( 'NONE', #88128 ) ;
#69186 = CARTESIAN_POINT ( 'NONE',  ( 6.449999999999933564, 2.500000000000000000, -6.841600689897078702 ) ) ;
#69187 = DIRECTION ( 'NONE',  ( 0.000000000000000000, 0.000000000000000000, 1.000000000000000000 ) ) ;
#69188 = EDGE_CURVE ( 'NONE', #39393, #96489, #7737, .T. ) ;
#69189 = ADVANCED_FACE ( 'NONE', ( #49543 ), #8299, .T. ) ;
#69190 = CARTESIAN_POINT ( 'NONE',  ( 0.5999999999999551248, 2.500000000000000000, -4.576537180435978236 ) ) ;
#69191 = EDGE_CURVE ( 'NONE', #52455, #104360, #99710, .T. ) ;
#69192 = FACE_BOUND ( 'NONE', #13388, .T. ) ;
#69193 = EDGE_CURVE ( 'NONE', #54491, #72352, #107803, .T. ) ;
#69194 = DIRECTION ( 'NONE',  ( -0.000000000000000000, 1.000000000000000000, -0.000000000000000000 ) ) ;
#69195 = CARTESIAN_POINT ( 'NONE',  ( 0.6499999999999561684, 2.500000000000000000, 1.818653347947321475 ) ) ;
#69196 = DIRECTION ( 'NONE',  ( 0.000000000000000000, 0.000000000000000000, 1.000000000000000000 ) ) ;
#69197 = DIRECTION ( 'NONE',  ( 0.000000000000000000, 0.000000000000000000, 1.000000000000000000 ) ) ;
#69198 = AXIS2_PLACEMENT_3D ( 'NONE', #30737, #97510, #77861 ) ;
#69199 = AXIS2_PLACEMENT_3D ( 'NONE', #92716, #73073, #41061 ) ;
#69200 = DIRECTION ( 'NONE',  ( -0.000000000000000000, -1.000000000000000000, -0.000000000000000000 ) ) ;
#69201 = LINE ( 'NONE', #60700, #105354 ) ;
#69202 = EDGE_CURVE ( 'NONE', #2409, #49329, #32917, .T. ) ;
#69203 = DIRECTION ( 'NONE',  ( -0.000000000000000000, 1.000000000000000000, -0.000000000000000000 ) ) ;
#69204 = AXIS2_PLACEMENT_3D ( 'NONE', #82261, #103179, #90776 ) ;
#69205 = ADVANCED_FACE ( 'NONE', ( #38441 ), #18203, .T. ) ;
#69206 = EDGE_CURVE ( 'NONE', #123253, #19378, #37005, .T. ) ;
#69207 = CARTESIAN_POINT ( 'NONE',  ( 3.000000000000000000, 0.000000000000000000, -5.000000000000004441 ) ) ;
#69208 = ORIENTED_EDGE ( 'NONE', *, *, #80704, .T. ) ;
#69209 = CIRCLE ( 'NONE', #81733, 0.1000000000000002554 ) ;
#69210 = ORIENTED_EDGE ( 'NONE', *, *, #36635, .F. ) ;
#69211 = VERTEX_POINT ( 'NONE', #48902 ) ;
#69212 = ORIENTED_EDGE ( 'NONE', *, *, #113984, .T. ) ;
#69213 = CARTESIAN_POINT ( 'NONE',  ( -11.05000000000000071, 2.500000000000000000, 2.511473670974873507 ) ) ;
#69214 = PRODUCT_RELATED_PRODUCT_CATEGORY ( 'part', '', ( #38744 ) ) ;
#69215 = DIRECTION ( 'NONE',  ( 0.000000000000000000, 0.000000000000000000, 1.000000000000000000 ) ) ;
#69216 = FACE_BOUND ( 'NONE', #64177, .T. ) ;
#69217 = CARTESIAN_POINT ( 'NONE',  ( 9.799999999999918998, 12.50000000000000000, -0.4115034346978156399 ) ) ;
#69218 = ORIENTED_EDGE ( 'NONE', *, *, #19227, .F. ) ;
#69219 = LINE ( 'NONE', #31898, #4928 ) ;
#69220 = DIRECTION ( 'NONE',  ( 0.000000000000000000, 0.000000000000000000, 1.000000000000000000 ) ) ;
#69221 = CARTESIAN_POINT ( 'NONE',  ( 7.099999999999928590, 2.500000000000000000, -5.022947341949754119 ) ) ;
#69222 = DIRECTION ( 'NONE',  ( 0.000000000000000000, -0.9999939076577903929, 0.003490651415223739937 ) ) ;
#69223 = DIRECTION ( 'NONE',  ( 0.000000000000000000, 0.000000000000000000, -1.000000000000000000 ) ) ;
#69224 = ORIENTED_EDGE ( 'NONE', *, *, #56793, .F. ) ;
#69225 = LINE ( 'NONE', #88881, #40818 ) ;
#69226 = ORIENTED_EDGE ( 'NONE', *, *, #59128, .F. ) ;
#69227 = AXIS2_PLACEMENT_3D ( 'NONE', #113903, #12459, #112611 ) ;
#69228 = EDGE_LOOP ( 'NONE', ( #11876, #46083 ) ) ;
#69229 = CIRCLE ( 'NONE', #12793, 0.06509327318403745899 ) ;
#69230 = FACE_OUTER_BOUND ( 'NONE', #60610, .T. ) ;
#69231 = AXIS2_PLACEMENT_3D ( 'NONE', #84087, #83475, #16627 ) ;
#69232 = DIRECTION ( 'NONE',  ( 0.000000000000000000, 1.000000000000000000, 0.000000000000000000 ) ) ;
#69233 = EDGE_LOOP ( 'NONE', ( #27323, #95600, #35599, #15330 ) ) ;
#69234 = CARTESIAN_POINT ( 'NONE',  ( 0.6499999999999543920, 2.500000000000000000, 6.048780366869521252 ) ) ;
#69235 = AXIS2_PLACEMENT_3D ( 'NONE', #597, #18943, #109268 ) ;
#69237 = CONICAL_SURFACE ( 'NONE', #21222, 0.1000000000000000056, 0.003490658503988666988 ) ;
#69236 = LINE ( 'NONE', #99370, #14364 ) ;
#69238 = EDGE_LOOP ( 'NONE', ( #111529, #53813 ) ) ;
#69239 = DIRECTION ( 'NONE',  ( 0.000000000000000000, 0.000000000000000000, 1.000000000000000000 ) ) ;
#69240 = ORIENTED_EDGE ( 'NONE', *, *, #13796, .T. ) ;
#69241 = CARTESIAN_POINT ( 'NONE',  ( -1.050000000000037348, 12.50000000000000000, -6.841600689897078702 ) ) ;
#69242 = ORIENTED_EDGE ( 'NONE', *, *, #55509, .T. ) ;
#69243 = CARTESIAN_POINT ( 'NONE',  ( -7.500000000000011546, 12.50000000000000000, 3.637306695894644726 ) ) ;
#69244 = FACE_BOUND ( 'NONE', #28620, .T. ) ;
#69245 = EDGE_CURVE ( 'NONE', #75910, #18522, #106044, .T. ) ;
#69246 = ORIENTED_EDGE ( 'NONE', *, *, #5622, .T. ) ;
#69248 = EDGE_CURVE ( 'NONE', #81193, #37867, #55861, .T. ) ;
#69247 = CARTESIAN_POINT ( 'NONE',  ( -9.400000000000007461, 12.50000000000000000, -0.3464101615137783474 ) ) ;
#69249 = ORIENTED_EDGE ( 'NONE', *, *, #99955, .T. ) ;
#69250 = DIRECTION ( 'NONE',  ( -4.274815082592931898E-19, -0.9999939076577903929, -0.003490651415223739937 ) ) ;
#69251 = DIRECTION ( 'NONE',  ( -4.274815082592931898E-19, -0.9999939076577903929, -0.003490651415223739937 ) ) ;
#69252 = DIRECTION ( 'NONE',  ( 0.000000000000000000, 0.000000000000000000, -1.000000000000000000 ) ) ;
#69253 = DIRECTION ( 'NONE',  ( 0.000000000000000000, -0.9999939076577903929, 0.003490651415223739937 ) ) ;
#69254 = DIRECTION ( 'NONE',  ( 0.000000000000000000, -0.9999939076577903929, 0.003490651415223739937 ) ) ;
#69255 = ORIENTED_EDGE ( 'NONE', *, *, #36154, .T. ) ;
#69256 = EDGE_CURVE ( 'NONE', #91667, #126381, #58071, .T. ) ;
#69257 = VERTEX_POINT ( 'NONE', #79009 ) ;
#69258 = ORIENTED_EDGE ( 'NONE', *, *, #90524, .T. ) ;
#69259 = FACE_OUTER_BOUND ( 'NONE', #108345, .T. ) ;
#69260 = CARTESIAN_POINT ( 'NONE',  ( 2.699999999999945555, 2.500000000000000000, 3.983716857408420076 ) ) ;
#69261 = DIRECTION ( 'NONE',  ( 0.000000000000000000, 1.000000000000000000, 0.000000000000000000 ) ) ;
#69263 = VERTEX_POINT ( 'NONE', #5245 ) ;
#69262 = ORIENTED_EDGE ( 'NONE', *, *, #101009, .F. ) ;
#69264 = ORIENTED_EDGE ( 'NONE', *, *, #93890, .T. ) ;
#69265 = FACE_OUTER_BOUND ( 'NONE', #71557, .T. ) ;
#69266 = AXIS2_PLACEMENT_3D ( 'NONE', #11687, #51629, #1860 ) ;
#69267 = DIRECTION ( 'NONE',  ( 0.000000000000000000, 0.000000000000000000, -1.000000000000000000 ) ) ;
#69268 = AXIS2_PLACEMENT_3D ( 'NONE', #67023, #16633, #27755 ) ;
#69269 = APPLICATION_PROTOCOL_DEFINITION ( 'draft international standard', 'automotive_design', 1998, #53873 ) ;
#69270 = PLANE ( 'NONE',  #15588 ) ;
#69271 = CARTESIAN_POINT ( 'NONE',  ( -13.09999999999999254, 12.50000000000000000, 0.3464101615137777923 ) ) ;
#69272 = DIRECTION ( 'NONE',  ( 0.000000000000000000, 1.000000000000000000, 0.000000000000000000 ) ) ;
#69273 = LINE ( 'NONE', #116445, #49244 ) ;
#69274 = DIRECTION ( 'NONE',  ( -0.000000000000000000, 1.000000000000000000, -0.000000000000000000 ) ) ;
#69275 = DIRECTION ( 'NONE',  ( 0.000000000000000000, 0.000000000000000000, 1.000000000000000000 ) ) ;
#69276 = ORIENTED_EDGE ( 'NONE', *, *, #90354, .F. ) ;
#69277 = EDGE_LOOP ( 'NONE', ( #58178, #103642, #34880, #116829 ) ) ;
#69278 = CARTESIAN_POINT ( 'NONE',  ( -10.00000000000000533, 2.500000000000000000, 0.5928203230275495006 ) ) ;
#69279 = DIRECTION ( 'NONE',  ( 0.000000000000000000, -0.000000000000000000, 1.000000000000000000 ) ) ;
#69280 = ORIENTED_EDGE ( 'NONE', *, *, #116555, .F. ) ;
#69281 =( BOUNDED_CURVE ( )  B_SPLINE_CURVE ( 2, ( #81308, #2080, #32869, #2728, #72773, #121223, #51852, #11909, #71469, #122519, #123165, #83867, #42694, #91123, #31562, #53136, #91762, #23030, #62946, #63603, #82602, #102855, #93068, #3380, #23670, #43327, #33507, #103524, #13836, #53770, #46517, #74058, #5942, #96912, #26256, #95635, #35436, #56977, #114617, #75336, #6567, #74703, #25584, #125090, #86445, #125713, #56341, #45895, #7229, #47187, #14469, #94327, #65520, #36729, #85164, #66162, #106098, #34143, #34800, #4640, #115233, #85800, #105458, #16396, #15768, #113988, #104784, #123781, #55700, #76641, #24314, #96256, #36070 ),
 .UNSPECIFIED., .F., .F. ) 
 B_SPLINE_CURVE_WITH_KNOTS ( ( 3, 2, 2, 2, 2, 2, 2, 2, 2, 2, 2, 2, 2, 2, 2, 2, 2, 2, 2, 2, 2, 2, 2, 2, 2, 2, 2, 2, 2, 2, 2, 2, 2, 2, 2, 2, 3 ),
 ( 0.000000000000000000, 0.02380952380952380820, 0.04761904761904761640, 0.07142857142857142461, 0.09523809523809523281, 0.1190476190476190410, 0.1428571428571428492, 0.1666666666666666574, 0.1904761904761904656, 0.2142857142857142461, 0.2380952380952380820, 0.2619047619047619180, 0.2857142857142856984, 0.3095238095238095344, 0.3333333333333333148, 0.3571428571428571508, 0.3809523809523809312, 0.4047619047619048227, 0.4285714285714284921, 0.4523809523809523836, 0.4761904761904761640, 0.5000000000000000000, 0.5238095238095238360, 0.5476190476190476719, 0.5714285714285713969, 0.5952380952380952328, 0.6190476190476190688, 0.6428571428571430157, 0.6666666666666666297, 0.6904761904761903546, 0.7142857142857143016, 0.7380952380952381375, 0.7619047619047618625, 0.7857142857142856984, 0.8095238095238096454, 0.8333333333333333703, 0.8350034827724532871 ),
 .UNSPECIFIED. ) 
 CURVE ( )  GEOMETRIC_REPRESENTATION_ITEM ( )  RATIONAL_B_SPLINE_CURVE ( ( 1.000000000000000000, 0.8660254037844387076, 1.000000000000000000, 0.8660254037844387076, 1.000000000000000000, 0.8660254037844387076, 1.000000000000000000, 0.8660254037844387076, 1.000000000000000000, 0.8660254037844387076, 1.000000000000000000, 0.8660254037844387076, 1.000000000000000000, 0.8660254037844387076, 1.000000000000000000, 0.8660254037844387076, 1.000000000000000000, 0.8660254037844387076, 1.000000000000000000, 0.8660254037844387076, 1.000000000000000000, 0.8660254037844387076, 1.000000000000000000, 0.8660254037844387076, 1.000000000000000000, 0.8660254037844387076, 1.000000000000000000, 0.8660254037844387076, 1.000000000000000000, 0.8660254037844387076, 1.000000000000000000, 0.8660254037844387076, 1.000000000000000000, 0.8660254037844387076, 1.000000000000000000, 0.8660254037844387076, 1.000000000000000000, 0.8660254037844387076, 1.000000000000000000, 0.8660254037844387076, 1.000000000000000000, 0.8660254037844387076, 1.000000000000000000, 0.8660254037844387076, 1.000000000000000000, 0.8660254037844387076, 1.000000000000000000, 0.8660254037844387076, 1.000000000000000000, 0.8660254037844387076, 1.000000000000000000, 0.8660254037844387076, 1.000000000000000000, 0.8660254037844387076, 1.000000000000000000, 0.8660254037844387076, 1.000000000000000000, 0.8660254037844387076, 1.000000000000000000, 0.8660254037844387076, 1.000000000000000000, 0.8660254037844387076, 1.000000000000000000, 0.8660254037844387076, 1.000000000000000000, 0.8660254037844387076, 1.000000000000000000, 0.8660254037844387076, 1.000000000000000000, 0.8660254037844387076, 1.000000000000000000, 0.9906021809375190612, 0.9825228059028749961 ) ) 
 REPRESENTATION_ITEM ( '' )  );
#69282 = VERTEX_POINT ( 'NONE', #65452 ) ;
#69283 = CARTESIAN_POINT ( 'NONE',  ( 186.8593750003414016, 0.000000000000000000, 7.564683531250000925 ) ) ;
#69284 = CARTESIAN_POINT ( 'NONE',  ( 11.64999999999990266, 2.500000000000000000, -6.595190528383302109 ) ) ;
#69285 = DIRECTION ( 'NONE',  ( 0.000000000000000000, 0.000000000000000000, 1.000000000000000000 ) ) ;
#69286 = CONICAL_SURFACE ( 'NONE', #246, 0.09999999999999982514, 0.003490658503988666988 ) ;
#69287 = CARTESIAN_POINT ( 'NONE',  ( -4.600000000000025402, 12.50000000000000000, 0.06509327318403504425 ) ) ;
#69288 = PRODUCT_DEFINITION_FORMATION_WITH_SPECIFIED_SOURCE ( 'ANY', '', #7300, .NOT_KNOWN. ) ;
#69289 = CIRCLE ( 'NONE', #100596, 0.06509327318403745899 ) ;
#69290 = CARTESIAN_POINT ( 'NONE',  ( 129.5000000000000000, -1.500000000000000000, 0.000000000000000000 ) ) ;
#69291 = EDGE_CURVE ( 'NONE', #109689, #70723, #11956, .T. ) ;
#69292 = CARTESIAN_POINT ( 'NONE',  ( -13.14999999999999147, 12.50000000000000000, 1.818653347947325472 ) ) ;
#69293 = CIRCLE ( 'NONE', #77610, 0.06509327318403745899 ) ;
#69294 = CARTESIAN_POINT ( 'NONE',  ( 2.049999999999950084, 2.500000000000000000, 2.165063509461097713 ) ) ;
#69295 = TOROIDAL_SURFACE ( 'NONE', #6574, 4.000000000000000000, 1.000000000000000000 ) ;
#69296 = DIRECTION ( 'NONE',  ( 0.000000000000000000, 0.000000000000000000, 1.000000000000000000 ) ) ;
#69297 = ORIENTED_EDGE ( 'NONE', *, *, #23426, .F. ) ;
#69298 = CIRCLE ( 'NONE', #106957, 0.1000000000000002554 ) ;
#69299 = CONICAL_SURFACE ( 'NONE', #56766, 0.1000000000000002554, 0.003490658503988666988 ) ;
#69300 = ORIENTED_EDGE ( 'NONE', *, *, #42508, .T. ) ;
#69301 = EDGE_CURVE ( 'NONE', #37406, #72308, #16134, .T. ) ;
#69302 = ORIENTED_EDGE ( 'NONE', *, *, #52766, .T. ) ;
#69304 = ORIENTED_EDGE ( 'NONE', *, *, #34651, .F. ) ;
#69303 = EDGE_CURVE ( 'NONE', #25426, #116569, #29258, .T. ) ;
#69305 = CARTESIAN_POINT ( 'NONE',  ( -1.850000000000033840, 12.50000000000000000, 6.841600689897072485 ) ) ;
#69306 = DIRECTION ( 'NONE',  ( 0.000000000000000000, 0.000000000000000000, 1.000000000000000000 ) ) ;
#69307 = ORIENTED_EDGE ( 'NONE', *, *, #46970, .F. ) ;
#69308 = FACE_OUTER_BOUND ( 'NONE', #98312, .T. ) ;
#69309 = CARTESIAN_POINT ( 'NONE',  ( 7.699999999999923794, 2.500000000000000000, 4.676537180435972552 ) ) ;
#69310 = CARTESIAN_POINT ( 'NONE',  ( -1.050000000000037792, 12.50000000000000000, 6.148780366869520009 ) ) ;
#69312 = EDGE_LOOP ( 'NONE', ( #102826, #104072 ) ) ;
#69311 = CARTESIAN_POINT ( 'NONE',  ( 15.39999999999989200, 12.50000000000000000, -0.6277270498435167934 ) ) ;
#69313 = EDGE_CURVE ( 'NONE', #1853, #51752, #78359, .T. ) ;
#69314 = CARTESIAN_POINT ( 'NONE',  ( -0.4000000000000331624, 2.500000000000000000, -0.6928203230275519209 ) ) ;
#69315 = DIRECTION ( 'NONE',  ( 0.000000000000000000, -0.9999939076577903929, 0.003490651415223739937 ) ) ;
#69316 = VERTEX_POINT ( 'NONE', #47605 ) ;
#69317 = VERTEX_POINT ( 'NONE', #87499 ) ;
#69318 = ORIENTED_EDGE ( 'NONE', *, *, #97705, .F. ) ;
#69319 = CIRCLE ( 'NONE', #14920, 0.1000000000000002554 ) ;
#69320 = EDGE_LOOP ( 'NONE', ( #28819, #128673 ) ) ;
#69321 = CARTESIAN_POINT ( 'NONE',  ( 2.500000000000002220, -1.500000000000000000, 10.00000000000000178 ) ) ;
#69322 = AXIS2_PLACEMENT_3D ( 'NONE', #56102, #37133, #77047 ) ;
#69323 = CONICAL_SURFACE ( 'NONE', #79803, 0.1000000000000002554, 0.003490658503988666988 ) ;
#69324 = B_SPLINE_CURVE_WITH_KNOTS ( 'NONE', 3,
 ( #110967, #53367, #62547, #1666, #41632, #72998, #91993, #121442, #90707, #80896, #31791, #31161, #120809, #63176, #61252, #2303, #112919, #12768, #23240, #123379 ),
 .UNSPECIFIED., .F., .F.,
 ( 4, 2, 2, 2, 2, 2, 2, 2, 2, 4 ),
 ( 0.000000000000000000, 0.0008832438798941733915, 0.001766487759788346783, 0.002649731639682520283, 0.003532975519576693566, 0.005299463279365040566, 0.007065951039153387132, 0.008832438798941733699, 0.01059892655873008287, 0.01413190207830678294 ),
 .UNSPECIFIED. ) ;
#69325 = LINE ( 'NONE', #19603, #48733 ) ;
#69326 = CARTESIAN_POINT ( 'NONE',  ( -10.65000000000000391, 2.500000000000000000, -2.411473670974874306 ) ) ;
#69327 = AXIS2_PLACEMENT_3D ( 'NONE', #30095, #20253, #51021 ) ;
#69329 = EDGE_CURVE ( 'NONE', #107678, #515, #108436, .T. ) ;
#69328 = CONICAL_SURFACE ( 'NONE', #58890, 0.1000000000000000472, 0.003490658503988666988 ) ;
#69331 = VERTEX_POINT ( 'NONE', #52740 ) ;
#69330 = CIRCLE ( 'NONE', #21316, 0.06509327318403745899 ) ;
#69332 = CARTESIAN_POINT ( 'NONE',  ( 0.7999999999999553024, 2.500000000000000000, -4.230127018922201998 ) ) ;
#69333 = CARTESIAN_POINT ( 'NONE',  ( -6.505213034913026604E-15, 2.500000000000000000, 4.330127018922196314 ) ) ;
#69334 = VECTOR ( 'NONE', #42816, 1000.000000000000000 ) ;
#69335 = CARTESIAN_POINT ( 'NONE',  ( -6.050000000000022027, 12.50000000000000000, -6.148780366869526226 ) ) ;
#69336 = DIRECTION ( 'NONE',  ( 0.000000000000000000, 1.000000000000000000, 0.000000000000000000 ) ) ;
#69337 = CONICAL_SURFACE ( 'NONE', #88196, 0.1000000000000002554, 0.003490658503988666988 ) ;
#69338 = ADVANCED_FACE ( 'NONE', ( #70457 ), #92674, .T. ) ;
#69339 = ORIENTED_EDGE ( 'NONE', *, *, #91472, .F. ) ;
#69340 = CARTESIAN_POINT ( 'NONE',  ( 1.449999999999951328, 2.500000000000000000, 2.611473670974873151 ) ) ;
#69341 = ORIENTED_EDGE ( 'NONE', *, *, #73326, .F. ) ;
#69342 = ORIENTED_EDGE ( 'NONE', *, *, #51749, .F. ) ;
#69343 = CARTESIAN_POINT ( 'NONE',  ( 4.599999999999940137, 2.500000000000000000, -4.330127018922201643 ) ) ;
#69344 = ADVANCED_FACE ( 'NONE', ( #62582 ), #116400, .T. ) ;
#69345 = ADVANCED_FACE ( 'NONE', ( #101851 ), #85107, .T. ) ;
#69346 = LINE ( 'NONE', #107990, #35597 ) ;
#69347 = EDGE_CURVE ( 'NONE', #76682, #56667, #49630, .T. ) ;
#69348 = FACE_BOUND ( 'NONE', #56054, .T. ) ;
#69349 = ADVANCED_FACE ( 'NONE', ( #3012 ), #92026, .T. ) ;
#69350 = DIRECTION ( 'NONE',  ( 0.000000000000000000, 0.000000000000000000, -1.000000000000000000 ) ) ;
#69351 = LINE ( 'NONE', #100741, #21458 ) ;
#69352 = CARTESIAN_POINT ( 'NONE',  ( 12.09999999999990550, 2.500000000000000000, -4.330127018922201643 ) ) ;
#69353 = EDGE_CURVE ( 'NONE', #80440, #86996, #28691, .T. ) ;
#69354 = VERTEX_POINT ( 'NONE', #51472 ) ;
#69355 = CARTESIAN_POINT ( 'NONE',  ( -1.250000000000035749, 12.50000000000000000, -2.922977105672691422 ) ) ;
#69356 = FACE_OUTER_BOUND ( 'NONE', #73168, .T. ) ;
#69357 = ADVANCED_FACE ( 'NONE', ( #109743 ), #100553, .T. ) ;
#69358 = DIRECTION ( 'NONE',  ( -0.000000000000000000, -1.000000000000000000, -0.000000000000000000 ) ) ;
#69359 = CARTESIAN_POINT ( 'NONE',  ( 186.3645833340161175, -6.668395609140180369, 3.849999999999994760 ) ) ;
#69360 = ORIENTED_EDGE ( 'NONE', *, *, #53263, .F. ) ;
#69361 = CONICAL_SURFACE ( 'NONE', #113279, 0.1000000000000002554, 0.003490658503988666988 ) ;
#69362 = DIRECTION ( 'NONE',  ( 0.000000000000000000, 1.000000000000000000, 0.000000000000000000 ) ) ;
#69363 = EDGE_CURVE ( 'NONE', #17965, #7615, #60012, .T. ) ;
#69364 = ADVANCED_FACE ( 'NONE', ( #40369 ), #22452, .T. ) ;
#69365 = DIRECTION ( 'NONE',  ( -0.000000000000000000, -1.000000000000000000, -0.000000000000000000 ) ) ;
#69366 = VERTEX_POINT ( 'NONE', #101210 ) ;
#69367 = VERTEX_POINT ( 'NONE', #91380 ) ;
#69368 = FACE_OUTER_BOUND ( 'NONE', #117124, .T. ) ;
#69369 = EDGE_CURVE ( 'NONE', #96946, #17252, #103902, .T. ) ;
#69370 = DIRECTION ( 'NONE',  ( -0.000000000000000000, 1.000000000000000000, -0.000000000000000000 ) ) ;
#69371 = FACE_BOUND ( 'NONE', #111791, .T. ) ;
#69373 = EDGE_CURVE ( 'NONE', #38962, #36641, #82985, .T. ) ;
#69372 = CONICAL_SURFACE ( 'NONE', #52651, 0.1000000000000000472, 0.003490658503988666988 ) ;
#69374 = CARTESIAN_POINT ( 'NONE',  ( 12.09999999999990550, 2.500000000000000000, -3.537306695894649966 ) ) ;
#69375 = CIRCLE ( 'NONE', #21354, 0.06509327318403745899 ) ;
#69376 = CIRCLE ( 'NONE', #90293, 0.1000000000000002554 ) ;
#69378 = LINE ( 'NONE', #109306, #117577 ) ;
#69377 = CIRCLE ( 'NONE', #42298, 0.1000000000000002554 ) ;
#69379 = CIRCLE ( 'NONE', #115331, 7.700000000000000178 ) ;
#69380 = ORIENTED_EDGE ( 'NONE', *, *, #98470, .T. ) ;
#69381 = CARTESIAN_POINT ( 'NONE',  ( -5.450000000000023270, 2.500000000000000000, -6.495190528383302464 ) ) ;
#69382 = CARTESIAN_POINT ( 'NONE',  ( 184.4583333333333428, 4.445597072760117285, 7.699999999999999289 ) ) ;
#69383 = ORIENTED_EDGE ( 'NONE', *, *, #56164, .F. ) ;
#69385 = CARTESIAN_POINT ( 'NONE',  ( 8.149999999999920419, 2.500000000000000000, 6.941600689897073018 ) ) ;
#69384 = VECTOR ( 'NONE', #71117, 1000.000000000000000 ) ;
#69386 = DIRECTION ( 'NONE',  ( 0.000000000000000000, 1.000000000000000000, 0.000000000000000000 ) ) ;
#69387 = AXIS2_PLACEMENT_3D ( 'NONE', #123302, #13333, #73545 ) ;
#69388 = AXIS2_PLACEMENT_3D ( 'NONE', #106248, #76794, #55224 ) ;
#69389 = AXIS2_PLACEMENT_3D ( 'NONE', #35496, #103592, #34207 ) ;
#69390 = AXIS2_PLACEMENT_3D ( 'NONE', #56038, #28531, #47528 ) ;
#69391 = CARTESIAN_POINT ( 'NONE',  ( 8.749999999999953815, 12.50000000000000000, -2.230156782645139391 ) ) ;
#69392 = CARTESIAN_POINT ( 'NONE',  ( 12.09999999999990195, 2.500000000000000000, 0.09999999999999772959 ) ) ;
#69393 = VECTOR ( 'NONE', #123304, 1000.000000000000000 ) ;
#69394 = VERTEX_POINT ( 'NONE', #42289 ) ;
#69395 = DIRECTION ( 'NONE',  ( -0.000000000000000000, 1.000000000000000000, -0.000000000000000000 ) ) ;
#69396 = CARTESIAN_POINT ( 'NONE',  ( -10.65000000000000213, 12.50000000000000000, 6.906693963081109722 ) ) ;
#69397 = DIRECTION ( 'NONE',  ( 0.000000000000000000, 1.000000000000000000, 0.000000000000000000 ) ) ;
#69398 = VERTEX_POINT ( 'NONE', #90078 ) ;
#69399 = ORIENTED_EDGE ( 'NONE', *, *, #128901, .F. ) ;
#69400 = CARTESIAN_POINT ( 'NONE',  ( 17.46224679592473805, 2.499999999999843237, 5.244174652589637553 ) ) ;
#69401 = ORIENTED_EDGE ( 'NONE', *, *, #22622, .T. ) ;
#69402 = CARTESIAN_POINT ( 'NONE',  ( 11.69999999999990870, 2.500000000000000000, -4.230127018922201998 ) ) ;
#69403 = CARTESIAN_POINT ( 'NONE',  ( 17.50000000000000000, -2.499999999999999556, 1.333333333333338144 ) ) ;
#69404 = EDGE_CURVE ( 'NONE', #84934, #40034, #70452, .T. ) ;
#69405 = CARTESIAN_POINT ( 'NONE',  ( -7.950000000000016165, 12.50000000000000000, -6.430097255199259010 ) ) ;
#69406 = ORIENTED_EDGE ( 'NONE', *, *, #34902, .F. ) ;
#69408 = ADVANCED_FACE ( 'NONE', ( #120844 ), #93437, .T. ) ;
#69407 = FACE_OUTER_BOUND ( 'NONE', #40957, .T. ) ;
#69409 = DIRECTION ( 'NONE',  ( -0.000000000000000000, 1.000000000000000000, -0.000000000000000000 ) ) ;
#69410 = CARTESIAN_POINT ( 'NONE',  ( 8.949999999999915801, 2.500000000000000000, 6.941600689897073018 ) ) ;
#69411 = CARTESIAN_POINT ( 'NONE',  ( 185.7760416670080588, 6.551208109652274736, 3.782341765625001351 ) ) ;
#69412 = DIRECTION ( 'NONE',  ( 0.000000000000000000, 0.000000000000000000, 1.000000000000000000 ) ) ;
#69413 = DIRECTION ( 'NONE',  ( 0.000000000000000000, 0.000000000000000000, -1.000000000000000000 ) ) ;
#69414 = ORIENTED_EDGE ( 'NONE', *, *, #20613, .F. ) ;
#69415 = ORIENTED_EDGE ( 'NONE', *, *, #2414, .T. ) ;
#69416 = CARTESIAN_POINT ( 'NONE',  ( 9.999999999999914735, 2.500000000000000000, 0.5928203230275495006 ) ) ;
#69417 = VERTEX_POINT ( 'NONE', #120207 ) ;
#69418 = AXIS2_PLACEMENT_3D ( 'NONE', #35739, #76952, #16070 ) ;
#69419 = CARTESIAN_POINT ( 'NONE',  ( 106.2064113537864927, 6.122648159495343911, 4.670050787261943448 ) ) ;
#69420 = AXIS2_PLACEMENT_3D ( 'NONE', #119811, #30159, #10489 ) ;
#69422 = VERTEX_POINT ( 'NONE', #42964 ) ;
#69421 = EDGE_LOOP ( 'NONE', ( #19929, #63558, #36350, #22746 ) ) ;
#69423 = VERTEX_POINT ( 'NONE', #61288 ) ;
#69424 = CARTESIAN_POINT ( 'NONE',  ( 0.6499999999999561684, 12.50000000000000000, -1.818653347947325916 ) ) ;
#69425 = DIRECTION ( 'NONE',  ( 0.000000000000000000, 0.000000000000000000, 1.000000000000000000 ) ) ;
#69426 = AXIS2_PLACEMENT_3D ( 'NONE', #32371, #92534, #37804 ) ;
#69428 = FACE_OUTER_BOUND ( 'NONE', #82003, .T. ) ;
#69427 = AXIS2_PLACEMENT_3D ( 'NONE', #75271, #115172, #94920 ) ;
#69429 = AXIS2_PLACEMENT_3D ( 'NONE', #1335, #20344, #70090 ) ;
#69430 =( NAMED_UNIT ( * ) SI_UNIT ( $, .STERADIAN. ) SOLID_ANGLE_UNIT ( ) );
#69431 = DIRECTION ( 'NONE',  ( 0.000000000000000000, -0.000000000000000000, 1.000000000000000000 ) ) ;
#69432 = CARTESIAN_POINT ( 'NONE',  ( 5.599999999999934808, 2.500000000000000000, -3.883716857408426648 ) ) ;
#69433 = CARTESIAN_POINT ( 'NONE',  ( -4.251083420886005162E-14, 12.50000000000000000, -3.702399969078687292 ) ) ;
#69434 = CIRCLE ( 'NONE', #79909, 0.1000000000000002554 ) ;
#69435 = DIRECTION ( 'NONE',  ( -0.000000000000000000, 1.000000000000000000, 1.846105847067148022E-16 ) ) ;
#69436 = DIRECTION ( 'NONE',  ( 0.000000000000000000, 0.000000000000000000, 1.000000000000000000 ) ) ;
#69437 = AXIS2_PLACEMENT_3D ( 'NONE', #92522, #4128, #74180 ) ;
#69438 = DIRECTION ( 'NONE',  ( 0.000000000000000000, 0.000000000000000000, -1.000000000000000000 ) ) ;
#69440 = VERTEX_POINT ( 'NONE', #82866 ) ;
#69439 = CIRCLE ( 'NONE', #33948, 0.06509327318403745899 ) ;
#69441 = ORIENTED_EDGE ( 'NONE', *, *, #78854, .T. ) ;
#69442 = CARTESIAN_POINT ( 'NONE',  ( 176.5000000000000000, 0.000000000000000000, 0.000000000000000000 ) ) ;
#69443 = VERTEX_POINT ( 'NONE', #50193 ) ;
#69444 = ORIENTED_EDGE ( 'NONE', *, *, #43513, .F. ) ;
#69445 = DIRECTION ( 'NONE',  ( -0.000000000000000000, 1.000000000000000000, -0.000000000000000000 ) ) ;
#69446 = EDGE_CURVE ( 'NONE', #102305, #101973, #64180, .T. ) ;
#69447 = CARTESIAN_POINT ( 'NONE',  ( 186.7500000000000000, 9.429780353434619030E-16, -7.700000000000000178 ) ) ;
#69448 = DIRECTION ( 'NONE',  ( 0.000000000000000000, 0.000000000000000000, 1.000000000000000000 ) ) ;
#69449 = DIRECTION ( 'NONE',  ( -0.000000000000000000, -1.000000000000000000, -0.000000000000000000 ) ) ;
#69450 = DIRECTION ( 'NONE',  ( 0.000000000000000000, 0.000000000000000000, 1.000000000000000000 ) ) ;
#69451 = VERTEX_POINT ( 'NONE', #104422 ) ;
#69452 = VECTOR ( 'NONE', #125983, 1000.000000000000000 ) ;
#69453 = VERTEX_POINT ( 'NONE', #25204 ) ;
#69454 = DIRECTION ( 'NONE',  ( 0.000000000000000000, 1.000000000000000000, 0.000000000000000000 ) ) ;
#69455 = ORIENTED_EDGE ( 'NONE', *, *, #98475, .F. ) ;
#69456 = CARTESIAN_POINT ( 'NONE',  ( 12.29999999999990301, 12.50000000000000000, -0.4115034346978156399 ) ) ;
#69457 = ORIENTED_EDGE ( 'NONE', *, *, #125823, .F. ) ;
#69458 = ADVANCED_FACE ( 'NONE', ( #73032 ), #39175, .T. ) ;
#69459 = EDGE_CURVE ( 'NONE', #54631, #1406, #44207, .T. ) ;
#69460 = EDGE_LOOP ( 'NONE', ( #124158, #108848 ) ) ;
#69461 = AXIS2_PLACEMENT_3D ( 'NONE', #96546, #36382, #126015 ) ;
#69462 = DIRECTION ( 'NONE',  ( 0.000000000000000000, 1.000000000000000000, 0.000000000000000000 ) ) ;
#69463 = CARTESIAN_POINT ( 'NONE',  ( 13.09999999999990195, 2.500000000000000000, 3.983716857408420076 ) ) ;
#69464 = CIRCLE ( 'NONE', #13014, 0.06509327318403745899 ) ;
#69465 = CIRCLE ( 'NONE', #56928, 0.1000000000000002554 ) ;
#69466 = CARTESIAN_POINT ( 'NONE',  ( -5.000000000000022204, 2.500000000000000000, -0.6928203230275541413 ) ) ;
#69467 = AXIS2_PLACEMENT_3D ( 'NONE', #21862, #98449, #59866 ) ;
#69468 = DIRECTION ( 'NONE',  ( -4.274815082592931898E-19, -0.9999939076577903929, -0.003490651415223739937 ) ) ;
#69469 = FACE_OUTER_BOUND ( 'NONE', #79040, .T. ) ;
#69470 = ORIENTED_EDGE ( 'NONE', *, *, #5535, .T. ) ;
#69471 = CARTESIAN_POINT ( 'NONE',  ( -8.150000000000012790, 12.50000000000000000, 2.576566944158910744 ) ) ;
#69472 = CARTESIAN_POINT ( 'NONE',  ( 5.649999999999934630, 2.500000000000000000, -1.818653347947325916 ) ) ;
#69473 = EDGE_CURVE ( 'NONE', #25044, #75922, #1296, .T. ) ;
#69474 = LINE ( 'NONE', #49227, #1886 ) ;
#69475 = CARTESIAN_POINT ( 'NONE',  ( 8.349999999999923261, 2.500000000000000000, 2.265063509461097357 ) ) ;
#69476 = VECTOR ( 'NONE', #48765, 1000.000000000000000 ) ;
#69477 = AXIS2_PLACEMENT_3D ( 'NONE', #86590, #38150, #95778 ) ;
#69478 = LINE ( 'NONE', #98951, #62677 ) ;
#69479 = VERTEX_POINT ( 'NONE', #124062 ) ;
#69480 = AXIS2_PLACEMENT_3D ( 'NONE', #64770, #5838, #7782 ) ;
#69481 = CIRCLE ( 'NONE', #2565, 0.06509327318403745899 ) ;
#69482 = VERTEX_POINT ( 'NONE', #84126 ) ;
#69483 = CARTESIAN_POINT ( 'NONE',  ( 8.949999999999919353, 2.500000000000000000, -6.048780366869526581 ) ) ;
#69484 = VECTOR ( 'NONE', #60075, 1000.000000000000000 ) ;
#69485 = ORIENTED_EDGE ( 'NONE', *, *, #103913, .T. ) ;
#69486 = DIRECTION ( 'NONE',  ( 0.000000000000000000, 0.000000000000000000, 1.000000000000000000 ) ) ;
#69487 = CARTESIAN_POINT ( 'NONE',  ( -0.4000000000000392131, 2.500000000000000000, -4.922947341949753586 ) ) ;
#69488 = VECTOR ( 'NONE', #52987, 1000.000000000000000 ) ;
#69489 = VERTEX_POINT ( 'NONE', #25869 ) ;
#69490 = DIRECTION ( 'NONE',  ( -0.000000000000000000, 1.000000000000000000, -0.000000000000000000 ) ) ;
#69491 = CARTESIAN_POINT ( 'NONE',  ( -8.350000000000012079, 12.50000000000000000, -2.922977105672691422 ) ) ;
#69492 = DIRECTION ( 'NONE',  ( 0.000000000000000000, 0.000000000000000000, 1.000000000000000000 ) ) ;
#69493 = DIRECTION ( 'NONE',  ( -0.000000000000000000, -1.000000000000000000, -0.000000000000000000 ) ) ;
#69494 = EDGE_CURVE ( 'NONE', #49326, #114386, #33751, .T. ) ;
#69495 = CYLINDRICAL_SURFACE ( 'NONE', #47773, 7.700000000000000178 ) ;
#69496 = ORIENTED_EDGE ( 'NONE', *, *, #98325, .T. ) ;
#69497 = EDGE_CURVE ( 'NONE', #97694, #126487, #73662, .T. ) ;
#69498 = FACE_OUTER_BOUND ( 'NONE', #104288, .T. ) ;
#69499 = CARTESIAN_POINT ( 'NONE',  ( 6.249999999999968914, 2.500000000000000000, -6.495190528383302464 ) ) ;
#69500 = EDGE_CURVE ( 'NONE', #43682, #58857, #97722, .T. ) ;
#69501 = DIRECTION ( 'NONE',  ( -0.000000000000000000, -1.000000000000000000, -0.000000000000000000 ) ) ;
#69502 = ORIENTED_EDGE ( 'NONE', *, *, #60903, .T. ) ;
#69503 = DIRECTION ( 'NONE',  ( 0.000000000000000000, 0.000000000000000000, 1.000000000000000000 ) ) ;
#69504 = VECTOR ( 'NONE', #86100, 1000.000000000000000 ) ;
#69505 = AXIS2_PLACEMENT_3D ( 'NONE', #42562, #62200, #32742 ) ;
#69506 = EDGE_CURVE ( 'NONE', #67824, #83209, #14087, .T. ) ;
#69507 = CIRCLE ( 'NONE', #54839, 0.1000000000000000472 ) ;
#69508 = ADVANCED_FACE ( 'NONE', ( #35695 ), #115510, .T. ) ;
#69509 = VERTEX_POINT ( 'NONE', #55334 ) ;
#69510 = CARTESIAN_POINT ( 'NONE',  ( 1.249999999999953815, 12.50000000000000000, 1.537336459617582918 ) ) ;
#69511 = PLANE ( 'NONE',  #40421 ) ;
#69512 = ADVANCED_FACE ( 'NONE', ( #35061 ), #114446, .T. ) ;
#69513 = DIRECTION ( 'NONE',  ( 0.000000000000000000, 0.000000000000000000, 1.000000000000000000 ) ) ;
#69514 = VERTEX_POINT ( 'NONE', #33127 ) ;
#69516 = CARTESIAN_POINT ( 'NONE',  ( 10.39999999999991509, 12.50000000000000000, -0.7579135962115917113 ) ) ;
#69515 = CIRCLE ( 'NONE', #117715, 0.1000000000000002554 ) ;
#69517 = AXIS2_PLACEMENT_3D ( 'NONE', #18284, #20231, #108604 ) ;
#69518 = CIRCLE ( 'NONE', #54948, 0.1000000000000002554 ) ;
#69519 = EDGE_CURVE ( 'NONE', #37534, #54491, #28786, .T. ) ;
#69520 = DIRECTION ( 'NONE',  ( -0.000000000000000000, 1.000000000000000000, -0.000000000000000000 ) ) ;
#69521 = CIRCLE ( 'NONE', #115481, 0.06509327318403745899 ) ;
#69522 = ORIENTED_EDGE ( 'NONE', *, *, #51079, .T. ) ;
#69523 = CONICAL_SURFACE ( 'NONE', #123802, 0.1000000000000000472, 0.003490658503988666988 ) ;
#69524 = DIRECTION ( 'NONE',  ( 0.000000000000000000, 1.000000000000000000, 0.000000000000000000 ) ) ;
#69525 = EDGE_LOOP ( 'NONE', ( #13915, #46869 ) ) ;
#69526 = ADVANCED_FACE ( 'NONE', ( #113602 ), #4917, .T. ) ;
#69527 = AXIS2_PLACEMENT_3D ( 'NONE', #18757, #49528, #89439 ) ;
#69528 = DIRECTION ( 'NONE',  ( 0.000000000000000000, 0.000000000000000000, 1.000000000000000000 ) ) ;
#69529 = EDGE_LOOP ( 'NONE', ( #96300, #7007 ) ) ;
#69530 = DIRECTION ( 'NONE',  ( 0.000000000000000000, 0.000000000000000000, -1.000000000000000000 ) ) ;
#69531 = CARTESIAN_POINT ( 'NONE',  ( 8.328334240990686865, 2.499999999999999556, -8.539519492767928099 ) ) ;
#69532 = VERTEX_POINT ( 'NONE', #3645 ) ;
#69533 = EDGE_LOOP ( 'NONE', ( #91825, #57368 ) ) ;
#69534 = CARTESIAN_POINT ( 'NONE',  ( -7.700000000000014388, 2.500000000000000000, -4.776537180435977525 ) ) ;
#69535 = PLANE ( 'NONE',  #115343 ) ;
#69536 = EDGE_LOOP ( 'NONE', ( #80707, #47775, #77006, #11327 ) ) ;
#69537 = AXIS2_PLACEMENT_3D ( 'NONE', #116830, #66447, #106375 ) ;
#69538 = LINE ( 'NONE', #48624, #119891 ) ;
#69539 = CARTESIAN_POINT ( 'NONE',  ( 4.199999999999939782, 12.50000000000000000, -2.276824562219559311E-15 ) ) ;
#69540 = DIRECTION ( 'NONE',  ( -0.000000000000000000, -1.000000000000000000, -0.000000000000000000 ) ) ;
#69541 = CARTESIAN_POINT ( 'NONE',  ( -3.350000000000028511, 2.500000000000000000, 2.857883832488649301 ) ) ;
#69542 = CARTESIAN_POINT ( 'NONE',  ( 7.499999999999925393, 12.50000000000000000, -0.6928203230275541413 ) ) ;
#69543 = LINE ( 'NONE', #68255, #95341 ) ;
#69544 = DIRECTION ( 'NONE',  ( 0.000000000000000000, 0.000000000000000000, -1.000000000000000000 ) ) ;
#69545 = VECTOR ( 'NONE', #72886, 1000.000000000000000 ) ;
#69546 = CIRCLE ( 'NONE', #102999, 1.000000000000000888 ) ;
#69547 = AXIS2_PLACEMENT_3D ( 'NONE', #111398, #123179, #93081 ) ;
#69548 = EDGE_LOOP ( 'NONE', ( #43523, #55662, #37837, #50803 ) ) ;
#69549 = ORIENTED_EDGE ( 'NONE', *, *, #58462, .F. ) ;
#69550 = ORIENTED_EDGE ( 'NONE', *, *, #1504, .F. ) ;
#69551 = ORIENTED_EDGE ( 'NONE', *, *, #52778, .T. ) ;
#69552 = CARTESIAN_POINT ( 'NONE',  ( 4.999999999999969802, 12.50000000000000000, 4.330127018922196314 ) ) ;
#69553 = DIRECTION ( 'NONE',  ( 0.000000000000000000, 0.000000000000000000, 1.000000000000000000 ) ) ;
#69554 = DIRECTION ( 'NONE',  ( 0.000000000000000000, 1.000000000000000000, 0.000000000000000000 ) ) ;
#69555 = ORIENTED_EDGE ( 'NONE', *, *, #43572, .F. ) ;
#69556 = FACE_BOUND ( 'NONE', #50432, .T. ) ;
#69557 = VERTEX_POINT ( 'NONE', #24575 ) ;
#69558 = CONICAL_SURFACE ( 'NONE', #90479, 0.1000000000000002554, 0.003490658503988666988 ) ;
#69559 = CARTESIAN_POINT ( 'NONE',  ( -10.80000000000000249, 2.500000000000000000, -4.430127018922197735 ) ) ;
#69560 = CARTESIAN_POINT ( 'NONE',  ( 5.649999999999936406, 2.500000000000000000, -6.248780366869526759 ) ) ;
#69561 = AXIS2_PLACEMENT_3D ( 'NONE', #8428, #128892, #99419 ) ;
#69563 = DIRECTION ( 'NONE',  ( 0.000000000000000000, 1.000000000000000000, 0.000000000000000000 ) ) ;
#69562 = VECTOR ( 'NONE', #116575, 1000.000000000000000 ) ;
#69564 = AXIS2_PLACEMENT_3D ( 'NONE', #57759, #85898, #17135 ) ;
#69565 = ADVANCED_FACE ( 'NONE', ( #83513 ), #43594, .T. ) ;
#69566 = DIRECTION ( 'NONE',  ( 0.000000000000000000, 0.000000000000000000, 1.000000000000000000 ) ) ;
#69567 = CARTESIAN_POINT ( 'NONE',  ( -11.84999999999999609, 2.500000000000000000, 1.918653347947321564 ) ) ;
#69568 = CARTESIAN_POINT ( 'NONE',  ( 2.899999999999943956, 12.50000000000000000, 4.265033745738159077 ) ) ;
#69569 = DIRECTION ( 'NONE',  ( 0.000000000000000000, 0.000000000000000000, 1.000000000000000000 ) ) ;
#69570 = DIRECTION ( 'NONE',  ( 0.000000000000000000, -0.000000000000000000, 1.000000000000000000 ) ) ;
#69571 = CARTESIAN_POINT ( 'NONE',  ( 2.099999999999949463, 12.50000000000000000, 0.6928203230275494784 ) ) ;
#69572 = DIRECTION ( 'NONE',  ( -0.000000000000000000, -1.000000000000000000, -0.000000000000000000 ) ) ;
#69573 = VECTOR ( 'NONE', #18349, 1000.000000000000000 ) ;
#69574 = EDGE_CURVE ( 'NONE', #24791, #77492, #54662, .T. ) ;
#69575 = ORIENTED_EDGE ( 'NONE', *, *, #30978, .T. ) ;
#69576 = ORIENTED_EDGE ( 'NONE', *, *, #101029, .T. ) ;
#69577 = EDGE_LOOP ( 'NONE', ( #3038, #106711, #116651, #127010 ) ) ;
#69579 = ORIENTED_EDGE ( 'NONE', *, *, #18224, .T. ) ;
#69578 = VECTOR ( 'NONE', #77806, 1000.000000000000000 ) ;
#69580 = AXIS2_PLACEMENT_3D ( 'NONE', #21994, #12135, #112294 ) ;
#69581 = VECTOR ( 'NONE', #83123, 1000.000000000000000 ) ;
#69582 = DIRECTION ( 'NONE',  ( 0.000000000000000000, 0.000000000000000000, 1.000000000000000000 ) ) ;
#69583 = DIRECTION ( 'NONE',  ( -0.000000000000000000, 1.000000000000000000, -0.000000000000000000 ) ) ;
#69585 = ORIENTED_EDGE ( 'NONE', *, *, #115753, .F. ) ;
#69584 = ORIENTED_EDGE ( 'NONE', *, *, #21943, .T. ) ;
#69586 = ORIENTED_EDGE ( 'NONE', *, *, #121799, .T. ) ;
#69587 = AXIS2_PLACEMENT_3D ( 'NONE', #3703, #113667, #63926 ) ;
#69588 = DIRECTION ( 'NONE',  ( 0.000000000000000000, 0.000000000000000000, 1.000000000000000000 ) ) ;
#69589 = DIRECTION ( 'NONE',  ( 0.000000000000000000, -0.9999939076577903929, 0.003490651415223739937 ) ) ;
#69590 = AXIS2_PLACEMENT_3D ( 'NONE', #38525, #47041, #67949 ) ;
#69591 = CARTESIAN_POINT ( 'NONE',  ( -2.100000000000033396, 12.50000000000000000, -5.022947341949754119 ) ) ;
#69592 = DIRECTION ( 'NONE',  ( 0.000000000000000000, 1.000000000000000000, 0.000000000000000000 ) ) ;
#69593 = CARTESIAN_POINT ( 'NONE',  ( 11.69999999999990514, 2.500000000000000000, -2.276824562219559311E-15 ) ) ;
#69594 = CARTESIAN_POINT ( 'NONE',  ( 142.3152275665817115, 0.5000000000000000000, 2.763522878056728693 ) ) ;
#69595 = DIRECTION ( 'NONE',  ( 0.000000000000000000, -0.9999939076577903929, 0.003490651415223739937 ) ) ;
#69596 = EDGE_LOOP ( 'NONE', ( #25793, #76914, #124848, #112823 ) ) ;
#69597 = DIRECTION ( 'NONE',  ( 0.000000000000000000, 1.000000000000000000, 0.000000000000000000 ) ) ;
#69598 = VERTEX_POINT ( 'NONE', #45521 ) ;
#69599 = EDGE_LOOP ( 'NONE', ( #75212, #84493 ) ) ;
#69600 = ORIENTED_EDGE ( 'NONE', *, *, #63324, .T. ) ;
#69601 = FACE_OUTER_BOUND ( 'NONE', #22079, .T. ) ;
#69602 = AXIS2_PLACEMENT_3D ( 'NONE', #94236, #54319, #123064 ) ;
#69603 = VECTOR ( 'NONE', #98779, 1000.000000000000000 ) ;
#69604 = EDGE_LOOP ( 'NONE', ( #88413, #73979, #86052, #26937 ) ) ;
#69605 = EDGE_LOOP ( 'NONE', ( #55149, #6581, #117511, #19834 ) ) ;
#69606 = DIRECTION ( 'NONE',  ( 0.000000000000000000, -0.9999939076577903929, 0.003490651415223739937 ) ) ;
#69607 = EDGE_CURVE ( 'NONE', #78336, #4391, #103784, .T. ) ;
#69609 = DIRECTION ( 'NONE',  ( 0.000000000000000000, 0.000000000000000000, 1.000000000000000000 ) ) ;
#69608 = VECTOR ( 'NONE', #33303, 1000.000000000000000 ) ;
#69610 = DIRECTION ( 'NONE',  ( 0.000000000000000000, 1.000000000000000000, 0.000000000000000000 ) ) ;
#69611 = DIRECTION ( 'NONE',  ( 0.000000000000000000, 0.000000000000000000, 1.000000000000000000 ) ) ;
#69612 = AXIS2_PLACEMENT_3D ( 'NONE', #33234, #73765, #71194 ) ;
#69613 = AXIS2_PLACEMENT_3D ( 'NONE', #5548, #86027, #26501 ) ;
#69614 = FACE_OUTER_BOUND ( 'NONE', #25043, .T. ) ;
#69615 = ORIENTED_EDGE ( 'NONE', *, *, #267, .T. ) ;
#69616 = DIRECTION ( 'NONE',  ( 0.000000000000000000, 0.000000000000000000, 1.000000000000000000 ) ) ;
#69617 = ADVANCED_FACE ( 'NONE', ( #14096 ), #103719, .T. ) ;
#69618 = AXIS2_PLACEMENT_3D ( 'NONE', #78691, #30239, #28289 ) ;
#69620 = ORIENTED_EDGE ( 'NONE', *, *, #70036, .F. ) ;
#69619 = CONICAL_SURFACE ( 'NONE', #119789, 0.1000000000000000472, 0.003490658503988666988 ) ;
#69621 = DIRECTION ( 'NONE',  ( 0.000000000000000000, -0.000000000000000000, 1.000000000000000000 ) ) ;
#69622 = AXIS2_PLACEMENT_3D ( 'NONE', #63052, #52582, #91225 ) ;
#69623 = VERTEX_POINT ( 'NONE', #8788 ) ;
#69624 = CARTESIAN_POINT ( 'NONE',  ( 113.0002503959617144, 8.700143905611811945, 0.1604050591010280913 ) ) ;
#69625 = DIRECTION ( 'NONE',  ( 0.000000000000000000, -0.000000000000000000, 1.000000000000000000 ) ) ;
#69626 = AXIS2_PLACEMENT_3D ( 'NONE', #31300, #83613, #71859 ) ;
#69627 = EDGE_LOOP ( 'NONE', ( #4028, #10843 ) ) ;
#69629 = ADVANCED_FACE ( 'NONE', ( #46803 ), #127300, .T. ) ;
#69628 = DIRECTION ( 'NONE',  ( 0.000000000000000000, 1.000000000000000000, 0.000000000000000000 ) ) ;
#69630 = CARTESIAN_POINT ( 'NONE',  ( -0.4500000000000397571, 12.50000000000000000, -6.495190528383302464 ) ) ;
#69631 = EDGE_CURVE ( 'NONE', #10759, #32556, #91465, .T. ) ;
#69632 = ORIENTED_EDGE ( 'NONE', *, *, #41781, .F. ) ;
#69633 = VECTOR ( 'NONE', #12486, 1000.000000000000000 ) ;
#69634 = EDGE_CURVE ( 'NONE', #15926, #44661, #108917, .T. ) ;
#69635 = LINE ( 'NONE', #12000, #744 ) ;
#69636 = EDGE_LOOP ( 'NONE', ( #121150, #45341 ) ) ;
#69637 = ORIENTED_EDGE ( 'NONE', *, *, #67725, .F. ) ;
#69638 = PLANE ( 'NONE',  #108286 ) ;
#69639 = LINE ( 'NONE', #91865, #53458 ) ;
#69640 = ADVANCED_FACE ( 'NONE', ( #97820 ), #12041, .T. ) ;
#69641 = FACE_OUTER_BOUND ( 'NONE', #108253, .T. ) ;
#69642 = DIRECTION ( 'NONE',  ( -0.000000000000000000, 1.000000000000000000, -0.000000000000000000 ) ) ;
#69643 = AXIS2_PLACEMENT_3D ( 'NONE', #107518, #36856, #7368 ) ;
#69644 = PLANE ( 'NONE',  #35388 ) ;
#69645 = ORIENTED_EDGE ( 'NONE', *, *, #50326, .F. ) ;
#69646 = FACE_OUTER_BOUND ( 'NONE', #88104, .T. ) ;
#69647 = AXIS2_PLACEMENT_3D ( 'NONE', #1883, #61478, #60819 ) ;
#69648 = VERTEX_POINT ( 'NONE', #58562 ) ;
#69649 = CONICAL_SURFACE ( 'NONE', #23677, 0.1000000000000000056, 0.003490658503988666988 ) ;
#69650 = CARTESIAN_POINT ( 'NONE',  ( 8.149999999999920419, 2.500000000000000000, -2.611473670974877592 ) ) ;
#69651 = FACE_OUTER_BOUND ( 'NONE', #1389, .T. ) ;
#69652 = CARTESIAN_POINT ( 'NONE',  ( 9.799999999999915445, 2.500000000000000000, -4.676537180435977881 ) ) ;
#69653 = FACE_OUTER_BOUND ( 'NONE', #50649, .T. ) ;
#69654 = CARTESIAN_POINT ( 'NONE',  ( -1.450000000000035483, 12.50000000000000000, 6.148780366869520897 ) ) ;
#69655 = CARTESIAN_POINT ( 'NONE',  ( -6.250000000000021316, 2.500000000000000000, -5.802370205355749988 ) ) ;
#69656 = AXIS2_PLACEMENT_3D ( 'NONE', #55541, #35263, #24788 ) ;
#69658 = CIRCLE ( 'NONE', #109370, 0.06509327318403745899 ) ;
#69657 = FACE_OUTER_BOUND ( 'NONE', #49476, .T. ) ;
#69659 = ORIENTED_EDGE ( 'NONE', *, *, #58729, .F. ) ;
#69660 = AXIS2_PLACEMENT_3D ( 'NONE', #68449, #16756, #56682 ) ;
#69661 = LINE ( 'NONE', #39595, #47996 ) ;
#69662 = DIRECTION ( 'NONE',  ( 0.000000000000000000, 0.000000000000000000, -1.000000000000000000 ) ) ;
#69663 = SURFACE_STYLE_USAGE ( .BOTH. , #78209 ) ;
#69664 = ORIENTED_EDGE ( 'NONE', *, *, #74794, .T. ) ;
#69665 = EDGE_CURVE ( 'NONE', #76961, #113506, #108179, .T. ) ;
#69666 = LINE ( 'NONE', #120706, #113772 ) ;
#69667 = EDGE_LOOP ( 'NONE', ( #65143, #42609, #64271, #47168 ) ) ;
#69668 = VECTOR ( 'NONE', #122015, 1000.000000000000000 ) ;
#69670 = ORIENTED_EDGE ( 'NONE', *, *, #73455, .F. ) ;
#69669 = AXIS2_PLACEMENT_3D ( 'NONE', #77513, #27762, #57891 ) ;
#69671 = CONICAL_SURFACE ( 'NONE', #40452, 0.1000000000000002554, 0.003490658503988666988 ) ;
#69672 = CARTESIAN_POINT ( 'NONE',  ( 6.049999999999934097, 2.500000000000000000, -6.148780366869526226 ) ) ;
#69673 = ADVANCED_FACE ( 'NONE', ( #28457 ), #57916, .T. ) ;
#69674 = ADVANCED_FACE ( 'NONE', ( #27786 ), #47284, .T. ) ;
#69676 = VERTEX_POINT ( 'NONE', #98453 ) ;
#69675 = CONICAL_SURFACE ( 'NONE', #65567, 0.09999999999999982514, 0.003490658503988666988 ) ;
#69677 = CARTESIAN_POINT ( 'NONE',  ( -0.6500000000000394351, 12.50000000000000000, 2.511473670974873507 ) ) ;
#69679 = ADVANCED_FACE ( 'NONE', ( #8146 ), #91187, .T. ) ;
#69678 = CARTESIAN_POINT ( 'NONE',  ( -7.100000000000018296, 12.50000000000000000, -4.330127018922201643 ) ) ;
#69680 = EDGE_CURVE ( 'NONE', #119313, #58497, #64278, .T. ) ;
#69681 = ORIENTED_EDGE ( 'NONE', *, *, #62514, .F. ) ;
#69682 = CARTESIAN_POINT ( 'NONE',  ( 4.599999999999936584, 2.500000000000000000, 3.537306695894645081 ) ) ;
#69683 = ADVANCED_FACE ( 'NONE', ( #29110 ), #124641, .T. ) ;
#69684 = DIRECTION ( 'NONE',  ( 0.000000000000000000, -0.9999939076577903929, 0.003490651415223739937 ) ) ;
#69685 = DIRECTION ( 'NONE',  ( 0.000000000000000000, -0.000000000000000000, 1.000000000000000000 ) ) ;
#69686 = ORIENTED_EDGE ( 'NONE', *, *, #122929, .F. ) ;
#69687 = EDGE_CURVE ( 'NONE', #97846, #22678, #68188, .T. ) ;
#69688 = EDGE_CURVE ( 'NONE', #87824, #91861, #57750, .T. ) ;
#69689 = EDGE_LOOP ( 'NONE', ( #34451, #43166 ) ) ;
#69690 = VERTEX_POINT ( 'NONE', #66427 ) ;
#69691 = DIRECTION ( 'NONE',  ( 0.000000000000000000, 1.000000000000000000, 0.000000000000000000 ) ) ;
#69692 = FACE_OUTER_BOUND ( 'NONE', #124653, .T. ) ;
#69694 = CARTESIAN_POINT ( 'NONE',  ( -13.94999999999998685, 2.500000000000000000, -2.511473670974875727 ) ) ;
#69693 = CIRCLE ( 'NONE', #67629, 0.06509327318403745899 ) ;
#69695 = AXIS2_PLACEMENT_3D ( 'NONE', #107740, #59309, #19344 ) ;
#69696 = FACE_BOUND ( 'NONE', #68333, .T. ) ;
#69697 = EDGE_LOOP ( 'NONE', ( #97885, #8128, #45587, #47673 ) ) ;
#69698 = DIRECTION ( 'NONE',  ( 0.000000000000000000, 1.000000000000000000, 0.000000000000000000 ) ) ;
#69699 = CARTESIAN_POINT ( 'NONE',  ( 1.449999999999949551, 2.500000000000000000, 6.841600689897072485 ) ) ;
#69700 = EDGE_LOOP ( 'NONE', ( #80654, #37373, #114111, #65154 ) ) ;
#69701 = FACE_OUTER_BOUND ( 'NONE', #74208, .T. ) ;
#69703 = CARTESIAN_POINT ( 'NONE',  ( -7.100000000000017408, 2.500000000000000000, -0.5928203230275542746 ) ) ;
#69702 = AXIS2_PLACEMENT_3D ( 'NONE', #44892, #25884, #14112 ) ;
#69704 = AXIS2_PLACEMENT_3D ( 'NONE', #3792, #95395, #124858 ) ;
#69705 = AXIS2_PLACEMENT_3D ( 'NONE', #86936, #8368, #48969 ) ;
#69706 = VECTOR ( 'NONE', #124821, 1000.000000000000000 ) ;
#69708 = CONICAL_SURFACE ( 'NONE', #44679, 0.1000000000000000472, 0.003490658503988666988 ) ;
#69707 = CARTESIAN_POINT ( 'NONE',  ( 87.50000000000002842, 4.028096841260344525E-16, 7.500000000000000888 ) ) ;
#69709 = FACE_OUTER_BOUND ( 'NONE', #49662, .T. ) ;
#69710 = CARTESIAN_POINT ( 'NONE',  ( -1.900000000000034106, 12.50000000000000000, -3.983716857408426293 ) ) ;
#69711 = DIRECTION ( 'NONE',  ( -4.274815082592931898E-19, -0.9999939076577903929, -0.003490651415223739937 ) ) ;
#69712 = LINE ( 'NONE', #120743, #123500 ) ;
#69713 = CONICAL_SURFACE ( 'NONE', #13264, 0.1000000000000002554, 0.003490658503988666988 ) ;
#69714 = VECTOR ( 'NONE', #118689, 1000.000000000000000 ) ;
#69715 = CIRCLE ( 'NONE', #115769, 0.06509327318403745899 ) ;
#69716 = ORIENTED_EDGE ( 'NONE', *, *, #58854, .T. ) ;
#69717 = ORIENTED_EDGE ( 'NONE', *, *, #61301, .T. ) ;
#69718 = EDGE_LOOP ( 'NONE', ( #37602, #13678, #89865, #71174 ) ) ;
#69719 = ORIENTED_EDGE ( 'NONE', *, *, #91416, .T. ) ;
#69721 = ORIENTED_EDGE ( 'NONE', *, *, #20665, .F. ) ;
#69720 = CIRCLE ( 'NONE', #52996, 0.09999999999999982514 ) ;
#69722 = CARTESIAN_POINT ( 'NONE',  ( -6.249999999999981348, 12.50000000000000000, 6.495190528383297135 ) ) ;
#69723 = AXIS2_PLACEMENT_3D ( 'NONE', #125167, #64305, #93139 ) ;
#69724 = CARTESIAN_POINT ( 'NONE',  ( 11.24999999999990941, 2.500000000000000000, 7.188010851410848723 ) ) ;
#69725 = ORIENTED_EDGE ( 'NONE', *, *, #28757, .T. ) ;
#69726 = FACE_BOUND ( 'NONE', #70924, .T. ) ;
#69727 = LINE ( 'NONE', #19319, #70857 ) ;
#69728 = DIRECTION ( 'NONE',  ( 0.000000000000000000, 0.000000000000000000, 1.000000000000000000 ) ) ;
#69729 = CARTESIAN_POINT ( 'NONE',  ( -0.6500000000000394351, 2.500000000000000000, 6.841600689897072485 ) ) ;
#69730 = PLANE ( 'NONE',  #30787 ) ;
#69731 = DIRECTION ( 'NONE',  ( 0.000000000000000000, -0.000000000000000000, 1.000000000000000000 ) ) ;
#69732 = CARTESIAN_POINT ( 'NONE',  ( 1.649999999999951505, 2.500000000000000000, 1.372243186433545370 ) ) ;
#69733 = VERTEX_POINT ( 'NONE', #19249 ) ;
#69734 = CIRCLE ( 'NONE', #86443, 0.09999999999999982514 ) ;
#69735 = VERTEX_POINT ( 'NONE', #59213 ) ;
#69736 = ADVANCED_FACE ( 'NONE', ( #108287 ), #93528, .T. ) ;
#69737 = ORIENTED_EDGE ( 'NONE', *, *, #66308, .T. ) ;
#69738 = ORIENTED_EDGE ( 'NONE', *, *, #73924, .F. ) ;
#69739 = ORIENTED_EDGE ( 'NONE', *, *, #7416, .T. ) ;
#69740 = DIRECTION ( 'NONE',  ( 0.000000000000000000, 0.000000000000000000, 1.000000000000000000 ) ) ;
#69741 = ORIENTED_EDGE ( 'NONE', *, *, #47334, .T. ) ;
#69742 = DIRECTION ( 'NONE',  ( 0.000000000000000000, 0.000000000000000000, 1.000000000000000000 ) ) ;
#69743 = AXIS2_PLACEMENT_3D ( 'NONE', #14472, #75340, #34804 ) ;
#69745 = CARTESIAN_POINT ( 'NONE',  ( -8.750000000000010658, 2.500000000000000000, 2.757883832488649656 ) ) ;
#69744 = AXIS2_PLACEMENT_3D ( 'NONE', #71445, #9482, #7532 ) ;
#69746 = DIRECTION ( 'NONE',  ( 0.000000000000000000, 1.000000000000000000, 0.000000000000000000 ) ) ;
#69747 = CARTESIAN_POINT ( 'NONE',  ( 185.9427083336747160, -6.551208109652278289, 3.782341765624995134 ) ) ;
#69748 = DIRECTION ( 'NONE',  ( -0.000000000000000000, -1.000000000000000000, -0.000000000000000000 ) ) ;
#69749 = CARTESIAN_POINT ( 'NONE',  ( 8.099999999999923261, 2.500000000000000000, 4.576537180435972019 ) ) ;
#69750 = CARTESIAN_POINT ( 'NONE',  ( 2.499999999999948930, 2.500000000000000000, -5.022947341949754119 ) ) ;
#69751 = CONICAL_SURFACE ( 'NONE', #61454, 0.1000000000000000056, 0.003490658503988666988 ) ;
#69752 = VERTEX_POINT ( 'NONE', #116166 ) ;
#69753 = DIRECTION ( 'NONE',  ( 0.000000000000000000, 0.000000000000000000, 1.000000000000000000 ) ) ;
#69754 = CONICAL_SURFACE ( 'NONE', #59318, 0.09999999999999982514, 0.003490658503988666988 ) ;
#69755 = CONICAL_SURFACE ( 'NONE', #44729, 0.1000000000000002554, 0.003490658503988666988 ) ;
#69756 = EDGE_LOOP ( 'NONE', ( #73336, #39987, #13718, #94546 ) ) ;
#69757 = AXIS2_PLACEMENT_3D ( 'NONE', #64506, #4274, #15391 ) ;
#69758 = EDGE_LOOP ( 'NONE', ( #70383, #101224, #63589, #79096 ) ) ;
#69759 = DIRECTION ( 'NONE',  ( 0.000000000000000000, 0.000000000000000000, 1.000000000000000000 ) ) ;
#69760 = LINE ( 'NONE', #60607, #53141 ) ;
#69761 = LINE ( 'NONE', #19355, #6998 ) ;
#69762 = AXIS2_PLACEMENT_3D ( 'NONE', #29191, #58645, #69084 ) ;
#69763 = ORIENTED_EDGE ( 'NONE', *, *, #81448, .T. ) ;
#69764 = ORIENTED_EDGE ( 'NONE', *, *, #35785, .T. ) ;
#69765 = DIRECTION ( 'NONE',  ( 0.000000000000000000, -0.000000000000000000, 1.000000000000000000 ) ) ;
#69767 = AXIS2_PLACEMENT_3D ( 'NONE', #24453, #14606, #55210 ) ;
#69766 = CARTESIAN_POINT ( 'NONE',  ( 9.149999999999915090, 2.500000000000000000, -2.265063509461101798 ) ) ;
#69769 = AXIS2_PLACEMENT_3D ( 'NONE', #109322, #119787, #117833 ) ;
#69768 = CARTESIAN_POINT ( 'NONE',  ( 11.84999999999990727, 2.500000000000000000, -2.611473670974877592 ) ) ;
#69770 = CONICAL_SURFACE ( 'NONE', #53055, 0.09999999999999982514, 0.003490658503988666988 ) ;
#69771 = FACE_OUTER_BOUND ( 'NONE', #43558, .T. ) ;
#69772 = VERTEX_POINT ( 'NONE', #26515 ) ;
#69773 = PLANE ( 'NONE',  #98296 ) ;
#69774 = ORIENTED_EDGE ( 'NONE', *, *, #21140, .F. ) ;
#69775 = CARTESIAN_POINT ( 'NONE',  ( 1.699999999999951994, 12.50000000000000000, 0.06509327318403515528 ) ) ;
#69776 = ADVANCED_FACE ( 'NONE', ( #56593 ), #36979, .T. ) ;
#69777 = ORIENTED_EDGE ( 'NONE', *, *, #25110, .F. ) ;
#69778 = CARTESIAN_POINT ( 'NONE',  ( 186.4166666666666856, 6.668395609140176816, 3.850000000000000977 ) ) ;
#69779 = CARTESIAN_POINT ( 'NONE',  ( -5.450000000000019718, 12.50000000000000000, 6.495190528383297135 ) ) ;
#69780 = DIRECTION ( 'NONE',  ( 0.000000000000000000, 0.000000000000000000, -1.000000000000000000 ) ) ;
#69781 = ADVANCED_FACE ( 'NONE', ( #57264 ), #51489, .T. ) ;
#69782 = CARTESIAN_POINT ( 'NONE',  ( -2.100000000000033840, 12.50000000000000000, 3.637306695894644726 ) ) ;
#69783 = EDGE_CURVE ( 'NONE', #3939, #69598, #30851, .T. ) ;
#69784 = ORIENTED_EDGE ( 'NONE', *, *, #114864, .F. ) ;
#69785 = DIRECTION ( 'NONE',  ( -0.000000000000000000, 1.000000000000000000, -0.000000000000000000 ) ) ;
#69786 = EDGE_CURVE ( 'NONE', #32002, #63267, #11761, .T. ) ;
#69787 = ORIENTED_EDGE ( 'NONE', *, *, #34431, .T. ) ;
#69788 = EDGE_CURVE ( 'NONE', #45708, #11852, #53816, .T. ) ;
#69789 = ORIENTED_EDGE ( 'NONE', *, *, #5369, .T. ) ;
#69790 = CIRCLE ( 'NONE', #17540, 0.1000000000000002554 ) ;
#69791 = AXIS2_PLACEMENT_3D ( 'NONE', #6424, #5799, #56196 ) ;
#69792 = EDGE_CURVE ( 'NONE', #59157, #29817, #112165, .T. ) ;
#69793 = DIRECTION ( 'NONE',  ( -0.000000000000000000, 1.000000000000000000, -0.000000000000000000 ) ) ;
#69794 = LINE ( 'NONE', #79614, #92985 ) ;
#69795 = CARTESIAN_POINT ( 'NONE',  ( -8.150000000000009237, 2.500000000000000000, 6.941600689897073018 ) ) ;
#69796 = ADVANCED_FACE ( 'NONE', ( #119387 ), #81008, .T. ) ;
#69797 = CARTESIAN_POINT ( 'NONE',  ( 186.9843750003414300, -8.734944146203032389, -1.604583208406768146E-15 ) ) ;
#69798 = DIRECTION ( 'NONE',  ( 0.000000000000000000, 0.000000000000000000, 1.000000000000000000 ) ) ;
#69799 = CARTESIAN_POINT ( 'NONE',  ( 4.599999999999936584, 2.500000000000000000, 3.737306695894644371 ) ) ;
#69800 = AXIS2_PLACEMENT_3D ( 'NONE', #110874, #49411, #21211 ) ;
#69801 = AXIS2_PLACEMENT_3D ( 'NONE', #90730, #394, #121462 ) ;
#69802 = CARTESIAN_POINT ( 'NONE',  ( -3.950000000000024603, 2.500000000000000000, 1.718653347947321386 ) ) ;
#69803 = CONICAL_SURFACE ( 'NONE', #44768, 0.09999999999999982514, 0.003490658503988666988 ) ;
#69804 = DIRECTION ( 'NONE',  ( 0.000000000000000000, 0.000000000000000000, 1.000000000000000000 ) ) ;
#69806 = CIRCLE ( 'NONE', #28037, 0.1000000000000002554 ) ;
#69805 = FACE_OUTER_BOUND ( 'NONE', #117728, .T. ) ;
#69807 = VECTOR ( 'NONE', #17118, 1000.000000000000000 ) ;
#69808 = ADVANCED_FACE ( 'NONE', ( #2190 ), #70346, .T. ) ;
#69809 = CIRCLE ( 'NONE', #13358, 0.1000000000000002554 ) ;
#69810 = VECTOR ( 'NONE', #64783, 1000.000000000000000 ) ;
#69811 = VECTOR ( 'NONE', #70196, 1000.000000000000000 ) ;
#69812 = ORIENTED_EDGE ( 'NONE', *, *, #58127, .T. ) ;
#69813 = DIRECTION ( 'NONE',  ( 0.000000000000000000, 0.000000000000000000, 1.000000000000000000 ) ) ;
#69814 = AXIS2_PLACEMENT_3D ( 'NONE', #79926, #11824, #30206 ) ;
#69815 = CARTESIAN_POINT ( 'NONE',  ( 6.649999999999929301, 12.50000000000000000, 6.430097255199259010 ) ) ;
#69816 = DIRECTION ( 'NONE',  ( 0.000000000000000000, 0.000000000000000000, 1.000000000000000000 ) ) ;
#69817 = DIRECTION ( 'NONE',  ( 1.000000000000000000, 0.000000000000000000, -1.445602896647339656E-16 ) ) ;
#69818 = CARTESIAN_POINT ( 'NONE',  ( -9.200000000000006395, 2.500000000000000000, -2.385244779468109755E-15 ) ) ;
#69819 = EDGE_LOOP ( 'NONE', ( #49567, #36229 ) ) ;
#69820 = LINE ( 'NONE', #28614, #653 ) ;
#69821 = DIRECTION ( 'NONE',  ( 0.000000000000000000, 1.000000000000000000, 0.000000000000000000 ) ) ;
#69823 = EDGE_LOOP ( 'NONE', ( #33543, #79424 ) ) ;
#69822 = DIRECTION ( 'NONE',  ( -0.000000000000000000, 1.000000000000000000, -0.000000000000000000 ) ) ;
#69824 = ADVANCED_FACE ( 'NONE', ( #81423 ), #43180, .T. ) ;
#69825 = AXIS2_PLACEMENT_3D ( 'NONE', #87065, #85133, #125067 ) ;
#69826 = EDGE_LOOP ( 'NONE', ( #107730, #89909, #95654, #46052 ) ) ;
#69827 = CARTESIAN_POINT ( 'NONE',  ( 8.299999999999922551, 2.500000000000000000, 0.09999999999999761857 ) ) ;
#69828 = EDGE_LOOP ( 'NONE', ( #4699, #113957, #79270, #90265 ) ) ;
#69829 = EDGE_LOOP ( 'NONE', ( #18794, #33884 ) ) ;
#69830 = ORIENTED_EDGE ( 'NONE', *, *, #116951, .F. ) ;
#69831 = DIRECTION ( 'NONE',  ( -0.000000000000000000, 1.000000000000000000, -0.000000000000000000 ) ) ;
#69832 = ADVANCED_FACE ( 'NONE', ( #40872 ), #37586, .F. ) ;
#69833 = ADVANCED_FACE ( 'NONE', ( #1399 ), #49439, .T. ) ;
#69834 = CARTESIAN_POINT ( 'NONE',  ( -2.900000000000029221, 12.50000000000000000, -2.276824562219559311E-15 ) ) ;
#69836 = EDGE_CURVE ( 'NONE', #94563, #62072, #93334, .T. ) ;
#69835 = DIRECTION ( 'NONE',  ( 0.000000000000000000, -0.9999939076577903929, 0.003490651415223739937 ) ) ;
#69837 = AXIS2_PLACEMENT_3D ( 'NONE', #15106, #84526, #73408 ) ;
#69838 = CARTESIAN_POINT ( 'NONE',  ( -3.950000000000024603, 2.500000000000000000, 1.818653347947321475 ) ) ;
#69839 = CIRCLE ( 'NONE', #59399, 0.1000000000000000472 ) ;
#69840 = ORIENTED_EDGE ( 'NONE', *, *, #100547, .F. ) ;
#69841 = EDGE_CURVE ( 'NONE', #18837, #110767, #122587, .T. ) ;
#69842 = CARTESIAN_POINT ( 'NONE',  ( 184.6250000000000000, -8.891194145520236347, -1.633285867636356299E-15 ) ) ;
#69843 = ORIENTED_EDGE ( 'NONE', *, *, #118613, .T. ) ;
#69844 = DIRECTION ( 'NONE',  ( -0.000000000000000000, -1.000000000000000000, -0.000000000000000000 ) ) ;
#69845 = PLANE ( 'NONE',  #65252 ) ;
#69846 = EDGE_CURVE ( 'NONE', #108066, #126779, #80823, .T. ) ;
#69847 = FACE_OUTER_BOUND ( 'NONE', #76881, .T. ) ;
#69848 = AXIS2_PLACEMENT_3D ( 'NONE', #64546, #24633, #126037 ) ;
#69849 = ADVANCED_FACE ( 'NONE', ( #40713 ), #76610, .T. ) ;
#69850 = ORIENTED_EDGE ( 'NONE', *, *, #107198, .T. ) ;
#69851 = EDGE_CURVE ( 'NONE', #66462, #73593, #78686, .T. ) ;
#69852 = ADVANCED_FACE ( 'NONE', ( #61630 ), #112127, .T. ) ;
#69853 = EDGE_LOOP ( 'NONE', ( #47351, #32566 ) ) ;
#69854 = EDGE_LOOP ( 'NONE', ( #104495, #15765 ) ) ;
#69855 = ORIENTED_EDGE ( 'NONE', *, *, #69836, .F. ) ;
#69856 = VERTEX_POINT ( 'NONE', #121817 ) ;
#69857 = FACE_OUTER_BOUND ( 'NONE', #46782, .T. ) ;
#69858 = FACE_OUTER_BOUND ( 'NONE', #112045, .T. ) ;
#69859 = DIRECTION ( 'NONE',  ( -0.000000000000000000, -1.000000000000000000, -0.000000000000000000 ) ) ;
#69860 = FACE_BOUND ( 'NONE', #80396, .T. ) ;
#69861 = CARTESIAN_POINT ( 'NONE',  ( -5.850000000000021849, 2.500000000000000000, -1.472243186433550122 ) ) ;
#69862 = CARTESIAN_POINT ( 'NONE',  ( 187.1979166673494603, 6.668395609140176816, 3.850000000000000977 ) ) ;
#69863 = EDGE_CURVE ( 'NONE', #47998, #91773, #13901, .T. ) ;
#69864 = CARTESIAN_POINT ( 'NONE',  ( -8.950000000000008171, 12.50000000000000000, -2.511473670974877948 ) ) ;
#69865 = DIRECTION ( 'NONE',  ( 0.000000000000000000, 0.000000000000000000, 1.000000000000000000 ) ) ;
#69866 = AXIS2_PLACEMENT_3D ( 'NONE', #52336, #81782, #60868 ) ;
#69867 = VECTOR ( 'NONE', #40316, 1000.000000000000000 ) ;
#69868 = DIRECTION ( 'NONE',  ( 0.000000000000000000, 1.000000000000000000, 0.000000000000000000 ) ) ;
#69869 = DIRECTION ( 'NONE',  ( 0.000000000000000000, -0.000000000000000000, 1.000000000000000000 ) ) ;
#69870 = CIRCLE ( 'NONE', #15471, 0.1000000000000002554 ) ;
#69871 = DIRECTION ( 'NONE',  ( 0.000000000000000000, -0.9999939076577903929, 0.003490651415223739937 ) ) ;
#69872 = AXIS2_PLACEMENT_3D ( 'NONE', #67239, #129456, #119589 ) ;
#69873 = DIRECTION ( 'NONE',  ( 0.000000000000000000, 0.000000000000000000, -1.000000000000000000 ) ) ;
#69874 = EDGE_LOOP ( 'NONE', ( #96932, #50562 ) ) ;
#69875 = ORIENTED_EDGE ( 'NONE', *, *, #128329, .T. ) ;
#69876 = EDGE_LOOP ( 'NONE', ( #43151, #62592 ) ) ;
#69877 = VERTEX_POINT ( 'NONE', #120540 ) ;
#69878 = CARTESIAN_POINT ( 'NONE',  ( -11.64999999999999858, 2.500000000000000000, -5.702370205355745902 ) ) ;
#69879 = DIRECTION ( 'NONE',  ( 0.000000000000000000, 0.000000000000000000, -1.000000000000000000 ) ) ;
#69880 = FACE_BOUND ( 'NONE', #33267, .T. ) ;
#69881 = DIRECTION ( 'NONE',  ( -0.000000000000000000, -1.000000000000000000, -0.000000000000000000 ) ) ;
#69882 = CONICAL_SURFACE ( 'NONE', #80355, 0.1000000000000002554, 0.003490658503988666988 ) ;
#69883 = AXIS2_PLACEMENT_3D ( 'NONE', #112467, #34562, #24078 ) ;
#69885 = EDGE_LOOP ( 'NONE', ( #972, #9870, #111198, #38559 ) ) ;
#69884 = CIRCLE ( 'NONE', #84554, 0.09999999999999982514 ) ;
#69887 = CIRCLE ( 'NONE', #67821, 0.06509327318403745899 ) ;
#69886 = CARTESIAN_POINT ( 'NONE',  ( -4.999999999999986677, 2.500000000000000000, 4.230127018922196669 ) ) ;
#69888 = DIRECTION ( 'NONE',  ( 0.000000000000000000, 0.000000000000000000, 1.000000000000000000 ) ) ;
#69889 = DIRECTION ( 'NONE',  ( -0.000000000000000000, 1.000000000000000000, -0.000000000000000000 ) ) ;
#69890 = DIRECTION ( 'NONE',  ( 0.000000000000000000, 1.000000000000000000, 0.000000000000000000 ) ) ;
#69891 = ORIENTED_EDGE ( 'NONE', *, *, #24558, .F. ) ;
#69892 = DIRECTION ( 'NONE',  ( 0.000000000000000000, 0.000000000000000000, 1.000000000000000000 ) ) ;
#69893 = AXIS2_PLACEMENT_3D ( 'NONE', #98319, #116680, #17157 ) ;
#69894 = AXIS2_PLACEMENT_3D ( 'NONE', #113734, #81681, #62062 ) ;
#69895 = EDGE_CURVE ( 'NONE', #91108, #19600, #20173, .T. ) ;
#69896 = VECTOR ( 'NONE', #70309, 1000.000000000000000 ) ;
#69897 = ORIENTED_EDGE ( 'NONE', *, *, #19974, .F. ) ;
#69898 = ORIENTED_EDGE ( 'NONE', *, *, #51171, .T. ) ;
#69899 = DIRECTION ( 'NONE',  ( -0.000000000000000000, -1.000000000000000000, -0.000000000000000000 ) ) ;
#69900 = CARTESIAN_POINT ( 'NONE',  ( -6.650000000000014566, 2.500000000000000000, 6.495190528383297135 ) ) ;
#69901 = ORIENTED_EDGE ( 'NONE', *, *, #30221, .F. ) ;
#69902 = VECTOR ( 'NONE', #101994, 1000.000000000000000 ) ;
#69903 = DIRECTION ( 'NONE',  ( -0.000000000000000000, -1.000000000000000000, -0.000000000000000000 ) ) ;
#69904 = DIRECTION ( 'NONE',  ( -0.000000000000000000, -1.000000000000000000, -0.000000000000000000 ) ) ;
#69905 = ORIENTED_EDGE ( 'NONE', *, *, #54538, .F. ) ;
#69906 = CARTESIAN_POINT ( 'NONE',  ( 4.599999999999938360, 2.500000000000000000, 0.09999999999999772959 ) ) ;
#69908 = ORIENTED_EDGE ( 'NONE', *, *, #42967, .T. ) ;
#69907 = VECTOR ( 'NONE', #10387, 1000.000000000000000 ) ;
#69909 = EDGE_CURVE ( 'NONE', #23517, #42124, #31515, .T. ) ;
#69910 = PLANE ( 'NONE',  #103873 ) ;
#69911 = ORIENTED_EDGE ( 'NONE', *, *, #59367, .F. ) ;
#69912 = DIRECTION ( 'NONE',  ( 0.000000000000000000, 0.000000000000000000, 1.000000000000000000 ) ) ;
#69913 = ORIENTED_EDGE ( 'NONE', *, *, #52007, .F. ) ;
#69914 = CARTESIAN_POINT ( 'NONE',  ( 111.9564666233451504, 7.065552756683692870, -3.073909748344711979 ) ) ;
#69915 = ORIENTED_EDGE ( 'NONE', *, *, #95772, .F. ) ;
#69916 = DIRECTION ( 'NONE',  ( 0.000000000000000000, 0.000000000000000000, 1.000000000000000000 ) ) ;
#69917 = DIRECTION ( 'NONE',  ( 0.000000000000000000, 0.000000000000000000, -1.000000000000000000 ) ) ;
#69918 = CARTESIAN_POINT ( 'NONE',  ( 10.19999999999991225, 12.50000000000000000, 3.983716857408420076 ) ) ;
#69919 = FACE_OUTER_BOUND ( 'NONE', #32238, .T. ) ;
#69920 = CARTESIAN_POINT ( 'NONE',  ( 16.55874544816229488, 0.4845305829427787869, -6.091953208798931207 ) ) ;
#69921 = AXIS2_PLACEMENT_3D ( 'NONE', #120192, #90724, #30540 ) ;
#69922 = ORIENTED_EDGE ( 'NONE', *, *, #23869, .F. ) ;
#69923 = EDGE_LOOP ( 'NONE', ( #52071, #1499, #61163, #82737 ) ) ;
#69924 = ORIENTED_EDGE ( 'NONE', *, *, #84207, .F. ) ;
#69925 = DIRECTION ( 'NONE',  ( 0.000000000000000000, -0.000000000000000000, 1.000000000000000000 ) ) ;
#69926 = DIRECTION ( 'NONE',  ( -4.274815082592931898E-19, -0.9999939076577903929, -0.003490651415223739937 ) ) ;
#69927 = CARTESIAN_POINT ( 'NONE',  ( -4.119968255444916849E-14, 12.50000000000000000, 3.637306695894644726 ) ) ;
#69929 = ORIENTED_EDGE ( 'NONE', *, *, #10791, .T. ) ;
#69928 = EDGE_LOOP ( 'NONE', ( #51277, #62857 ) ) ;
#69930 = ORIENTED_EDGE ( 'NONE', *, *, #41317, .T. ) ;
#69931 = DIRECTION ( 'NONE',  ( 0.000000000000000000, 0.000000000000000000, 1.000000000000000000 ) ) ;
#69932 = AXIS2_PLACEMENT_3D ( 'NONE', #108990, #59936, #321 ) ;
#69933 = ORIENTED_EDGE ( 'NONE', *, *, #121357, .T. ) ;
#69934 = FACE_OUTER_BOUND ( 'NONE', #99959, .T. ) ;
#69935 = AXIS2_PLACEMENT_3D ( 'NONE', #11739, #3851, #64065 ) ;
#69936 = EDGE_CURVE ( 'NONE', #49883, #58319, #71416, .T. ) ;
#69937 = ITEM_DEFINED_TRANSFORMATION ( 'NONE', 'NONE', #6569,  #108296 ) ;
#69938 = DIRECTION ( 'NONE',  ( 0.000000000000000000, 1.000000000000000000, 0.000000000000000000 ) ) ;
#69939 = CARTESIAN_POINT ( 'NONE',  ( -6.850000000000017408, 2.500000000000000000, -2.611473670974877592 ) ) ;
#69940 = CARTESIAN_POINT ( 'NONE',  ( 1.899999999999949507, 2.500000000000000000, 3.883716857408421319 ) ) ;
#69941 = DIRECTION ( 'NONE',  ( 0.000000000000000000, 0.000000000000000000, 1.000000000000000000 ) ) ;
#69942 = DIRECTION ( 'NONE',  ( 0.000000000000000000, 0.000000000000000000, -1.000000000000000000 ) ) ;
#69943 = FACE_OUTER_BOUND ( 'NONE', #60794, .T. ) ;
#69944 = EDGE_CURVE ( 'NONE', #78169, #63386, #29575, .T. ) ;
#69945 = EDGE_LOOP ( 'NONE', ( #8888, #73613, #41740, #35750 ) ) ;
#69946 = EDGE_LOOP ( 'NONE', ( #37615, #81650, #20315, #94322 ) ) ;
#69947 = AXIS2_PLACEMENT_3D ( 'NONE', #10111, #61143, #50059 ) ;
#69948 = DIRECTION ( 'NONE',  ( 0.000000000000000000, 0.000000000000000000, 1.000000000000000000 ) ) ;
#69949 = AXIS2_PLACEMENT_3D ( 'NONE', #25585, #66164, #46518 ) ;
#69950 = EDGE_CURVE ( 'NONE', #78151, #39661, #74550, .T. ) ;
#69951 = EDGE_LOOP ( 'NONE', ( #57238, #99765 ) ) ;
#69952 = EDGE_CURVE ( 'NONE', #59465, #28605, #124720, .T. ) ;
#69953 = ORIENTED_EDGE ( 'NONE', *, *, #117200, .T. ) ;
#69954 = EDGE_CURVE ( 'NONE', #13985, #76810, #34869, .T. ) ;
#69955 = CARTESIAN_POINT ( 'NONE',  ( 185.1927083336747160, 6.551208109652275624, -3.782341765624998686 ) ) ;
#69957 = EDGE_CURVE ( 'NONE', #87658, #39511, #98965, .T. ) ;
#69956 = DIRECTION ( 'NONE',  ( 0.000000000000000000, -0.9999939076577903929, 0.003490651415223739937 ) ) ;
#69958 = ADVANCED_FACE ( 'NONE', ( #19767 ), #99619, .T. ) ;
#69959 = DIRECTION ( 'NONE',  ( 0.000000000000000000, 1.000000000000000000, 0.000000000000000000 ) ) ;
#69960 = CARTESIAN_POINT ( 'NONE',  ( -0.8500000000000386136, 2.500000000000000000, 7.188010851410848723 ) ) ;
#69961 = AXIS2_PLACEMENT_3D ( 'NONE', #109956, #32052, #100133 ) ;
#69962 = CARTESIAN_POINT ( 'NONE',  ( -8.550000000000007816, 12.50000000000000000, 6.148780366869520009 ) ) ;
#69963 = CIRCLE ( 'NONE', #124244, 0.06509327318403745899 ) ;
#69964 = CARTESIAN_POINT ( 'NONE',  ( -13.94999999999998863, 2.500000000000000000, -1.718653347947323828 ) ) ;
#69965 = CARTESIAN_POINT ( 'NONE',  ( 3.749999999999938716, 12.50000000000000000, 7.253104124594885960 ) ) ;
#69966 = VECTOR ( 'NONE', #11923, 1000.000000000000000 ) ;
#69967 = EDGE_CURVE ( 'NONE', #55060, #80681, #110065, .T. ) ;
#69968 = CONICAL_SURFACE ( 'NONE', #61652, 0.09999999999999982514, 0.003490658503988666988 ) ;
#69970 = EDGE_CURVE ( 'NONE', #19230, #121105, #103476, .T. ) ;
#69969 = DIRECTION ( 'NONE',  ( 0.000000000000000000, -0.000000000000000000, 1.000000000000000000 ) ) ;
#69971 = ADVANCED_FACE ( 'NONE', ( #42649 ), #95393, .T. ) ;
#69972 = ORIENTED_EDGE ( 'NONE', *, *, #123415, .T. ) ;
#69973 = ORIENTED_EDGE ( 'NONE', *, *, #120546, .T. ) ;
#69974 = ORIENTED_EDGE ( 'NONE', *, *, #33029, .F. ) ;
#69975 = ORIENTED_EDGE ( 'NONE', *, *, #70950, .F. ) ;
#69976 = CARTESIAN_POINT ( 'NONE',  ( 14.14999999999989733, 2.500000000000000000, 2.957883832488649389 ) ) ;
#69977 = CARTESIAN_POINT ( 'NONE',  ( 10.84999999999990905, 12.50000000000000000, -7.188010851410854052 ) ) ;
#69978 = ORIENTED_EDGE ( 'NONE', *, *, #79473, .T. ) ;
#69979 = CARTESIAN_POINT ( 'NONE',  ( 9.149999999999916866, 2.500000000000000000, -2.857883832488653741 ) ) ;
#69980 = CARTESIAN_POINT ( 'NONE',  ( 4.799999999999934097, 12.50000000000000000, 4.741630453620009789 ) ) ;
#69981 = AXIS2_PLACEMENT_3D ( 'NONE', #103122, #110987, #93310 ) ;
#69982 = DIRECTION ( 'NONE',  ( 0.000000000000000000, -0.9999939076577903929, 0.003490651415223739937 ) ) ;
#69984 = VERTEX_POINT ( 'NONE', #62907 ) ;
#69983 = DIRECTION ( 'NONE',  ( 0.000000000000000000, 0.000000000000000000, 1.000000000000000000 ) ) ;
#69985 = AXIS2_PLACEMENT_3D ( 'NONE', #27130, #67026, #74301 ) ;
#69986 = CONICAL_SURFACE ( 'NONE', #124361, 0.09999999999999999167, 0.003490658503988666988 ) ;
#69987 = DIRECTION ( 'NONE',  ( 0.000000000000000000, 0.000000000000000000, -1.000000000000000000 ) ) ;
#69988 = DIRECTION ( 'NONE',  ( 0.000000000000000000, 0.000000000000000000, 1.000000000000000000 ) ) ;
#69989 = VERTEX_POINT ( 'NONE', #5257 ) ;
#69990 = CONICAL_SURFACE ( 'NONE', #93070, 0.09999999999999982514, 0.003490658503988666988 ) ;
#69991 = VECTOR ( 'NONE', #23910, 1000.000000000000000 ) ;
#69992 = ORIENTED_EDGE ( 'NONE', *, *, #57717, .F. ) ;
#69993 = ORIENTED_EDGE ( 'NONE', *, *, #39538, .T. ) ;
#69994 = EDGE_LOOP ( 'NONE', ( #68473, #61716 ) ) ;
#69995 = CARTESIAN_POINT ( 'NONE',  ( 9.799999999999918998, 2.500000000000000000, -0.3464101615137782364 ) ) ;
#69996 = CIRCLE ( 'NONE', #55413, 0.09999999999999982514 ) ;
#69997 = CARTESIAN_POINT ( 'NONE',  ( 0.3999999999999628852, 2.500000000000000000, -0.6928203230275520319 ) ) ;
#69998 = CARTESIAN_POINT ( 'NONE',  ( 3.299999999999944755, 12.50000000000000000, -4.265033745738164406 ) ) ;
#69999 = AXIS2_PLACEMENT_3D ( 'NONE', #11009, #90875, #1205 ) ;
#70000 = CIRCLE ( 'NONE', #65776, 0.06509327318403745899 ) ;
#70002 = VECTOR ( 'NONE', #87488, 1000.000000000000000 ) ;
#70001 = LINE ( 'NONE', #38121, #81542 ) ;
#70003 = VERTEX_POINT ( 'NONE', #83822 ) ;
#70004 = CARTESIAN_POINT ( 'NONE',  ( -1.050000000000037792, 12.50000000000000000, 1.753560074763284016 ) ) ;
#70005 = DIRECTION ( 'NONE',  ( -0.000000000000000000, -1.000000000000000000, -0.000000000000000000 ) ) ;
#70006 = CARTESIAN_POINT ( 'NONE',  ( -12.89999999999999147, 12.50000000000000000, 3.572213422710607489 ) ) ;
#70007 = CARTESIAN_POINT ( 'NONE',  ( 13.09999999999990195, 2.500000000000000000, 3.883716857408420431 ) ) ;
#70008 = EDGE_CURVE ( 'NONE', #2830, #41232, #13787, .T. ) ;
#70009 = EDGE_CURVE ( 'NONE', #91773, #47998, #30659, .T. ) ;
#70010 = VERTEX_POINT ( 'NONE', #64827 ) ;
#70011 = DIRECTION ( 'NONE',  ( 0.000000000000000000, -0.9999939076577903929, 0.003490651415223739937 ) ) ;
#70012 = ADVANCED_FACE ( 'NONE', ( #3974 ), #18109, .T. ) ;
#70013 = ORIENTED_EDGE ( 'NONE', *, *, #48720, .F. ) ;
#70014 = ORIENTED_EDGE ( 'NONE', *, *, #121115, .T. ) ;
#70015 = FACE_OUTER_BOUND ( 'NONE', #13511, .T. ) ;
#70016 = DIRECTION ( 'NONE',  ( 0.000000000000000000, 0.000000000000000000, 1.000000000000000000 ) ) ;
#70017 = FACE_BOUND ( 'NONE', #36226, .T. ) ;
#70018 = DIRECTION ( 'NONE',  ( 0.000000000000000000, 0.000000000000000000, 1.000000000000000000 ) ) ;
#70019 = AXIS2_PLACEMENT_3D ( 'NONE', #97729, #8055, #87257 ) ;
#70020 = DIRECTION ( 'NONE',  ( 0.000000000000000000, 0.000000000000000000, 1.000000000000000000 ) ) ;
#70021 = EDGE_CURVE ( 'NONE', #92462, #83779, #33462, .T. ) ;
#70022 = LINE ( 'NONE', #9803, #31165 ) ;
#70023 = DIRECTION ( 'NONE',  ( -4.274815082592931898E-19, -0.9999939076577903929, -0.003490651415223739937 ) ) ;
#70024 = CARTESIAN_POINT ( 'NONE',  ( 2.499999999999983569, 12.50000000000000000, -4.330127018922201643 ) ) ;
#70025 = DIRECTION ( 'NONE',  ( 0.000000000000000000, 0.000000000000000000, 1.000000000000000000 ) ) ;
#70026 = CARTESIAN_POINT ( 'NONE',  ( 6.899999999999928413, 12.50000000000000000, 4.611443907251934426 ) ) ;
#70027 = ORIENTED_EDGE ( 'NONE', *, *, #118917, .T. ) ;
#70028 = AXIS2_PLACEMENT_3D ( 'NONE', #46716, #56525, #85973 ) ;
#70029 = VECTOR ( 'NONE', #69871, 1000.000000000000000 ) ;
#70030 = DIRECTION ( 'NONE',  ( 0.000000000000000000, 0.000000000000000000, 1.000000000000000000 ) ) ;
#70031 = DIRECTION ( 'NONE',  ( 0.000000000000000000, 0.000000000000000000, -1.000000000000000000 ) ) ;
#70032 = EDGE_LOOP ( 'NONE', ( #24697, #34688, #127228, #20107 ) ) ;
#70033 = ORIENTED_EDGE ( 'NONE', *, *, #126524, .F. ) ;
#70034 = CARTESIAN_POINT ( 'NONE',  ( -4.800000000000028244, 2.500000000000000000, -4.083716857408426826 ) ) ;
#70035 = CARTESIAN_POINT ( 'NONE',  ( -0.6000000000000383915, 2.500000000000000000, -4.776537180435977525 ) ) ;
#70036 = EDGE_CURVE ( 'NONE', #115297, #95313, #89129, .T. ) ;
#70037 = FACE_BOUND ( 'NONE', #45141, .T. ) ;
#70038 = LINE ( 'NONE', #69374, #51448 ) ;
#70039 = AXIS2_PLACEMENT_3D ( 'NONE', #28308, #37497, #66293 ) ;
#70040 = CARTESIAN_POINT ( 'NONE',  ( -11.89999999999999503, 2.500000000000000000, 4.676537180435972552 ) ) ;
#70041 = AXIS2_PLACEMENT_3D ( 'NONE', #102083, #90972, #11760 ) ;
#70042 = VERTEX_POINT ( 'NONE', #92350 ) ;
#70043 = CARTESIAN_POINT ( 'NONE',  ( -10.40000000000000213, 2.500000000000000000, 0.09999999999999772959 ) ) ;
#70044 = FACE_OUTER_BOUND ( 'NONE', #52674, .T. ) ;
#70045 = ORIENTED_EDGE ( 'NONE', *, *, #10998, .F. ) ;
#70046 = DIRECTION ( 'NONE',  ( -0.000000000000000000, -1.000000000000000000, -0.000000000000000000 ) ) ;
#70047 = CARTESIAN_POINT ( 'NONE',  ( -9.550000000000006040, 12.50000000000000000, -2.099970236277064473 ) ) ;
#70048 = CIRCLE ( 'NONE', #7336, 0.1000000000000000472 ) ;
#70049 = ADVANCED_FACE ( 'NONE', ( #43925 ), #116302, .T. ) ;
#70050 = CARTESIAN_POINT ( 'NONE',  ( 8.549999999999922551, 2.500000000000000000, -6.248780366869526759 ) ) ;
#70051 = PLANE ( 'NONE',  #48857 ) ;
#70052 = ORIENTED_EDGE ( 'NONE', *, *, #67744, .T. ) ;
#70053 = CARTESIAN_POINT ( 'NONE',  ( 14.19999999999989626, 12.50000000000000000, -2.276824562219559311E-15 ) ) ;
#70054 = CARTESIAN_POINT ( 'NONE',  ( 4.599999999999939249, 12.50000000000000000, -3.637306695894650055 ) ) ;
#70055 = DIRECTION ( 'NONE',  ( -4.274815082592931898E-19, -0.9999939076577903929, -0.003490651415223739937 ) ) ;
#70056 = CARTESIAN_POINT ( 'NONE',  ( 21.24748443165276512, -0.7426079187842464790, -4.181982372968835904 ) ) ;
#70057 = VERTEX_POINT ( 'NONE', #112013 ) ;
#70058 = ORIENTED_EDGE ( 'NONE', *, *, #9276, .F. ) ;
#70059 = EDGE_CURVE ( 'NONE', #111925, #106111, #66134, .T. ) ;
#70060 = CARTESIAN_POINT ( 'NONE',  ( 1.649999999999948841, 2.500000000000000000, 6.495190528383297135 ) ) ;
#70061 = CIRCLE ( 'NONE', #93051, 0.06509327318403743123 ) ;
#70062 = ORIENTED_EDGE ( 'NONE', *, *, #117457, .F. ) ;
#70063 = DIRECTION ( 'NONE',  ( 0.000000000000000000, 0.000000000000000000, 1.000000000000000000 ) ) ;
#70064 = FACE_OUTER_BOUND ( 'NONE', #60871, .T. ) ;
#70066 = DIRECTION ( 'NONE',  ( 0.000000000000000000, 1.000000000000000000, 0.000000000000000000 ) ) ;
#70065 = AXIS2_PLACEMENT_3D ( 'NONE', #988, #70373, #119457 ) ;
#70067 = ORIENTED_EDGE ( 'NONE', *, *, #120671, .T. ) ;
#70068 = CONICAL_SURFACE ( 'NONE', #34582, 0.1000000000000000472, 0.003490658503988666988 ) ;
#70069 = CARTESIAN_POINT ( 'NONE',  ( -8.100000000000013856, 2.500000000000000000, -0.4464101615137782142 ) ) ;
#70070 = FACE_OUTER_BOUND ( 'NONE', #61286, .T. ) ;
#70071 = CARTESIAN_POINT ( 'NONE',  ( 87.50000000000001421, 3.974992050023850698, -6.359987280038159163 ) ) ;
#70072 = VECTOR ( 'NONE', #95034, 1000.000000000000000 ) ;
#70073 = DIRECTION ( 'NONE',  ( 0.000000000000000000, 0.000000000000000000, -1.000000000000000000 ) ) ;
#70074 = PLANE ( 'NONE',  #82104 ) ;
#70075 = DIRECTION ( 'NONE',  ( 0.000000000000000000, 1.000000000000000000, 0.000000000000000000 ) ) ;
#70076 = CIRCLE ( 'NONE', #38711, 0.06509327318403743123 ) ;
#70077 = EDGE_LOOP ( 'NONE', ( #108893, #96201, #124793, #111638 ) ) ;
#70079 = ORIENTED_EDGE ( 'NONE', *, *, #29320, .T. ) ;
#70078 = AXIS2_PLACEMENT_3D ( 'NONE', #22763, #71188, #72498 ) ;
#70081 = CARTESIAN_POINT ( 'NONE',  ( 4.599999999999935696, 12.50000000000000000, 5.022947341949748790 ) ) ;
#70080 = AXIS2_PLACEMENT_3D ( 'NONE', #98272, #47907, #126464 ) ;
#70082 = EDGE_LOOP ( 'NONE', ( #18040, #110042 ) ) ;
#70083 = CARTESIAN_POINT ( 'NONE',  ( -7.700000000000012612, 2.500000000000000000, 4.576537180435972019 ) ) ;
#70086 = ORIENTED_EDGE ( 'NONE', *, *, #24124, .T. ) ;
#70085 = ORIENTED_EDGE ( 'NONE', *, *, #16994, .F. ) ;
#70084 = CONICAL_SURFACE ( 'NONE', #118195, 0.09999999999999982514, 0.003490658503988666988 ) ;
#70087 = ORIENTED_EDGE ( 'NONE', *, *, #63918, .T. ) ;
#70088 = CARTESIAN_POINT ( 'NONE',  ( 87.50000000000000000, -0.7169905660282998028, -7.499999999999998224 ) ) ;
#70089 = AXIS2_PLACEMENT_3D ( 'NONE', #73018, #102477, #12786 ) ;
#70091 = AXIS2_PLACEMENT_3D ( 'NONE', #53323, #53956, #13376 ) ;
#70090 = DIRECTION ( 'NONE',  ( 0.000000000000000000, 0.000000000000000000, -1.000000000000000000 ) ) ;
#70092 = CARTESIAN_POINT ( 'NONE',  ( 11.64999999999990443, 2.500000000000000000, -7.188010851410854052 ) ) ;
#70093 = EDGE_CURVE ( 'NONE', #17252, #96946, #99605, .T. ) ;
#70094 = SURFACE_STYLE_FILL_AREA ( #32767 ) ;
#70095 = DIRECTION ( 'NONE',  ( 0.000000000000000000, 0.000000000000000000, -1.000000000000000000 ) ) ;
#70096 = LINE ( 'NONE', #51110, #121233 ) ;
#70097 = DIRECTION ( 'NONE',  ( 0.000000000000000000, 0.000000000000000000, 1.000000000000000000 ) ) ;
#70098 = CARTESIAN_POINT ( 'NONE',  ( -7.900000000000014566, 12.50000000000000000, 0.06509327318403515528 ) ) ;
#70099 = CARTESIAN_POINT ( 'NONE',  ( 0.8499999999999527933, 2.500000000000000000, 7.188010851410848723 ) ) ;
#70100 = LINE ( 'NONE', #79913, #35220 ) ;
#70101 = ORIENTED_EDGE ( 'NONE', *, *, #104618, .F. ) ;
#70102 = ADVANCED_FACE ( 'NONE', ( #85112 ), #9711, .T. ) ;
#70103 = EDGE_LOOP ( 'NONE', ( #48747, #62470 ) ) ;
#70104 = CARTESIAN_POINT ( 'NONE',  ( 10.64999999999991331, 2.500000000000000000, -1.818653347947325916 ) ) ;
#70105 = EDGE_CURVE ( 'NONE', #33814, #1760, #125039, .T. ) ;
#70106 = ORIENTED_EDGE ( 'NONE', *, *, #31896, .T. ) ;
#70107 = EDGE_CURVE ( 'NONE', #11509, #103770, #82973, .T. ) ;
#70108 = ORIENTED_EDGE ( 'NONE', *, *, #73831, .F. ) ;
#70109 = EDGE_CURVE ( 'NONE', #102432, #66032, #62274, .T. ) ;
#70110 = CARTESIAN_POINT ( 'NONE',  ( 0.6499999999999543920, 2.500000000000000000, 6.148780366869520897 ) ) ;
#70111 = EDGE_CURVE ( 'NONE', #83056, #17094, #24470, .T. ) ;
#70112 = CIRCLE ( 'NONE', #82733, 0.06509327318403745899 ) ;
#70113 = FACE_OUTER_BOUND ( 'NONE', #92076, .T. ) ;
#70114 = CARTESIAN_POINT ( 'NONE',  ( -4.350000000000023626, 2.500000000000000000, 6.048780366869521252 ) ) ;
#70115 = DIRECTION ( 'NONE',  ( -4.274815082592931898E-19, -0.9999939076577903929, -0.003490651415223739937 ) ) ;
#70116 = CARTESIAN_POINT ( 'NONE',  ( -1.700000000000034817, 12.50000000000000000, -4.265033745738164406 ) ) ;
#70117 = EDGE_CURVE ( 'NONE', #43052, #28988, #32821, .T. ) ;
#70118 = LINE ( 'NONE', #110041, #109532 ) ;
#70119 = ORIENTED_EDGE ( 'NONE', *, *, #22714, .F. ) ;
#70120 = EDGE_CURVE ( 'NONE', #63981, #31023, #114346, .T. ) ;
#70121 = CIRCLE ( 'NONE', #13658, 0.09999999999999999167 ) ;
#70122 = ADVANCED_FACE ( 'NONE', ( #127622 ), #60005, .T. ) ;
#70123 = AXIS2_PLACEMENT_3D ( 'NONE', #33802, #54091, #37035 ) ;
#70124 = EDGE_CURVE ( 'NONE', #37517, #31757, #47456, .T. ) ;
#70125 = VERTEX_POINT ( 'NONE', #115192 ) ;
#70126 = FACE_OUTER_BOUND ( 'NONE', #7133, .T. ) ;
#70127 = EDGE_CURVE ( 'NONE', #41488, #103678, #89222, .T. ) ;
#70128 = ORIENTED_EDGE ( 'NONE', *, *, #129559, .F. ) ;
#70129 = DIRECTION ( 'NONE',  ( 0.000000000000000000, 1.000000000000000000, 0.000000000000000000 ) ) ;
#70130 = EDGE_LOOP ( 'NONE', ( #20812, #44427, #26668, #61074 ) ) ;
#70131 = ORIENTED_EDGE ( 'NONE', *, *, #29806, .T. ) ;
#70132 = EDGE_CURVE ( 'NONE', #54614, #52844, #53710, .T. ) ;
#70133 = DIRECTION ( 'NONE',  ( 0.000000000000000000, 0.000000000000000000, -1.000000000000000000 ) ) ;
#70134 = CARTESIAN_POINT ( 'NONE',  ( 4.999999999999971578, 2.500000000000000000, 0.09999999999999772959 ) ) ;
#70135 = AXIS2_PLACEMENT_3D ( 'NONE', #68864, #79352, #108783 ) ;
#70136 = DIRECTION ( 'NONE',  ( 0.000000000000000000, 0.000000000000000000, -1.000000000000000000 ) ) ;
#70137 = DIRECTION ( 'NONE',  ( -4.274815082592931898E-19, -0.9999939076577903929, -0.003490651415223739937 ) ) ;
#70138 = CONICAL_SURFACE ( 'NONE', #86844, 0.1000000000000002554, 0.003490658503988666988 ) ;
#70139 = FACE_OUTER_BOUND ( 'NONE', #109739, .T. ) ;
#70140 = EDGE_LOOP ( 'NONE', ( #101041, #77012, #124739, #55821 ) ) ;
#70141 = LINE ( 'NONE', #20390, #37384 ) ;
#70142 = DIRECTION ( 'NONE',  ( 0.000000000000000000, 1.000000000000000000, 0.000000000000000000 ) ) ;
#70143 = DIRECTION ( 'NONE',  ( -0.000000000000000000, -1.000000000000000000, -0.000000000000000000 ) ) ;
#70144 = DIRECTION ( 'NONE',  ( 0.000000000000000000, 1.000000000000000000, 0.000000000000000000 ) ) ;
#70145 = DIRECTION ( 'NONE',  ( 0.000000000000000000, 0.000000000000000000, 1.000000000000000000 ) ) ;
#70146 = VERTEX_POINT ( 'NONE', #27467 ) ;
#70147 = VECTOR ( 'NONE', #87240, 1000.000000000000000 ) ;
#70148 = CIRCLE ( 'NONE', #63875, 0.09999999999999982514 ) ;
#70149 = VERTEX_POINT ( 'NONE', #86396 ) ;
#70150 = CARTESIAN_POINT ( 'NONE',  ( 3.149999999999946176, 12.50000000000000000, -6.148780366869526226 ) ) ;
#70151 = EDGE_CURVE ( 'NONE', #23957, #64139, #68053, .T. ) ;
#70152 = ORIENTED_EDGE ( 'NONE', *, *, #21341, .T. ) ;
#70153 = CARTESIAN_POINT ( 'NONE',  ( 17.50011966276722930, -2.224296756944748488, 4.070989939658955947 ) ) ;
#70154 = CARTESIAN_POINT ( 'NONE',  ( -11.64999999999999680, 2.500000000000000000, 7.288010851410849256 ) ) ;
#70155 = VECTOR ( 'NONE', #63310, 1000.000000000000000 ) ;
#70156 = ORIENTED_EDGE ( 'NONE', *, *, #59767, .T. ) ;
#70157 = DIRECTION ( 'NONE',  ( -0.000000000000000000, 1.000000000000000000, -0.000000000000000000 ) ) ;
#70158 = CARTESIAN_POINT ( 'NONE',  ( -2.100000000000034728, 2.500000000000000000, 4.230127018922196669 ) ) ;
#70159 = CARTESIAN_POINT ( 'NONE',  ( -3.749999999999994671, 2.500000000000000000, -6.595190528383302109 ) ) ;
#70160 = AXIS2_PLACEMENT_3D ( 'NONE', #127569, #6463, #46418 ) ;
#70161 = DIRECTION ( 'NONE',  ( 0.000000000000000000, -0.9999939076577903929, 0.003490651415223739937 ) ) ;
#70162 = EDGE_CURVE ( 'NONE', #73210, #109722, #16036, .T. ) ;
#70163 = AXIS2_PLACEMENT_3D ( 'NONE', #62507, #33050, #72321 ) ;
#70164 = DIRECTION ( 'NONE',  ( 0.000000000000000000, 1.000000000000000000, 0.000000000000000000 ) ) ;
#70165 = CIRCLE ( 'NONE', #103617, 0.06509327318403745899 ) ;
#70166 = ADVANCED_FACE ( 'NONE', ( #18305 ), #122666, .T. ) ;
#70167 = ORIENTED_EDGE ( 'NONE', *, *, #78989, .F. ) ;
#70168 = CARTESIAN_POINT ( 'NONE',  ( -4.350000000000023626, 12.50000000000000000, 2.511473670974873507 ) ) ;
#70169 = CARTESIAN_POINT ( 'NONE',  ( -8.550000000000014921, 2.500000000000000000, -6.048780366869521252 ) ) ;
#70170 = EDGE_CURVE ( 'NONE', #99317, #95559, #22339, .T. ) ;
#70171 = VERTEX_POINT ( 'NONE', #26845 ) ;
#70172 = CONICAL_SURFACE ( 'NONE', #34685, 0.1000000000000000472, 0.003490658503988666988 ) ;
#70173 = EDGE_LOOP ( 'NONE', ( #34865, #63035 ) ) ;
#70174 = CARTESIAN_POINT ( 'NONE',  ( 8.149999999999920419, 2.500000000000000000, 6.741600689897071952 ) ) ;
#70175 = DIRECTION ( 'NONE',  ( 0.000000000000000000, -0.9999939076577903929, 0.003490651415223739937 ) ) ;
#70176 = CARTESIAN_POINT ( 'NONE',  ( 0.3999999999999628852, 2.500000000000000000, 0.6928203230275518099 ) ) ;
#70177 = VERTEX_POINT ( 'NONE', #98152 ) ;
#70178 = AXIS2_PLACEMENT_3D ( 'NONE', #108274, #98438, #8763 ) ;
#70179 = VECTOR ( 'NONE', #8692, 1000.000000000000000 ) ;
#70180 = DIRECTION ( 'NONE',  ( 0.000000000000000000, 0.000000000000000000, 1.000000000000000000 ) ) ;
#70181 = AXIS2_PLACEMENT_3D ( 'NONE', #39525, #109530, #121277 ) ;
#70182 = CARTESIAN_POINT ( 'NONE',  ( 3.749999999999976907, 2.500000000000000000, 2.265063509461097357 ) ) ;
#70183 = VECTOR ( 'NONE', #68681, 1000.000000000000000 ) ;
#70184 = VERTEX_POINT ( 'NONE', #57605 ) ;
#70185 = DIRECTION ( 'NONE',  ( -0.000000000000000000, 1.000000000000000000, -0.000000000000000000 ) ) ;
#70186 = ORIENTED_EDGE ( 'NONE', *, *, #36990, .F. ) ;
#70187 = CARTESIAN_POINT ( 'NONE',  ( -3.350000000000031619, 2.500000000000000000, -5.702370205355749455 ) ) ;
#70188 = ORIENTED_EDGE ( 'NONE', *, *, #70132, .T. ) ;
#70189 = CARTESIAN_POINT ( 'NONE',  ( -11.84999999999999609, 2.500000000000000000, 2.511473670974873507 ) ) ;
#70190 = CARTESIAN_POINT ( 'NONE',  ( -4.600000000000028066, 12.50000000000000000, -4.957854068765716882 ) ) ;
#70191 = ORIENTED_EDGE ( 'NONE', *, *, #17034, .T. ) ;
#70192 = ORIENTED_EDGE ( 'NONE', *, *, #45844, .T. ) ;
#70193 = FACE_OUTER_BOUND ( 'NONE', #26054, .T. ) ;
#70194 = DIRECTION ( 'NONE',  ( 0.000000000000000000, 0.000000000000000000, 1.000000000000000000 ) ) ;
#70195 = ORIENTED_EDGE ( 'NONE', *, *, #63108, .F. ) ;
#70197 = EDGE_CURVE ( 'NONE', #7097, #5713, #97628, .T. ) ;
#70196 = DIRECTION ( 'NONE',  ( 0.000000000000000000, -0.9999939076577903929, 0.003490651415223739937 ) ) ;
#70198 = DIRECTION ( 'NONE',  ( 0.000000000000000000, 0.000000000000000000, 1.000000000000000000 ) ) ;
#70199 = CARTESIAN_POINT ( 'NONE',  ( -11.64999999999999680, 12.50000000000000000, 6.495190528383297135 ) ) ;
#70200 = DIRECTION ( 'NONE',  ( -0.000000000000000000, -1.000000000000000000, -0.000000000000000000 ) ) ;
#70201 = DIRECTION ( 'NONE',  ( 0.000000000000000000, 0.000000000000000000, 1.000000000000000000 ) ) ;
#70202 = FACE_OUTER_BOUND ( 'NONE', #45321, .T. ) ;
#70203 = CONICAL_SURFACE ( 'NONE', #122444, 0.1000000000000000472, 0.003490658503988666988 ) ;
#70204 = CARTESIAN_POINT ( 'NONE',  ( -12.89999999999999147, 2.500000000000000000, 1.843143693225357538E-15 ) ) ;
#70205 = CONICAL_SURFACE ( 'NONE', #99463, 0.1000000000000002554, 0.003490658503988666988 ) ;
#70206 = CIRCLE ( 'NONE', #128820, 0.06509327318403745899 ) ;
#70207 = ORIENTED_EDGE ( 'NONE', *, *, #24608, .F. ) ;
#70208 = CIRCLE ( 'NONE', #105807, 0.09999999999999999167 ) ;
#70209 = EDGE_LOOP ( 'NONE', ( #97291, #84577 ) ) ;
#70210 = VERTEX_POINT ( 'NONE', #88319 ) ;
#70211 = DIRECTION ( 'NONE',  ( -4.274815082592931898E-19, -0.9999939076577903929, -0.003490651415223739937 ) ) ;
#70212 = CARTESIAN_POINT ( 'NONE',  ( -7.500000000000001776, -1.500000000000000000, 1.734723475976807094E-15 ) ) ;
#70213 = ADVANCED_FACE ( 'NONE', ( #106049 ), #57927, .T. ) ;
#70214 = DIRECTION ( 'NONE',  ( 0.000000000000000000, 1.000000000000000000, 0.000000000000000000 ) ) ;
#70216 = ORIENTED_EDGE ( 'NONE', *, *, #20782, .T. ) ;
#70215 = ORIENTED_EDGE ( 'NONE', *, *, #127123, .F. ) ;
#70217 = FACE_BOUND ( 'NONE', #59806, .T. ) ;
#70218 = VERTEX_POINT ( 'NONE', #36683 ) ;
#70219 = ADVANCED_FACE ( 'NONE', ( #97512 ), #108082, .T. ) ;
#70220 = FACE_OUTER_BOUND ( 'NONE', #105438, .T. ) ;
#70221 = DIRECTION ( 'NONE',  ( 1.000000000000000000, -0.000000000000000000, -0.000000000000000000 ) ) ;
#70222 = CARTESIAN_POINT ( 'NONE',  ( 1.449999999999952660, 12.50000000000000000, -6.776507416713040577 ) ) ;
#70223 = CARTESIAN_POINT ( 'NONE',  ( 17.99892160975016253, -2.500000000000000000, 4.934975027008865034 ) ) ;
#70224 = PLANE ( 'NONE',  #59704 ) ;
#70226 = AXIS2_PLACEMENT_3D ( 'NONE', #92431, #2759, #101623 ) ;
#70225 = CIRCLE ( 'NONE', #15830, 0.06509327318403743123 ) ;
#70227 = DIRECTION ( 'NONE',  ( -0.000000000000000000, 1.000000000000000000, -0.000000000000000000 ) ) ;
#70228 = DIRECTION ( 'NONE',  ( 1.000000000000000000, -0.000000000000000000, -0.000000000000000000 ) ) ;
#70229 = DIRECTION ( 'NONE',  ( 0.000000000000000000, -0.000000000000000000, 1.000000000000000000 ) ) ;
#70230 = ADVANCED_FACE ( 'NONE', ( #7837 ), #74638, .T. ) ;
#70231 = CARTESIAN_POINT ( 'NONE',  ( 3.549999999999943867, 2.500000000000000000, -6.148780366869526226 ) ) ;
#70232 = DIRECTION ( 'NONE',  ( 0.000000000000000000, 0.000000000000000000, -1.000000000000000000 ) ) ;
#70233 = AXIS2_PLACEMENT_3D ( 'NONE', #123782, #115911, #56978 ) ;
#70234 = ORIENTED_EDGE ( 'NONE', *, *, #22088, .F. ) ;
#70235 = ORIENTED_EDGE ( 'NONE', *, *, #100968, .F. ) ;
#70236 = VECTOR ( 'NONE', #72165, 1000.000000000000000 ) ;
#70237 = ORIENTED_EDGE ( 'NONE', *, *, #101903, .T. ) ;
#70238 = ORIENTED_EDGE ( 'NONE', *, *, #59740, .T. ) ;
#70239 = CARTESIAN_POINT ( 'NONE',  ( 7.899999999999924860, 2.500000000000000000, 4.230127018922196669 ) ) ;
#70240 = CARTESIAN_POINT ( 'NONE',  ( -13.14999999999999147, 2.500000000000000000, 1.918653347947325338 ) ) ;
#70242 = ORIENTED_EDGE ( 'NONE', *, *, #42178, .F. ) ;
#70241 = ORIENTED_EDGE ( 'NONE', *, *, #30393, .F. ) ;
#70243 = ORIENTED_EDGE ( 'NONE', *, *, #75036, .F. ) ;
#70244 = LINE ( 'NONE', #59808, #75208 ) ;
#70245 = PLANE ( 'NONE',  #105217 ) ;
#70246 = FACE_OUTER_BOUND ( 'NONE', #81946, .T. ) ;
#70247 = DIRECTION ( 'NONE',  ( -0.000000000000000000, -1.000000000000000000, -0.000000000000000000 ) ) ;
#70248 = FACE_OUTER_BOUND ( 'NONE', #3710, .T. ) ;
#70249 = LINE ( 'NONE', #110177, #49743 ) ;
#70250 = FACE_OUTER_BOUND ( 'NONE', #94259, .T. ) ;
#70251 = ORIENTED_EDGE ( 'NONE', *, *, #110213, .T. ) ;
#70252 = FACE_OUTER_BOUND ( 'NONE', #118038, .T. ) ;
#70253 = VERTEX_POINT ( 'NONE', #56922 ) ;
#70254 = EDGE_CURVE ( 'NONE', #1609, #49878, #70446, .T. ) ;
#70256 = ORIENTED_EDGE ( 'NONE', *, *, #44210, .T. ) ;
#70255 = VECTOR ( 'NONE', #127070, 1000.000000000000000 ) ;
#70257 = EDGE_LOOP ( 'NONE', ( #20202, #24180, #127382, #124400 ) ) ;
#70258 = AXIS2_PLACEMENT_3D ( 'NONE', #71403, #70144, #2657 ) ;
#70259 = CARTESIAN_POINT ( 'NONE',  ( -1.900000000000035438, 2.500000000000000000, 4.083716857408420609 ) ) ;
#70260 = EDGE_LOOP ( 'NONE', ( #22600, #29492 ) ) ;
#70261 = ADVANCED_FACE ( 'NONE', ( #26204 ), #91369, .T. ) ;
#70262 = EDGE_LOOP ( 'NONE', ( #87747, #128106 ) ) ;
#70263 = ADVANCED_FACE ( 'NONE', ( #46472 ), #32807, .T. ) ;
#70264 = DIRECTION ( 'NONE',  ( -0.000000000000000000, 1.000000000000000000, -0.000000000000000000 ) ) ;
#70265 = VECTOR ( 'NONE', #60069, 1000.000000000000000 ) ;
#70266 =( NAMED_UNIT ( * ) PLANE_ANGLE_UNIT ( ) SI_UNIT ( $, .RADIAN. ) );
#70267 = DIRECTION ( 'NONE',  ( -0.000000000000000000, 1.000000000000000000, -0.000000000000000000 ) ) ;
#70268 = DIRECTION ( 'NONE',  ( -0.000000000000000000, -1.000000000000000000, -0.000000000000000000 ) ) ;
#70269 = CARTESIAN_POINT ( 'NONE',  ( 4.149999999999938183, 2.500000000000000000, 7.288010851410849256 ) ) ;
#70270 = ADVANCED_FACE ( 'NONE', ( #37327 ), #77233, .T. ) ;
#70271 = CARTESIAN_POINT ( 'NONE',  ( -2.900000000000030109, 2.500000000000000000, -3.637306695894650055 ) ) ;
#70272 = ADVANCED_FACE ( 'NONE', ( #90257 ), #105944, .T. ) ;
#70273 = EDGE_CURVE ( 'NONE', #3662, #48633, #85099, .T. ) ;
#70274 = ORIENTED_EDGE ( 'NONE', *, *, #23379, .T. ) ;
#70275 = DIRECTION ( 'NONE',  ( -0.000000000000000000, -1.000000000000000000, -0.000000000000000000 ) ) ;
#70276 = CIRCLE ( 'NONE', #80745, 0.06509327318403745899 ) ;
#70277 = VERTEX_POINT ( 'NONE', #19607 ) ;
#70278 = CARTESIAN_POINT ( 'NONE',  ( 4.599999999999935696, 12.50000000000000000, 5.088040615133786027 ) ) ;
#70279 = AXIS2_PLACEMENT_3D ( 'NONE', #106774, #36123, #105509 ) ;
#70280 = EDGE_CURVE ( 'NONE', #75731, #27272, #30756, .T. ) ;
#70281 = ORIENTED_EDGE ( 'NONE', *, *, #113997, .T. ) ;
#70282 = CARTESIAN_POINT ( 'NONE',  ( -13.09999999999999254, 2.500000000000000000, -0.3464101615137741286 ) ) ;
#70283 = DIRECTION ( 'NONE',  ( -0.000000000000000000, -1.000000000000000000, -0.000000000000000000 ) ) ;
#70284 = VERTEX_POINT ( 'NONE', #30093 ) ;
#70285 = CARTESIAN_POINT ( 'NONE',  ( -11.44999999999999751, 2.500000000000000000, -6.941600689897074794 ) ) ;
#70286 = CARTESIAN_POINT ( 'NONE',  ( -11.64999999999999680, 12.50000000000000000, 2.165063509461097713 ) ) ;
#70287 = ORIENTED_EDGE ( 'NONE', *, *, #85978, .F. ) ;
#70288 = EDGE_CURVE ( 'NONE', #97686, #127904, #59566, .T. ) ;
#70289 = FACE_OUTER_BOUND ( 'NONE', #112009, .T. ) ;
#70290 = VERTEX_POINT ( 'NONE', #70004 ) ;
#70291 = EDGE_LOOP ( 'NONE', ( #2496, #68151, #51413, #87888 ) ) ;
#70292 = DIRECTION ( 'NONE',  ( 0.000000000000000000, -0.000000000000000000, 1.000000000000000000 ) ) ;
#70293 = DIRECTION ( 'NONE',  ( 0.000000000000000000, 0.000000000000000000, 1.000000000000000000 ) ) ;
#70294 = CARTESIAN_POINT ( 'NONE',  ( 184.0468750003414300, -8.734944146203032389, -1.604583208406768146E-15 ) ) ;
#70295 = AXIS2_PLACEMENT_3D ( 'NONE', #127534, #37855, #19504 ) ;
#70296 = DIRECTION ( 'NONE',  ( 0.000000000000000000, 0.000000000000000000, 1.000000000000000000 ) ) ;
#70297 = CARTESIAN_POINT ( 'NONE',  ( -3.749999999999991562, 12.50000000000000000, 6.495190528383297135 ) ) ;
#70298 = VERTEX_POINT ( 'NONE', #38625 ) ;
#70299 = CONICAL_SURFACE ( 'NONE', #124678, 0.1000000000000000472, 0.003490658503988666988 ) ;
#70300 = DIRECTION ( 'NONE',  ( -4.274815082592931898E-19, -0.9999939076577903929, -0.003490651415223739937 ) ) ;
#70301 = AXIS2_PLACEMENT_3D ( 'NONE', #85671, #124314, #5167 ) ;
#70302 = CIRCLE ( 'NONE', #87015, 0.09999999999999982514 ) ;
#70303 = VERTEX_POINT ( 'NONE', #595 ) ;
#70304 = CIRCLE ( 'NONE', #114216, 0.1000000000000000056 ) ;
#70305 = CARTESIAN_POINT ( 'NONE',  ( 3.549999999999944755, 2.500000000000000000, -6.741600689897077281 ) ) ;
#70306 = DIRECTION ( 'NONE',  ( -0.000000000000000000, -1.000000000000000000, -0.000000000000000000 ) ) ;
#70307 = AXIS2_PLACEMENT_3D ( 'NONE', #75817, #95470, #17537 ) ;
#70308 = DIRECTION ( 'NONE',  ( 0.000000000000000000, 0.000000000000000000, 1.000000000000000000 ) ) ;
#70309 = DIRECTION ( 'NONE',  ( -4.274815082592931898E-19, -0.9999939076577903929, -0.003490651415223739937 ) ) ;
#70310 = CARTESIAN_POINT ( 'NONE',  ( 12.09999999999990550, 12.50000000000000000, -4.265033745738164406 ) ) ;
#70311 = CARTESIAN_POINT ( 'NONE',  ( 0.000000000000000000, 8.500000000000000000, 0.000000000000000000 ) ) ;
#70312 = DIRECTION ( 'NONE',  ( 0.000000000000000000, 1.000000000000000000, 0.000000000000000000 ) ) ;
#70313 = ORIENTED_EDGE ( 'NONE', *, *, #106421, .F. ) ;
#70314 = CIRCLE ( 'NONE', #24247, 0.06509327318403745899 ) ;
#70316 = EDGE_CURVE ( 'NONE', #71034, #95476, #31373, .T. ) ;
#70315 = CARTESIAN_POINT ( 'NONE',  ( -8.350000000000012079, 2.500000000000000000, -2.757883832488654097 ) ) ;
#70318 = AXIS2_PLACEMENT_3D ( 'NONE', #83748, #111246, #34007 ) ;
#70317 = VECTOR ( 'NONE', #42406, 1000.000000000000000 ) ;
#70319 = DIRECTION ( 'NONE',  ( -0.000000000000000000, -1.000000000000000000, -0.000000000000000000 ) ) ;
#70320 = CARTESIAN_POINT ( 'NONE',  ( 9.349999999999919709, 2.500000000000000000, -6.148780366869526226 ) ) ;
#70321 = ORIENTED_EDGE ( 'NONE', *, *, #22262, .T. ) ;
#70322 = CARTESIAN_POINT ( 'NONE',  ( -6.050000000000017586, 12.50000000000000000, 1.818653347947321475 ) ) ;
#70323 = EDGE_CURVE ( 'NONE', #80502, #7747, #112210, .T. ) ;
#70324 = VERTEX_POINT ( 'NONE', #11054 ) ;
#70325 = ORIENTED_EDGE ( 'NONE', *, *, #47899, .F. ) ;
#70326 = CARTESIAN_POINT ( 'NONE',  ( -8.750000000000012434, 2.500000000000000000, -5.902370205355745192 ) ) ;
#70327 = ORIENTED_EDGE ( 'NONE', *, *, #49921, .T. ) ;
#70328 = DIRECTION ( 'NONE',  ( 0.000000000000000000, 0.000000000000000000, -1.000000000000000000 ) ) ;
#70329 = DIRECTION ( 'NONE',  ( -0.000000000000000000, -1.000000000000000000, -0.000000000000000000 ) ) ;
#70330 = VERTEX_POINT ( 'NONE', #50354 ) ;
#70331 = CARTESIAN_POINT ( 'NONE',  ( 3.299999999999942979, 2.500000000000000000, 4.230127018922196669 ) ) ;
#70332 = DIRECTION ( 'NONE',  ( -0.000000000000000000, -1.000000000000000000, -0.000000000000000000 ) ) ;
#70333 = CARTESIAN_POINT ( 'NONE',  ( -15.39999999999997904, 2.500000000000000000, -0.7928203230275518987 ) ) ;
#70334 = EDGE_LOOP ( 'NONE', ( #65794, #34346 ) ) ;
#70335 = CIRCLE ( 'NONE', #47451, 0.06509327318403745899 ) ;
#70336 = ORIENTED_EDGE ( 'NONE', *, *, #104756, .T. ) ;
#70337 = ORIENTED_EDGE ( 'NONE', *, *, #97544, .F. ) ;
#70338 = CARTESIAN_POINT ( 'NONE',  ( 1.249999999999952038, 2.500000000000000000, 2.757883832488649656 ) ) ;
#70339 = CARTESIAN_POINT ( 'NONE',  ( 6.899999999999926636, 12.50000000000000000, -0.3464101615137782364 ) ) ;
#70340 = DIRECTION ( 'NONE',  ( 0.000000000000000000, 1.000000000000000000, 0.000000000000000000 ) ) ;
#70341 = FACE_BOUND ( 'NONE', #13370, .T. ) ;
#70342 = EDGE_LOOP ( 'NONE', ( #52345, #21381, #865, #30661 ) ) ;
#70343 = DIRECTION ( 'NONE',  ( 0.000000000000000000, 0.000000000000000000, 1.000000000000000000 ) ) ;
#70344 = DIRECTION ( 'NONE',  ( -0.000000000000000000, -1.000000000000000000, -0.000000000000000000 ) ) ;
#70345 = EDGE_LOOP ( 'NONE', ( #69670, #53746, #112342, #55307 ) ) ;
#70347 = AXIS2_PLACEMENT_3D ( 'NONE', #38836, #99012, #79382 ) ;
#70346 = CONICAL_SURFACE ( 'NONE', #15947, 0.1000000000000002554, 0.003490658503988666988 ) ;
#70349 = EDGE_CURVE ( 'NONE', #2854, #76377, #55769, .T. ) ;
#70348 = DIRECTION ( 'NONE',  ( -0.000000000000000000, -1.000000000000000000, -0.000000000000000000 ) ) ;
#70350 = LINE ( 'NONE', #89976, #118156 ) ;
#70351 = DIRECTION ( 'NONE',  ( -0.000000000000000000, 1.000000000000000000, -0.000000000000000000 ) ) ;
#70352 = DIRECTION ( 'NONE',  ( 0.000000000000000000, 0.000000000000000000, 1.000000000000000000 ) ) ;
#70353 = LINE ( 'NONE', #91929, #17398 ) ;
#70354 = CARTESIAN_POINT ( 'NONE',  ( -13.74999999999998757, 12.50000000000000000, -2.857883832488651521 ) ) ;
#70355 = DIRECTION ( 'NONE',  ( -0.000000000000000000, 1.000000000000000000, -0.000000000000000000 ) ) ;
#70357 = CONICAL_SURFACE ( 'NONE', #36924, 0.09999999999999982514, 0.003490658503988666988 ) ;
#70356 = CIRCLE ( 'NONE', #36923, 0.1000000000000002554 ) ;
#70358 = EDGE_CURVE ( 'NONE', #75765, #79726, #121028, .T. ) ;
#70359 = ORIENTED_EDGE ( 'NONE', *, *, #123589, .F. ) ;
#70360 = EDGE_LOOP ( 'NONE', ( #97757, #11141 ) ) ;
#70361 = VERTEX_POINT ( 'NONE', #79186 ) ;
#70362 = ORIENTED_EDGE ( 'NONE', *, *, #50183, .T. ) ;
#70363 = DIRECTION ( 'NONE',  ( -0.000000000000000000, -1.000000000000000000, -0.000000000000000000 ) ) ;
#70364 = EDGE_CURVE ( 'NONE', #28471, #118431, #111189, .T. ) ;
#70365 = DIRECTION ( 'NONE',  ( 0.000000000000000000, 0.000000000000000000, 1.000000000000000000 ) ) ;
#70366 = VERTEX_POINT ( 'NONE', #30740 ) ;
#70367 = FACE_BOUND ( 'NONE', #115929, .T. ) ;
#70368 = EDGE_CURVE ( 'NONE', #18789, #70557, #21540, .T. ) ;
#70369 = DIRECTION ( 'NONE',  ( 0.000000000000000000, 0.000000000000000000, 1.000000000000000000 ) ) ;
#70370 = CARTESIAN_POINT ( 'NONE',  ( -8.749999999999975131, 2.500000000000000000, 2.265063509461097357 ) ) ;
#70371 = ADVANCED_FACE ( 'NONE', ( #51019 ), #36995, .T. ) ;
#70372 = CARTESIAN_POINT ( 'NONE',  ( 6.849999999999930367, 2.500000000000000000, -6.148780366869526226 ) ) ;
#70373 = DIRECTION ( 'NONE',  ( -0.000000000000000000, 1.000000000000000000, -0.000000000000000000 ) ) ;
#70374 = LINE ( 'NONE', #110298, #32945 ) ;
#70375 = DIRECTION ( 'NONE',  ( 0.000000000000000000, 0.000000000000000000, 1.000000000000000000 ) ) ;
#70376 = CARTESIAN_POINT ( 'NONE',  ( -0.8500000000000395017, 2.500000000000000000, 2.165063509461097713 ) ) ;
#70377 = ADVANCED_FACE ( 'NONE', ( #128941 ), #14079, .T. ) ;
#70378 = DIRECTION ( 'NONE',  ( 0.000000000000000000, 0.000000000000000000, 1.000000000000000000 ) ) ;
#70380 = ORIENTED_EDGE ( 'NONE', *, *, #46806, .T. ) ;
#70379 = AXIS2_PLACEMENT_3D ( 'NONE', #24671, #66512, #95345 ) ;
#70381 = AXIS2_PLACEMENT_3D ( 'NONE', #104349, #86636, #65045 ) ;
#70382 = ORIENTED_EDGE ( 'NONE', *, *, #103657, .T. ) ;
#70383 = ORIENTED_EDGE ( 'NONE', *, *, #17643, .F. ) ;
#70385 = ORIENTED_EDGE ( 'NONE', *, *, #107319, .F. ) ;
#70384 = CIRCLE ( 'NONE', #61983, 0.06509327318403745899 ) ;
#70386 = ORIENTED_EDGE ( 'NONE', *, *, #79862, .F. ) ;
#70387 = EDGE_LOOP ( 'NONE', ( #65531, #25381, #83169, #34131 ) ) ;
#70388 = DIRECTION ( 'NONE',  ( 0.000000000000000000, 0.000000000000000000, 1.000000000000000000 ) ) ;
#70389 = DIRECTION ( 'NONE',  ( 0.000000000000000000, 0.000000000000000000, 1.000000000000000000 ) ) ;
#70390 = VERTEX_POINT ( 'NONE', #98795 ) ;
#70391 = FACE_OUTER_BOUND ( 'NONE', #15390, .T. ) ;
#70392 = VECTOR ( 'NONE', #82291, 1000.000000000000000 ) ;
#70393 = AXIS2_PLACEMENT_3D ( 'NONE', #109812, #100616, #19487 ) ;
#70394 = AXIS2_PLACEMENT_3D ( 'NONE', #41355, #21043, #29576 ) ;
#70395 = CARTESIAN_POINT ( 'NONE',  ( 6.899999999999928413, 12.50000000000000000, -3.918623584224389056 ) ) ;
#70396 = CARTESIAN_POINT ( 'NONE',  ( 185.0260416670080588, -6.551208109652273848, -3.782341765625003571 ) ) ;
#70397 = FACE_OUTER_BOUND ( 'NONE', #2503, .T. ) ;
#70398 = DIRECTION ( 'NONE',  ( -0.000000000000000000, -1.000000000000000000, -0.000000000000000000 ) ) ;
#70399 = CIRCLE ( 'NONE', #87109, 0.06509327318403745899 ) ;
#70400 = ORIENTED_EDGE ( 'NONE', *, *, #55826, .T. ) ;
#70401 = DIRECTION ( 'NONE',  ( 0.000000000000000000, 0.000000000000000000, -1.000000000000000000 ) ) ;
#70402 = VECTOR ( 'NONE', #77423, 1000.000000000000000 ) ;
#70403 = EDGE_LOOP ( 'NONE', ( #1483, #48046, #74749, #106186 ) ) ;
#70404 = EDGE_CURVE ( 'NONE', #53613, #48711, #119096, .T. ) ;
#70405 = CIRCLE ( 'NONE', #45375, 0.1000000000000002554 ) ;
#70406 = VERTEX_POINT ( 'NONE', #100728 ) ;
#70407 = DIRECTION ( 'NONE',  ( -0.000000000000000000, -1.000000000000000000, -0.000000000000000000 ) ) ;
#70408 = CARTESIAN_POINT ( 'NONE',  ( -5.850000000000022737, 2.500000000000000000, -6.595190528383302109 ) ) ;
#70409 = CARTESIAN_POINT ( 'NONE',  ( -2.100000000000033396, 2.500000000000000000, -3.637306695894650055 ) ) ;
#70410 = ORIENTED_EDGE ( 'NONE', *, *, #93885, .F. ) ;
#70412 = ADVANCED_FACE ( 'NONE', ( #41203 ), #61484, .T. ) ;
#70411 = ORIENTED_EDGE ( 'NONE', *, *, #31227, .F. ) ;
#70413 = DIRECTION ( 'NONE',  ( 0.000000000000000000, -0.000000000000000000, 1.000000000000000000 ) ) ;
#70414 = DIRECTION ( 'NONE',  ( -0.000000000000000000, 1.000000000000000000, -0.000000000000000000 ) ) ;
#70415 = DIRECTION ( 'NONE',  ( 0.000000000000000000, 1.000000000000000000, 0.000000000000000000 ) ) ;
#70416 = CARTESIAN_POINT ( 'NONE',  ( 5.799999999999934985, 2.500000000000000000, -4.430127018922202176 ) ) ;
#70417 = ORIENTED_EDGE ( 'NONE', *, *, #89153, .F. ) ;
#70418 = EDGE_CURVE ( 'NONE', #84654, #112423, #129050, .T. ) ;
#70419 = CARTESIAN_POINT ( 'NONE',  ( -8.950000000000009948, 2.500000000000000000, -1.818653347947326138 ) ) ;
#70420 = EDGE_CURVE ( 'NONE', #64587, #21874, #83067, .T. ) ;
#70421 = VECTOR ( 'NONE', #4352, 1000.000000000000000 ) ;
#70422 = ADVANCED_FACE ( 'NONE', ( #62765 ), #64679, .T. ) ;
#70423 = ORIENTED_EDGE ( 'NONE', *, *, #32132, .F. ) ;
#70424 = DIRECTION ( 'NONE',  ( 0.000000000000000000, 0.000000000000000000, 1.000000000000000000 ) ) ;
#70425 = ORIENTED_EDGE ( 'NONE', *, *, #123011, .F. ) ;
#70426 = CARTESIAN_POINT ( 'NONE',  ( 186.3750000000000000, 8.891194145520236347, 5.444286225454521982E-16 ) ) ;
#70427 = EDGE_CURVE ( 'NONE', #42111, #86508, #122969, .T. ) ;
#70428 = DIRECTION ( 'NONE',  ( 0.000000000000000000, 0.000000000000000000, -1.000000000000000000 ) ) ;
#70429 = CARTESIAN_POINT ( 'NONE',  ( 4.349999999999939249, 2.500000000000000000, 2.511473670974873507 ) ) ;
#70430 = CARTESIAN_POINT ( 'NONE',  ( 11.64999999999990266, 2.500000000000000000, 2.165063509461097713 ) ) ;
#70431 = VERTEX_POINT ( 'NONE', #62122 ) ;
#70432 = EDGE_CURVE ( 'NONE', #22282, #121706, #63401, .T. ) ;
#70433 = DIRECTION ( 'NONE',  ( 0.000000000000000000, 0.000000000000000000, 1.000000000000000000 ) ) ;
#70434 = EDGE_CURVE ( 'NONE', #94355, #86071, #123595, .T. ) ;
#70435 = AXIS2_PLACEMENT_3D ( 'NONE', #35945, #77784, #98713 ) ;
#70436 = AXIS2_PLACEMENT_3D ( 'NONE', #107662, #8151, #128616 ) ;
#70437 = CARTESIAN_POINT ( 'NONE',  ( -9.200000000000006395, 2.500000000000000000, 4.230127018922196669 ) ) ;
#70438 = ORIENTED_EDGE ( 'NONE', *, *, #12910, .T. ) ;
#70439 = VERTEX_POINT ( 'NONE', #73223 ) ;
#70440 = ORIENTED_EDGE ( 'NONE', *, *, #128813, .F. ) ;
#70441 = CARTESIAN_POINT ( 'NONE',  ( -5.000000000000023093, 2.500000000000000000, 5.022947341949748790 ) ) ;
#70442 = DIRECTION ( 'NONE',  ( 0.000000000000000000, -0.000000000000000000, 1.000000000000000000 ) ) ;
#70443 = FACE_OUTER_BOUND ( 'NONE', #11746, .T. ) ;
#70444 = CARTESIAN_POINT ( 'NONE',  ( -6.650000000000018119, 2.500000000000000000, -2.857883832488653741 ) ) ;
#70445 = LINE ( 'NONE', #39725, #5203 ) ;
#70448 = CONICAL_SURFACE ( 'NONE', #80916, 0.1000000000000002554, 0.003490658503988666988 ) ;
#70447 = CARTESIAN_POINT ( 'NONE',  ( 9.349999999999916156, 2.500000000000000000, -2.511473670974877948 ) ) ;
#70446 = CIRCLE ( 'NONE', #126882, 0.06509327318403745899 ) ;
#70449 = DIRECTION ( 'NONE',  ( 0.000000000000000000, 1.000000000000000000, 0.000000000000000000 ) ) ;
#70450 = CARTESIAN_POINT ( 'NONE',  ( 14.54999999999989235, 12.50000000000000000, -2.230156782645139391 ) ) ;
#70451 = DIRECTION ( 'NONE',  ( 0.000000000000000000, 1.000000000000000000, 0.000000000000000000 ) ) ;
#70453 = CONICAL_SURFACE ( 'NONE', #13995, 0.09999999999999982514, 0.003490658503988666988 ) ;
#70452 = CIRCLE ( 'NONE', #95584, 0.09999999999999999167 ) ;
#70454 = AXIS2_PLACEMENT_3D ( 'NONE', #976, #40932, #120751 ) ;
#70455 = ORIENTED_EDGE ( 'NONE', *, *, #88571, .T. ) ;
#70456 = DIRECTION ( 'NONE',  ( 0.000000000000000000, 0.000000000000000000, 1.000000000000000000 ) ) ;
#70457 = FACE_OUTER_BOUND ( 'NONE', #66332, .T. ) ;
#70458 = CARTESIAN_POINT ( 'NONE',  ( 11.84999999999990727, 2.500000000000000000, 6.148780366869520009 ) ) ;
#70459 = DIRECTION ( 'NONE',  ( 0.000000000000000000, 0.000000000000000000, -1.000000000000000000 ) ) ;
#70460 = ORIENTED_EDGE ( 'NONE', *, *, #128811, .F. ) ;
#70461 = FACE_OUTER_BOUND ( 'NONE', #7366, .T. ) ;
#70462 = ADVANCED_FACE ( 'NONE', ( #113137 ), #1564, .T. ) ;
#70463 = DIRECTION ( 'NONE',  ( -1.000000000000000000, 0.000000000000000000, 0.000000000000000000 ) ) ;
#70465 = EDGE_LOOP ( 'NONE', ( #125387, #65660 ) ) ;
#70464 = CARTESIAN_POINT ( 'NONE',  ( -0.8000000000000376810, 12.50000000000000000, -4.265033745738164406 ) ) ;
#70466 = CIRCLE ( 'NONE', #14016, 0.1000000000000002554 ) ;
#70467 = VERTEX_POINT ( 'NONE', #84322 ) ;
#70468 = AXIS2_PLACEMENT_3D ( 'NONE', #91156, #112088, #22436 ) ;
#70469 = FACE_OUTER_BOUND ( 'NONE', #71580, .T. ) ;
#70470 = ADVANCED_FACE ( 'NONE', ( #103329 ), #124257, .T. ) ;
#70471 = ORIENTED_EDGE ( 'NONE', *, *, #34425, .F. ) ;
#70472 = EDGE_LOOP ( 'NONE', ( #70234, #106134, #82413, #29074 ) ) ;
#70473 = CARTESIAN_POINT ( 'NONE',  ( -11.25000000000000000, 2.500000000000000000, 7.088010851410848190 ) ) ;
#70474 = DIRECTION ( 'NONE',  ( -0.000000000000000000, 1.000000000000000000, -0.000000000000000000 ) ) ;
#70475 = DIRECTION ( 'NONE',  ( -0.000000000000000000, -1.000000000000000000, -0.000000000000000000 ) ) ;
#70476 = CARTESIAN_POINT ( 'NONE',  ( -12.69999999999999218, 2.500000000000000000, -0.4464101615137741064 ) ) ;
#70477 = ORIENTED_EDGE ( 'NONE', *, *, #76296, .F. ) ;
#70478 = AXIS2_PLACEMENT_3D ( 'NONE', #106685, #16980, #56923 ) ;
#70479 = DIRECTION ( 'NONE',  ( 0.000000000000000000, 0.000000000000000000, 1.000000000000000000 ) ) ;
#70480 = ORIENTED_EDGE ( 'NONE', *, *, #96313, .T. ) ;
#70481 = DIRECTION ( 'NONE',  ( 0.000000000000000000, 1.000000000000000000, 0.000000000000000000 ) ) ;
#70482 = CARTESIAN_POINT ( 'NONE',  ( 17.49999999999999645, 2.413244906437269854, 3.595454705090515901 ) ) ;
#70483 = AXIS2_PLACEMENT_3D ( 'NONE', #86978, #79740, #28719 ) ;
#70484 = CARTESIAN_POINT ( 'NONE',  ( 17.49149623775398155, -2.500000000000000000, 4.292098716152740856 ) ) ;
#70485 = ORIENTED_EDGE ( 'NONE', *, *, #71089, .F. ) ;
#70486 = AXIS2_PLACEMENT_3D ( 'NONE', #43046, #23354, #33833 ) ;
#70487 = EDGE_LOOP ( 'NONE', ( #78003, #123559, #42492, #73890 ) ) ;
#70488 = EDGE_LOOP ( 'NONE', ( #102097, #50428, #2292, #35497 ) ) ;
#70489 = ORIENTED_EDGE ( 'NONE', *, *, #74654, .F. ) ;
#70490 = EDGE_LOOP ( 'NONE', ( #50632, #7869, #56763, #88211 ) ) ;
#70491 = DIRECTION ( 'NONE',  ( 0.000000000000000000, 0.000000000000000000, 1.000000000000000000 ) ) ;
#70492 = CARTESIAN_POINT ( 'NONE',  ( 8.920123399939686948, 2.500000000000000888, 8.410822907404332582 ) ) ;
#70493 = DIRECTION ( 'NONE',  ( 0.000000000000000000, 0.000000000000000000, -1.000000000000000000 ) ) ;
#70494 = FACE_BOUND ( 'NONE', #97114, .T. ) ;
#70495 = CARTESIAN_POINT ( 'NONE',  ( -4.350000000000023626, 2.500000000000000000, 6.941600689897073018 ) ) ;
#70496 = CARTESIAN_POINT ( 'NONE',  ( 186.1562500006828031, 8.891194145520236347, 5.444286225454521982E-16 ) ) ;
#70497 = DIRECTION ( 'NONE',  ( 0.000000000000000000, 0.000000000000000000, -1.000000000000000000 ) ) ;
#70498 = FACE_OUTER_BOUND ( 'NONE', #55908, .T. ) ;
#70499 = DIRECTION ( 'NONE',  ( 0.000000000000000000, 0.000000000000000000, 1.000000000000000000 ) ) ;
#70500 = PLANE ( 'NONE',  #107400 ) ;
#70501 = VECTOR ( 'NONE', #124947, 1000.000000000000000 ) ;
#70502 = DIRECTION ( 'NONE',  ( 0.000000000000000000, 0.000000000000000000, 1.000000000000000000 ) ) ;
#70503 = ADVANCED_FACE ( 'NONE', ( #111863 ), #43142, .T. ) ;
#70504 = DIRECTION ( 'NONE',  ( 0.000000000000000000, 1.000000000000000000, 0.000000000000000000 ) ) ;
#70505 = VERTEX_POINT ( 'NONE', #102668 ) ;
#70506 = ORIENTED_EDGE ( 'NONE', *, *, #72621, .F. ) ;
#70507 = EDGE_LOOP ( 'NONE', ( #26155, #69850 ) ) ;
#70508 = EDGE_LOOP ( 'NONE', ( #47820, #59477, #49364, #46946 ) ) ;
#70509 = CARTESIAN_POINT ( 'NONE',  ( 12.04999999999990834, 12.50000000000000000, 6.495190528383297135 ) ) ;
#70510 = EDGE_CURVE ( 'NONE', #7899, #62189, #89311, .T. ) ;
#70511 = CARTESIAN_POINT ( 'NONE',  ( -11.89999999999999680, 2.500000000000000000, -0.4464101615137742174 ) ) ;
#70512 = FACE_BOUND ( 'NONE', #62127, .T. ) ;
#70513 = ADVANCED_FACE ( 'NONE', ( #82417 ), #7822, .T. ) ;
#70514 = CARTESIAN_POINT ( 'NONE',  ( 1.449999999999952216, 2.500000000000000000, 1.718653347947321386 ) ) ;
#70515 = AXIS2_PLACEMENT_3D ( 'NONE', #97127, #38223, #58517 ) ;
#70516 = ADVANCED_FACE ( 'NONE', ( #121664 ), #35051, .T. ) ;
#70517 = EDGE_CURVE ( 'NONE', #82469, #87565, #22853, .T. ) ;
#70518 = VERTEX_POINT ( 'NONE', #33942 ) ;
#70519 = CARTESIAN_POINT ( 'NONE',  ( -6.650000000000015454, 2.500000000000000000, 7.188010851410848723 ) ) ;
#70520 = DIRECTION ( 'NONE',  ( 0.000000000000000000, 1.000000000000000000, 0.000000000000000000 ) ) ;
#70521 = DIRECTION ( 'NONE',  ( 0.000000000000000000, 1.000000000000000000, 0.000000000000000000 ) ) ;
#70522 = EDGE_CURVE ( 'NONE', #67262, #57482, #32025, .T. ) ;
#70523 = CARTESIAN_POINT ( 'NONE',  ( 3.349999999999945466, 2.500000000000000000, -2.265063509461101798 ) ) ;
#70524 = VERTEX_POINT ( 'NONE', #102040 ) ;
#70525 = DIRECTION ( 'NONE',  ( -4.274815082592931898E-19, -0.9999939076577903929, -0.003490651415223739937 ) ) ;
#70527 = CIRCLE ( 'NONE', #51762, 0.06509327318403743123 ) ;
#70526 = AXIS2_PLACEMENT_3D ( 'NONE', #81116, #101399, #51661 ) ;
#70528 = VERTEX_POINT ( 'NONE', #43779 ) ;
#70529 = ORIENTED_EDGE ( 'NONE', *, *, #12461, .F. ) ;
#70530 = DIRECTION ( 'NONE',  ( 0.000000000000000000, 1.000000000000000000, 0.000000000000000000 ) ) ;
#70531 = LINE ( 'NONE', #20797, #120869 ) ;
#70532 = ORIENTED_EDGE ( 'NONE', *, *, #26052, .T. ) ;
#70533 = DIRECTION ( 'NONE',  ( -0.000000000000000000, 1.000000000000000000, -0.000000000000000000 ) ) ;
#70535 = AXIS2_PLACEMENT_3D ( 'NONE', #117009, #8356, #96732 ) ;
#70534 = AXIS2_PLACEMENT_3D ( 'NONE', #107657, #12015, #70308 ) ;
#70536 = CONICAL_SURFACE ( 'NONE', #16138, 0.09999999999999982514, 0.003490658503988666988 ) ;
#70537 = FACE_OUTER_BOUND ( 'NONE', #107437, .T. ) ;
#70538 = DIRECTION ( 'NONE',  ( 0.000000000000000000, 0.000000000000000000, 1.000000000000000000 ) ) ;
#70539 = CARTESIAN_POINT ( 'NONE',  ( 7.499999999999925393, 12.50000000000000000, -3.702399969078687292 ) ) ;
#70540 = ORIENTED_EDGE ( 'NONE', *, *, #94141, .T. ) ;
#70541 = DIRECTION ( 'NONE',  ( -4.274815082592931898E-19, -0.9999939076577903929, -0.003490651415223739937 ) ) ;
#70542 = VERTEX_POINT ( 'NONE', #103973 ) ;
#70543 = DIRECTION ( 'NONE',  ( -0.000000000000000000, -1.000000000000000000, -0.000000000000000000 ) ) ;
#70544 = CIRCLE ( 'NONE', #22462, 0.1000000000000002554 ) ;
#70545 = EDGE_LOOP ( 'NONE', ( #49943, #71648 ) ) ;
#70546 = DIRECTION ( 'NONE',  ( 0.000000000000000000, 0.000000000000000000, -1.000000000000000000 ) ) ;
#70547 = ORIENTED_EDGE ( 'NONE', *, *, #67670, .T. ) ;
#70548 = DIRECTION ( 'NONE',  ( 0.000000000000000000, 1.000000000000000000, 0.000000000000000000 ) ) ;
#70549 = AXIS2_PLACEMENT_3D ( 'NONE', #105661, #15964, #55902 ) ;
#70550 = CARTESIAN_POINT ( 'NONE',  ( 14.14999999999989733, 2.500000000000000000, 1.472243186433545459 ) ) ;
#70551 = DIRECTION ( 'NONE',  ( 0.000000000000000000, -0.000000000000000000, 1.000000000000000000 ) ) ;
#70552 = DIRECTION ( 'NONE',  ( 0.000000000000000000, 0.000000000000000000, 1.000000000000000000 ) ) ;
#70554 = AXIS2_PLACEMENT_3D ( 'NONE', #125590, #105327, #126254 ) ;
#70553 = CARTESIAN_POINT ( 'NONE',  ( -6.249999999999981348, 12.50000000000000000, 6.560283801567334372 ) ) ;
#70555 = ORIENTED_EDGE ( 'NONE', *, *, #30876, .F. ) ;
#70556 = CONICAL_SURFACE ( 'NONE', #16157, 0.1000000000000002554, 0.003490658503988666988 ) ;
#70557 = VERTEX_POINT ( 'NONE', #104602 ) ;
#70558 = ORIENTED_EDGE ( 'NONE', *, *, #116220, .T. ) ;
#70559 = DIRECTION ( 'NONE',  ( -0.000000000000000000, -1.000000000000000000, -0.000000000000000000 ) ) ;
#70560 = CIRCLE ( 'NONE', #91492, 0.06509327318403745899 ) ;
#70561 = CARTESIAN_POINT ( 'NONE',  ( 108.0000000000000142, 8.500000000000000000, 2.749999999999997335 ) ) ;
#70563 = EDGE_CURVE ( 'NONE', #75085, #44948, #114435, .T. ) ;
#70562 = CARTESIAN_POINT ( 'NONE',  ( 6.899999999999926636, 2.500000000000000000, -0.4464101615137782142 ) ) ;
#70565 = ORIENTED_EDGE ( 'NONE', *, *, #93965, .T. ) ;
#70564 = EDGE_LOOP ( 'NONE', ( #72388, #33775 ) ) ;
#70566 = VERTEX_POINT ( 'NONE', #91568 ) ;
#70567 = EDGE_CURVE ( 'NONE', #43893, #38024, #1890, .T. ) ;
#70568 = CARTESIAN_POINT ( 'NONE',  ( -10.00000000000000711, 12.50000000000000000, -3.572213422710607933 ) ) ;
#70569 = CONICAL_SURFACE ( 'NONE', #41347, 0.1000000000000002554, 0.003490658503988666988 ) ;
#70570 = EDGE_CURVE ( 'NONE', #1000, #109625, #118639, .T. ) ;
#70571 = VECTOR ( 'NONE', #11453, 1000.000000000000000 ) ;
#70572 = ORIENTED_EDGE ( 'NONE', *, *, #3691, .F. ) ;
#70573 = CARTESIAN_POINT ( 'NONE',  ( 7.099999999999927702, 12.50000000000000000, -3.637306695894650055 ) ) ;
#70574 = AXIS2_PLACEMENT_3D ( 'NONE', #19218, #225, #80098 ) ;
#70575 = CIRCLE ( 'NONE', #74788, 0.06509327318403745899 ) ;
#70576 = DIRECTION ( 'NONE',  ( 0.000000000000000000, 0.000000000000000000, -1.000000000000000000 ) ) ;
#70577 = DIRECTION ( 'NONE',  ( -4.274815082592931898E-19, -0.9999939076577903929, -0.003490651415223739937 ) ) ;
#70579 = EDGE_CURVE ( 'NONE', #62109, #33637, #49623, .T. ) ;
#70578 = DIRECTION ( 'NONE',  ( 0.000000000000000000, 0.000000000000000000, 1.000000000000000000 ) ) ;
#70580 = CARTESIAN_POINT ( 'NONE',  ( 12.09999999999990195, 2.500000000000000000, 0.6928203230275494784 ) ) ;
#70581 = DIRECTION ( 'NONE',  ( 0.000000000000000000, 0.000000000000000000, -1.000000000000000000 ) ) ;
#70582 = EDGE_CURVE ( 'NONE', #84244, #77843, #126182, .T. ) ;
#70583 = AXIS2_PLACEMENT_3D ( 'NONE', #128723, #28560, #108396 ) ;
#70584 = CARTESIAN_POINT ( 'NONE',  ( 9.799999999999915445, 2.500000000000000000, -4.776537180435977525 ) ) ;
#70585 = ORIENTED_EDGE ( 'NONE', *, *, #71746, .F. ) ;
#70587 = ORIENTED_EDGE ( 'NONE', *, *, #108203, .F. ) ;
#70586 = EDGE_CURVE ( 'NONE', #39415, #26182, #5108, .T. ) ;
#70588 = LINE ( 'NONE', #95706, #23594 ) ;
#70591 = ADVANCED_FACE ( 'NONE', ( #46327 ), #108663, .T. ) ;
#70590 = CIRCLE ( 'NONE', #14131, 0.06509327318403745899 ) ;
#70589 = STYLED_ITEM ( 'NONE', ( #12614 ), #99052 ) ;
#70592 = DIRECTION ( 'NONE',  ( -0.000000000000000000, -1.000000000000000000, -0.000000000000000000 ) ) ;
#70593 = EDGE_LOOP ( 'NONE', ( #80346, #52043 ) ) ;
#70594 = ORIENTED_EDGE ( 'NONE', *, *, #95505, .T. ) ;
#70595 = CARTESIAN_POINT ( 'NONE',  ( 185.1093750003413732, 9.264065473108010111E-16, -7.564683531250000925 ) ) ;
#70596 = DIRECTION ( 'NONE',  ( 0.000000000000000000, 1.000000000000000000, 0.000000000000000000 ) ) ;
#70597 = CARTESIAN_POINT ( 'NONE',  ( 115.5000000000000000, 5.000000000000000000, -4.999999999999997335 ) ) ;
#70598 = ADVANCED_FACE ( 'NONE', ( #54849 ), #97713, .T. ) ;
#70599 = LINE ( 'NONE', #96994, #38508 ) ;
#70600 = LINE ( 'NONE', #97476, #314 ) ;
#70601 = DIRECTION ( 'NONE',  ( 0.000000000000000000, 1.000000000000000000, 0.000000000000000000 ) ) ;
#70602 = CARTESIAN_POINT ( 'NONE',  ( 4.799999999999937650, 12.50000000000000000, -3.983716857408426293 ) ) ;
#70603 = LINE ( 'NONE', #100067, #118760 ) ;
#70604 = VECTOR ( 'NONE', #128179, 1000.000000000000000 ) ;
#70605 = DIRECTION ( 'NONE',  ( 0.000000000000000000, 0.000000000000000000, -1.000000000000000000 ) ) ;
#70606 = EDGE_LOOP ( 'NONE', ( #9058, #14452, #85866, #123924 ) ) ;
#70607 = EDGE_LOOP ( 'NONE', ( #121584, #80165, #49389, #114068 ) ) ;
#70608 = ORIENTED_EDGE ( 'NONE', *, *, #2401, .F. ) ;
#70609 = EDGE_LOOP ( 'NONE', ( #87994, #38501, #125328, #7449 ) ) ;
#70610 = EDGE_LOOP ( 'NONE', ( #86934, #25373, #78303, #4679 ) ) ;
#70611 = CARTESIAN_POINT ( 'NONE',  ( -13.14999999999999147, 2.500000000000000000, 2.611473670974877148 ) ) ;
#70612 = DIRECTION ( 'NONE',  ( -0.000000000000000000, -1.000000000000000000, -0.000000000000000000 ) ) ;
#70613 = ORIENTED_EDGE ( 'NONE', *, *, #111683, .F. ) ;
#70614 = AXIS2_PLACEMENT_3D ( 'NONE', #104845, #15163, #84578 ) ;
#70615 = CARTESIAN_POINT ( 'NONE',  ( 3.149999999999946176, 2.500000000000000000, -1.918653347947325782 ) ) ;
#70617 = DIRECTION ( 'NONE',  ( -0.000000000000000000, -1.000000000000000000, -0.000000000000000000 ) ) ;
#70616 = VECTOR ( 'NONE', #102199, 1000.000000000000000 ) ;
#70618 = FACE_OUTER_BOUND ( 'NONE', #71574, .T. ) ;
#70620 = ORIENTED_EDGE ( 'NONE', *, *, #116223, .F. ) ;
#70619 = FACE_OUTER_BOUND ( 'NONE', #94418, .T. ) ;
#70621 = FACE_OUTER_BOUND ( 'NONE', #28049, .T. ) ;
#70622 = AXIS2_PLACEMENT_3D ( 'NONE', #99089, #8743, #79451 ) ;
#70623 = DIRECTION ( 'NONE',  ( 0.000000000000000000, 0.000000000000000000, 1.000000000000000000 ) ) ;
#70624 = ORIENTED_EDGE ( 'NONE', *, *, #320, .T. ) ;
#70625 = VECTOR ( 'NONE', #19037, 1000.000000000000000 ) ;
#70626 = EDGE_CURVE ( 'NONE', #105627, #106720, #95440, .T. ) ;
#70627 = EDGE_LOOP ( 'NONE', ( #109128, #71610 ) ) ;
#70628 = VERTEX_POINT ( 'NONE', #125531 ) ;
#70629 = VERTEX_POINT ( 'NONE', #75783 ) ;
#70630 = DIRECTION ( 'NONE',  ( -0.000000000000000000, -1.000000000000000000, -0.000000000000000000 ) ) ;
#70631 = CARTESIAN_POINT ( 'NONE',  ( 7.949999999999922018, 12.50000000000000000, -2.165063509461101710 ) ) ;
#70632 = CARTESIAN_POINT ( 'NONE',  ( 15.39999999999989200, 12.50000000000000000, 0.7579135962115869374 ) ) ;
#70633 = CIRCLE ( 'NONE', #116594, 0.06509327318403743123 ) ;
#70634 = FACE_OUTER_BOUND ( 'NONE', #22055, .T. ) ;
#70635 = ORIENTED_EDGE ( 'NONE', *, *, #36262, .T. ) ;
#70636 = VECTOR ( 'NONE', #22499, 1000.000000000000000 ) ;
#70637 = CARTESIAN_POINT ( 'NONE',  ( 8.749999999999918288, 2.500000000000000000, 7.088010851410848190 ) ) ;
#70638 = DIRECTION ( 'NONE',  ( 0.000000000000000000, 0.000000000000000000, 1.000000000000000000 ) ) ;
#70639 = CARTESIAN_POINT ( 'NONE',  ( 1.449999999999952216, 2.500000000000000000, 1.918653347947321564 ) ) ;
#70640 = CARTESIAN_POINT ( 'NONE',  ( -8.749999999999976907, 12.50000000000000000, -6.495190528383297135 ) ) ;
#70641 = ORIENTED_EDGE ( 'NONE', *, *, #14397, .T. ) ;
#70642 = CIRCLE ( 'NONE', #26733, 0.1000000000000002554 ) ;
#70643 = DIRECTION ( 'NONE',  ( 0.000000000000000000, 0.000000000000000000, 1.000000000000000000 ) ) ;
#70644 = VECTOR ( 'NONE', #61059, 1000.000000000000000 ) ;
#70645 = ORIENTED_EDGE ( 'NONE', *, *, #57059, .F. ) ;
#70646 = ORIENTED_EDGE ( 'NONE', *, *, #104377, .T. ) ;
#70647 = FACE_OUTER_BOUND ( 'NONE', #44023, .T. ) ;
#70648 = DIRECTION ( 'NONE',  ( -0.000000000000000000, -1.000000000000000000, -0.000000000000000000 ) ) ;
#70649 = FACE_BOUND ( 'NONE', #38143, .T. ) ;
#70650 = CIRCLE ( 'NONE', #3751, 0.06509327318403745899 ) ;
#70651 = FACE_OUTER_BOUND ( 'NONE', #81652, .T. ) ;
#70652 = CARTESIAN_POINT ( 'NONE',  ( -11.05000000000000071, 12.50000000000000000, 2.446380397790835826 ) ) ;
#70653 = AXIS2_PLACEMENT_3D ( 'NONE', #11802, #51742, #52379 ) ;
#70654 = DIRECTION ( 'NONE',  ( 0.000000000000000000, 0.000000000000000000, 1.000000000000000000 ) ) ;
#70655 = AXIS2_PLACEMENT_3D ( 'NONE', #104286, #25715, #104905 ) ;
#70656 = FACE_OUTER_BOUND ( 'NONE', #68632, .T. ) ;
#70658 = PLANE ( 'NONE',  #57131 ) ;
#70657 = AXIS2_PLACEMENT_3D ( 'NONE', #3413, #43357, #113361 ) ;
#70660 = DIRECTION ( 'NONE',  ( -0.000000000000000000, -1.000000000000000000, -0.000000000000000000 ) ) ;
#70659 = CIRCLE ( 'NONE', #59942, 0.09999999999999982514 ) ;
#70661 = VERTEX_POINT ( 'NONE', #16204 ) ;
#70662 = DIRECTION ( 'NONE',  ( -4.274815082592931898E-19, -0.9999939076577903929, -0.003490651415223739937 ) ) ;
#70663 = EDGE_CURVE ( 'NONE', #127904, #35498, #16834, .T. ) ;
#70664 = DIRECTION ( 'NONE',  ( 0.000000000000000000, -0.9999939076577903929, 0.003490651415223739937 ) ) ;
#70665 = ORIENTED_EDGE ( 'NONE', *, *, #92840, .T. ) ;
#70666 = VERTEX_POINT ( 'NONE', #56769 ) ;
#70667 = CARTESIAN_POINT ( 'NONE',  ( -6.050000000000017586, 2.500000000000000000, 6.148780366869520009 ) ) ;
#70668 = EDGE_CURVE ( 'NONE', #102850, #49354, #103989, .T. ) ;
#70669 = CARTESIAN_POINT ( 'NONE',  ( 1.249999999999952482, 12.50000000000000000, -5.802370205355749988 ) ) ;
#70670 = FACE_BOUND ( 'NONE', #108850, .T. ) ;
#70671 = ADVANCED_FACE ( 'NONE', ( #8971 ), #19440, .T. ) ;
#70672 = DIRECTION ( 'NONE',  ( 0.000000000000000000, -0.9999939076577903929, 0.003490651415223739937 ) ) ;
#70674 = CIRCLE ( 'NONE', #87383, 0.06509327318403745899 ) ;
#70673 = AXIS2_PLACEMENT_3D ( 'NONE', #45004, #126783, #54800 ) ;
#70675 = CARTESIAN_POINT ( 'NONE',  ( 6.649999999999930189, 12.50000000000000000, 7.188010851410848723 ) ) ;
#70676 = EDGE_CURVE ( 'NONE', #32793, #45295, #101932, .T. ) ;
#70677 = ADVANCED_FACE ( 'NONE', ( #68540 ), #24564, .T. ) ;
#70678 = VERTEX_POINT ( 'NONE', #48265 ) ;
#70679 = LINE ( 'NONE', #20938, #11103 ) ;
#70680 = ADVANCED_FACE ( 'NONE', ( #50216 ), #51761, .T. ) ;
#70681 = EDGE_CURVE ( 'NONE', #89857, #46113, #68465, .T. ) ;
#70682 = DIRECTION ( 'NONE',  ( 0.000000000000000000, 1.000000000000000000, 0.000000000000000000 ) ) ;
#70683 = EDGE_CURVE ( 'NONE', #51148, #97627, #41308, .T. ) ;
#70684 = ORIENTED_EDGE ( 'NONE', *, *, #73193, .T. ) ;
#70685 = DIRECTION ( 'NONE',  ( 0.000000000000000000, -0.000000000000000000, 1.000000000000000000 ) ) ;
#70686 = CARTESIAN_POINT ( 'NONE',  ( 97.50000000000000000, 0.000000000000000000, 7.500000000000000000 ) ) ;
#70687 = B_SPLINE_CURVE_WITH_KNOTS ( 'NONE', 3,
 ( #74318, #113594, #114238, #23935, #73650, #14722, #32486, #103777, #72396, #103125 ),
 .UNSPECIFIED., .F., .F.,
 ( 4, 2, 2, 2, 4 ),
 ( 4.270600654694601050E-17, 0.0006221151217586636060, 0.001244230243517284494, 0.001866345365275905383, 0.002488460487034526054 ),
 .UNSPECIFIED. ) ;
#70688 = FACE_OUTER_BOUND ( 'NONE', #46745, .T. ) ;
#70690 = EDGE_CURVE ( 'NONE', #79454, #50744, #108171, .T. ) ;
#70689 = FACE_OUTER_BOUND ( 'NONE', #34350, .T. ) ;
#70691 = EDGE_CURVE ( 'NONE', #42905, #124494, #12028, .T. ) ;
#70692 = ORIENTED_EDGE ( 'NONE', *, *, #41878, .T. ) ;
#70693 = DIRECTION ( 'NONE',  ( 0.000000000000000000, 0.000000000000000000, -1.000000000000000000 ) ) ;
#70694 = CARTESIAN_POINT ( 'NONE',  ( -13.94999999999998863, 12.50000000000000000, -1.818653347947323917 ) ) ;
#70695 = CIRCLE ( 'NONE', #76959, 0.06509327318403745899 ) ;
#70696 = CARTESIAN_POINT ( 'NONE',  ( 184.6562500006828031, 8.891194145520236347, 5.444286225454521982E-16 ) ) ;
#70697 = ORIENTED_EDGE ( 'NONE', *, *, #113666, .T. ) ;
#70698 = AXIS2_PLACEMENT_3D ( 'NONE', #74405, #105141, #106438 ) ;
#70699 = ORIENTED_EDGE ( 'NONE', *, *, #79562, .T. ) ;
#70700 = LINE ( 'NONE', #40626, #86914 ) ;
#70701 = ORIENTED_EDGE ( 'NONE', *, *, #9699, .T. ) ;
#70702 = DIRECTION ( 'NONE',  ( 0.000000000000000000, -0.9999939076577903929, 0.003490651415223739937 ) ) ;
#70703 = CARTESIAN_POINT ( 'NONE',  ( 87.49999999999998579, -4.871203238224192766, 5.733266569811710234 ) ) ;
#70704 = AXIS2_PLACEMENT_3D ( 'NONE', #9243, #98253, #58358 ) ;
#70705 = CONICAL_SURFACE ( 'NONE', #12199, 0.1000000000000000472, 0.003490658503988666988 ) ;
#70706 = FACE_OUTER_BOUND ( 'NONE', #126684, .T. ) ;
#70707 = ORIENTED_EDGE ( 'NONE', *, *, #128484, .F. ) ;
#70708 = DIRECTION ( 'NONE',  ( 0.000000000000000000, 0.000000000000000000, 1.000000000000000000 ) ) ;
#70709 = CARTESIAN_POINT ( 'NONE',  ( 12.49999999999993605, 12.50000000000000000, -2.276824562219559311E-15 ) ) ;
#70710 = LINE ( 'NONE', #100795, #50748 ) ;
#70711 = DIRECTION ( 'NONE',  ( 0.000000000000000000, 1.000000000000000000, 0.000000000000000000 ) ) ;
#70712 = DIRECTION ( 'NONE',  ( 0.000000000000000000, -0.000000000000000000, 1.000000000000000000 ) ) ;
#70713 = DIRECTION ( 'NONE',  ( -0.000000000000000000, 1.000000000000000000, -0.000000000000000000 ) ) ;
#70714 = AXIS2_PLACEMENT_3D ( 'NONE', #85620, #35884, #115719 ) ;
#70715 = EDGE_LOOP ( 'NONE', ( #45479, #43859, #85980, #92580 ) ) ;
#70717 = VERTEX_POINT ( 'NONE', #29926 ) ;
#70716 = CIRCLE ( 'NONE', #114526, 0.06509327318403745899 ) ;
#70718 = CARTESIAN_POINT ( 'NONE',  ( -1.322875655532295136, -1.500000000000000222, -5.000000000000004441 ) ) ;
#70719 = VERTEX_POINT ( 'NONE', #39762 ) ;
#70720 = CARTESIAN_POINT ( 'NONE',  ( 106.8360844680885862, 5.968126920954556880, 4.865526191718072546 ) ) ;
#70722 = ORIENTED_EDGE ( 'NONE', *, *, #73542, .T. ) ;
#70721 = EDGE_LOOP ( 'NONE', ( #125482, #100003, #43375, #71709 ) ) ;
#70723 = VERTEX_POINT ( 'NONE', #20101 ) ;
#70724 = ADVANCED_FACE ( 'NONE', ( #10280 ), #38466, .T. ) ;
#70725 = CARTESIAN_POINT ( 'NONE',  ( 87.50000000000000000, 0.7169905660283039106, -7.500000000000000000 ) ) ;
#70726 = ADVANCED_FACE ( 'NONE', ( #28637 ), #40399, .T. ) ;
#70728 = CARTESIAN_POINT ( 'NONE',  ( -11.44999999999999751, 12.50000000000000000, 2.511473670974873507 ) ) ;
#70727 = CIRCLE ( 'NONE', #97907, 0.09999999999999999167 ) ;
#70729 = PLANE ( 'NONE',  #110362 ) ;
#70730 = EDGE_CURVE ( 'NONE', #31372, #124183, #20742, .T. ) ;
#70731 = PRESENTATION_STYLE_ASSIGNMENT (( #100196 ) ) ;
#70732 = CARTESIAN_POINT ( 'NONE',  ( 4.149999999999941735, 2.500000000000000000, -7.088010851410853519 ) ) ;
#70733 = LINE ( 'NONE', #99563, #125350 ) ;
#70734 = DIRECTION ( 'NONE',  ( -4.274815082592931898E-19, -0.9999939076577903929, -0.003490651415223739937 ) ) ;
#70735 = DIRECTION ( 'NONE',  ( 0.000000000000000000, 0.000000000000000000, 1.000000000000000000 ) ) ;
#70736 = VECTOR ( 'NONE', #53871, 1000.000000000000000 ) ;
#70737 = CARTESIAN_POINT ( 'NONE',  ( -5.650000000000019895, 2.500000000000000000, 6.048780366869520364 ) ) ;
#70738 = EDGE_CURVE ( 'NONE', #108554, #46396, #66413, .T. ) ;
#70739 = DIRECTION ( 'NONE',  ( -0.000000000000000000, -1.000000000000000000, -0.000000000000000000 ) ) ;
#70740 = EDGE_CURVE ( 'NONE', #44317, #94526, #114523, .T. ) ;
#70741 = AXIS2_PLACEMENT_3D ( 'NONE', #52255, #60160, #121624 ) ;
#70742 = ORIENTED_EDGE ( 'NONE', *, *, #2182, .F. ) ;
#70743 = EDGE_CURVE ( 'NONE', #110598, #99172, #9983, .T. ) ;
#70744 = CARTESIAN_POINT ( 'NONE',  ( -14.99999999999994671, 2.500000000000000000, -0.1000000000000000056 ) ) ;
#70745 = ORIENTED_EDGE ( 'NONE', *, *, #67794, .F. ) ;
#70746 = ORIENTED_EDGE ( 'NONE', *, *, #28755, .F. ) ;
#70747 = CARTESIAN_POINT ( 'NONE',  ( -15.39999999999997904, 2.500000000000000000, -0.7928203230275518987 ) ) ;
#70748 = CIRCLE ( 'NONE', #64484, 0.06509327318403745899 ) ;
#70749 = DIRECTION ( 'NONE',  ( 0.000000000000000000, 0.000000000000000000, 1.000000000000000000 ) ) ;
#70750 = ADVANCED_FACE ( 'NONE', ( #126617 ), #125316, .T. ) ;
#70751 = DIRECTION ( 'NONE',  ( -0.000000000000000000, 1.000000000000000000, -0.000000000000000000 ) ) ;
#70752 = CARTESIAN_POINT ( 'NONE',  ( 2.899999999999945732, 12.50000000000000000, -4.330127018922201643 ) ) ;
#70753 = CARTESIAN_POINT ( 'NONE',  ( 11.64999999999990798, 2.500000000000000000, 7.188010851410848723 ) ) ;
#70754 = FACE_OUTER_BOUND ( 'NONE', #49555, .T. ) ;
#70755 = ORIENTED_EDGE ( 'NONE', *, *, #68057, .F. ) ;
#70756 = CIRCLE ( 'NONE', #31068, 0.06509327318403745899 ) ;
#70757 = ORIENTED_EDGE ( 'NONE', *, *, #119769, .T. ) ;
#70758 = DIRECTION ( 'NONE',  ( -0.000000000000000000, -1.000000000000000000, -0.000000000000000000 ) ) ;
#70759 = VERTEX_POINT ( 'NONE', #96479 ) ;
#70760 = DIRECTION ( 'NONE',  ( -1.000000000000000000, -0.000000000000000000, -0.000000000000000000 ) ) ;
#70761 = ORIENTED_EDGE ( 'NONE', *, *, #98044, .F. ) ;
#70762 = AXIS2_PLACEMENT_3D ( 'NONE', #12232, #69881, #30618 ) ;
#70763 = ADVANCED_FACE ( 'NONE', ( #77500 ), #16628, .T. ) ;
#70764 = EDGE_LOOP ( 'NONE', ( #54094, #27278 ) ) ;
#70765 = CARTESIAN_POINT ( 'NONE',  ( -3.350000000000028955, 2.500000000000000000, 7.188010851410848723 ) ) ;
#70766 = CARTESIAN_POINT ( 'NONE',  ( -3.469446951953614189E-14, 12.50000000000000000, -0.6928203230275519209 ) ) ;
#70767 = AXIS2_PLACEMENT_3D ( 'NONE', #96026, #37118, #25336 ) ;
#70768 = CARTESIAN_POINT ( 'NONE',  ( 7.949999999999925571, 2.500000000000000000, -6.395190528383301931 ) ) ;
#70769 = CARTESIAN_POINT ( 'NONE',  ( -4.350000000000027178, 12.50000000000000000, -6.841600689897077814 ) ) ;
#70770 = CARTESIAN_POINT ( 'NONE',  ( 17.50000000000000000, 0.8333333333333314830, 4.000000000000000000 ) ) ;
#70771 = EDGE_LOOP ( 'NONE', ( #86181, #7224, #119432, #38748 ) ) ;
#70772 = DIRECTION ( 'NONE',  ( 0.000000000000000000, 1.000000000000000000, 0.000000000000000000 ) ) ;
#70773 = DIRECTION ( 'NONE',  ( 0.000000000000000000, 0.000000000000000000, 1.000000000000000000 ) ) ;
#70774 = DIRECTION ( 'NONE',  ( -0.000000000000000000, -1.000000000000000000, -0.000000000000000000 ) ) ;
#70775 = DIRECTION ( 'NONE',  ( 0.000000000000000000, -0.000000000000000000, 1.000000000000000000 ) ) ;
#70776 = PLANE ( 'NONE',  #45954 ) ;
#70777 = ORIENTED_EDGE ( 'NONE', *, *, #64874, .T. ) ;
#70778 = EDGE_CURVE ( 'NONE', #8819, #65023, #35652, .T. ) ;
#70779 = VERTEX_POINT ( 'NONE', #25829 ) ;
#70780 = CIRCLE ( 'NONE', #77048, 0.1000000000000002554 ) ;
#70781 = DIRECTION ( 'NONE',  ( -0.000000000000000000, 1.000000000000000000, -0.000000000000000000 ) ) ;
#70782 = ORIENTED_EDGE ( 'NONE', *, *, #116604, .F. ) ;
#70783 = CARTESIAN_POINT ( 'NONE',  ( -11.64999999999999680, 12.50000000000000000, 7.122917578226811486 ) ) ;
#70784 = CARTESIAN_POINT ( 'NONE',  ( 115.5000000000000000, -5.000000000000000000, 2.000000000000003553 ) ) ;
#70785 = AXIS2_PLACEMENT_3D ( 'NONE', #79950, #108756, #119877 ) ;
#70786 = VECTOR ( 'NONE', #24881, 1000.000000000000000 ) ;
#70787 = AXIS2_PLACEMENT_3D ( 'NONE', #90855, #1185, #41134 ) ;
#70788 = ORIENTED_EDGE ( 'NONE', *, *, #48330, .F. ) ;
#70789 = CARTESIAN_POINT ( 'NONE',  ( 184.0833333333333144, -6.668395609140180369, 3.849999999999994760 ) ) ;
#70790 = CARTESIAN_POINT ( 'NONE',  ( -10.60000000000000142, 12.50000000000000000, 3.918623584224383727 ) ) ;
#70791 = EDGE_CURVE ( 'NONE', #5270, #119894, #99880, .T. ) ;
#70792 = CARTESIAN_POINT ( 'NONE',  ( 10.64999999999990976, 12.50000000000000000, 2.446380397790835826 ) ) ;
#70793 = DIRECTION ( 'NONE',  ( 0.000000000000000000, 1.000000000000000000, 0.000000000000000000 ) ) ;
#70794 = AXIS2_PLACEMENT_3D ( 'NONE', #102435, #94371, #122081 ) ;
#70795 = CIRCLE ( 'NONE', #62503, 0.06509327318403741736 ) ;
#70796 = CIRCLE ( 'NONE', #16492, 0.1000000000000002554 ) ;
#70797 = FACE_OUTER_BOUND ( 'NONE', #85330, .T. ) ;
#70798 = VERTEX_POINT ( 'NONE', #27750 ) ;
#70799 = CARTESIAN_POINT ( 'NONE',  ( 76.40064913000593094, 3.742349286023933796, -5.987206112383456791 ) ) ;
#70800 = DIRECTION ( 'NONE',  ( 0.000000000000000000, -0.000000000000000000, 1.000000000000000000 ) ) ;
#70801 = CONICAL_SURFACE ( 'NONE', #91733, 0.1000000000000002554, 0.003490658503988666988 ) ;
#70802 = DIRECTION ( 'NONE',  ( 0.000000000000000000, 0.000000000000000000, 1.000000000000000000 ) ) ;
#70803 = DIRECTION ( 'NONE',  ( -0.000000000000000000, 1.000000000000000000, -0.000000000000000000 ) ) ;
#70804 = AXIS2_PLACEMENT_3D ( 'NONE', #44523, #126315, #125648 ) ;
#70805 = EDGE_LOOP ( 'NONE', ( #71244, #73921 ) ) ;
#70806 = ORIENTED_EDGE ( 'NONE', *, *, #98579, .F. ) ;
#70807 = CARTESIAN_POINT ( 'NONE',  ( 6.449999999999931788, 2.500000000000000000, 6.148780366869520009 ) ) ;
#70808 = DIRECTION ( 'NONE',  ( 0.000000000000000000, 1.000000000000000000, 0.000000000000000000 ) ) ;
#70809 = FACE_OUTER_BOUND ( 'NONE', #98068, .T. ) ;
#70810 = EDGE_LOOP ( 'NONE', ( #6115, #105530 ) ) ;
#70811 = AXIS2_PLACEMENT_3D ( 'NONE', #115772, #105956, #26113 ) ;
#70812 = DIRECTION ( 'NONE',  ( 0.000000000000000000, 0.000000000000000000, -1.000000000000000000 ) ) ;
#70813 = ADVANCED_FACE ( 'NONE', ( #36945 ), #68559, .T. ) ;
#70814 = DIRECTION ( 'NONE',  ( -0.000000000000000000, -1.000000000000000000, -0.000000000000000000 ) ) ;
#70815 = AXIS2_PLACEMENT_3D ( 'NONE', #66579, #95410, #37777 ) ;
#70816 = ORIENTED_EDGE ( 'NONE', *, *, #18089, .F. ) ;
#70817 = CARTESIAN_POINT ( 'NONE',  ( 14.14999999999989377, 2.500000000000000000, -2.957883832488653830 ) ) ;
#70818 = ORIENTED_EDGE ( 'NONE', *, *, #96973, .T. ) ;
#70819 = LINE ( 'NONE', #90447, #122725 ) ;
#70820 = EDGE_CURVE ( 'NONE', #115112, #18179, #38239, .T. ) ;
#70821 = ORIENTED_EDGE ( 'NONE', *, *, #79299, .F. ) ;
#70822 = AXIS2_PLACEMENT_3D ( 'NONE', #18751, #119525, #108420 ) ;
#70823 = CARTESIAN_POINT ( 'NONE',  ( 4.349999999999941025, 2.500000000000000000, -1.818653347947326138 ) ) ;
#70824 = DIRECTION ( 'NONE',  ( 0.000000000000000000, 0.000000000000000000, 1.000000000000000000 ) ) ;
#70825 = EDGE_CURVE ( 'NONE', #108744, #4798, #112490, .T. ) ;
#70826 = ORIENTED_EDGE ( 'NONE', *, *, #86452, .F. ) ;
#70827 = EDGE_CURVE ( 'NONE', #115716, #94495, #45594, .T. ) ;
#70828 = ORIENTED_EDGE ( 'NONE', *, *, #124240, .T. ) ;
#70829 = ADVANCED_FACE ( 'NONE', ( #86674 ), #58117, .T. ) ;
#70830 = EDGE_CURVE ( 'NONE', #76876, #92053, #5855, .T. ) ;
#70831 = CARTESIAN_POINT ( 'NONE',  ( 187.2968750003414300, 8.734944146203032389, 5.348610694689227483E-16 ) ) ;
#70832 = CARTESIAN_POINT ( 'NONE',  ( 15.39999999999989200, 12.50000000000000000, -0.7579135962115917113 ) ) ;
#70833 = AXIS2_PLACEMENT_3D ( 'NONE', #37592, #127890, #46762 ) ;
#70834 = VERTEX_POINT ( 'NONE', #95861 ) ;
#70835 = DIRECTION ( 'NONE',  ( -4.274815082592931898E-19, -0.9999939076577903929, -0.003490651415223739937 ) ) ;
#70836 = CARTESIAN_POINT ( 'NONE',  ( 186.3177083336747160, 4.367472073101515306, 7.564683531250000925 ) ) ;
#70837 = AXIS2_PLACEMENT_3D ( 'NONE', #34102, #64190, #125680 ) ;
#70838 = EDGE_CURVE ( 'NONE', #53951, #53201, #95758, .T. ) ;
#70839 = CARTESIAN_POINT ( 'NONE',  ( -7.050000000000016698, 2.500000000000000000, -6.395190528383301931 ) ) ;
#70840 = FACE_OUTER_BOUND ( 'NONE', #11899, .T. ) ;
#70841 = DIRECTION ( 'NONE',  ( -0.000000000000000000, 1.000000000000000000, -0.000000000000000000 ) ) ;
#70842 = DIRECTION ( 'NONE',  ( 0.000000000000000000, 1.000000000000000000, 0.000000000000000000 ) ) ;
#70843 = CARTESIAN_POINT ( 'NONE',  ( -14.59999999999998366, 2.500000000000000000, 0.7928203230275517877 ) ) ;
#70844 = CIRCLE ( 'NONE', #20765, 0.1000000000000002554 ) ;
#70845 = EDGE_CURVE ( 'NONE', #81499, #12633, #118740, .T. ) ;
#70846 = ADVANCED_FACE ( 'NONE', ( #17934 ), #67672, .T. ) ;
#70847 = EDGE_CURVE ( 'NONE', #38354, #119869, #45486, .T. ) ;
#70848 = EDGE_LOOP ( 'NONE', ( #116248, #32948, #76259, #41973 ) ) ;
#70849 = ORIENTED_EDGE ( 'NONE', *, *, #123275, .F. ) ;
#70850 = DIRECTION ( 'NONE',  ( 0.000000000000000000, 1.000000000000000000, 0.000000000000000000 ) ) ;
#70852 = VECTOR ( 'NONE', #84979, 1000.000000000000000 ) ;
#70851 = CONICAL_SURFACE ( 'NONE', #20687, 0.09999999999999982514, 0.003490658503988666988 ) ;
#70853 = EDGE_LOOP ( 'NONE', ( #121171, #36607 ) ) ;
#70854 = DIRECTION ( 'NONE',  ( 0.000000000000000000, 0.000000000000000000, 1.000000000000000000 ) ) ;
#70855 = CARTESIAN_POINT ( 'NONE',  ( 9.599999999999914380, 2.500000000000000000, 3.637306695894644726 ) ) ;
#70856 = FACE_OUTER_BOUND ( 'NONE', #22535, .T. ) ;
#70857 = VECTOR ( 'NONE', #109655, 1000.000000000000000 ) ;
#70859 = EDGE_LOOP ( 'NONE', ( #118342, #3403 ) ) ;
#70858 = EDGE_LOOP ( 'NONE', ( #101137, #65025 ) ) ;
#70860 = FACE_BOUND ( 'NONE', #129501, .T. ) ;
#70861 = ORIENTED_EDGE ( 'NONE', *, *, #69494, .F. ) ;
#70862 = ADVANCED_FACE ( 'NONE', ( #87944 ), #3717, .T. ) ;
#70863 = DIRECTION ( 'NONE',  ( 0.000000000000000000, 1.000000000000000000, 0.000000000000000000 ) ) ;
#70864 = DIRECTION ( 'NONE',  ( 0.000000000000000000, 0.000000000000000000, 1.000000000000000000 ) ) ;
#70865 = LINE ( 'NONE', #21109, #5313 ) ;
#70868 = DIRECTION ( 'NONE',  ( 0.000000000000000000, 1.000000000000000000, 0.000000000000000000 ) ) ;
#70867 = AXIS2_PLACEMENT_3D ( 'NONE', #90758, #79027, #41045 ) ;
#70866 = VECTOR ( 'NONE', #31333, 1000.000000000000000 ) ;
#70869 = CARTESIAN_POINT ( 'NONE',  ( 184.4479166673494603, -6.668395609140176816, -3.850000000000003642 ) ) ;
#70870 = CARTESIAN_POINT ( 'NONE',  ( -4.600000000000024514, 2.500000000000000000, 5.022947341949748790 ) ) ;
#70871 = DIRECTION ( 'NONE',  ( 0.000000000000000000, 1.000000000000000000, 0.000000000000000000 ) ) ;
#70872 = FACE_OUTER_BOUND ( 'NONE', #85820, .T. ) ;
#70873 = CARTESIAN_POINT ( 'NONE',  ( 8.749999999999957367, 2.500000000000000000, 2.165063509461097713 ) ) ;
#70874 = DIRECTION ( 'NONE',  ( 0.000000000000000000, 1.000000000000000000, 0.000000000000000000 ) ) ;
#70875 = FACE_OUTER_BOUND ( 'NONE', #38547, .T. ) ;
#70876 = ORIENTED_EDGE ( 'NONE', *, *, #128484, .T. ) ;
#70877 = EDGE_LOOP ( 'NONE', ( #16734, #19893, #20955, #117042 ) ) ;
#70878 = VERTEX_POINT ( 'NONE', #86011 ) ;
#70879 = ORIENTED_EDGE ( 'NONE', *, *, #31031, .T. ) ;
#70880 = DIRECTION ( 'NONE',  ( 0.000000000000000000, 0.000000000000000000, 1.000000000000000000 ) ) ;
#70881 = VECTOR ( 'NONE', #69222, 1000.000000000000000 ) ;
#70882 = DIRECTION ( 'NONE',  ( 0.000000000000000000, -0.9999939076577903929, 0.003490651415223739937 ) ) ;
#70884 = VERTEX_POINT ( 'NONE', #68322 ) ;
#70883 = EDGE_LOOP ( 'NONE', ( #87707, #100696, #117237, #81282 ) ) ;
#70885 = ORIENTED_EDGE ( 'NONE', *, *, #67183, .F. ) ;
#70886 = DIRECTION ( 'NONE',  ( 1.000000000000000000, -0.000000000000000000, -0.000000000000000000 ) ) ;
#70887 = CIRCLE ( 'NONE', #1824, 0.06509327318403745899 ) ;
#70888 = CIRCLE ( 'NONE', #52110, 0.06509327318403745899 ) ;
#70889 = FACE_OUTER_BOUND ( 'NONE', #46904, .T. ) ;
#70890 = CARTESIAN_POINT ( 'NONE',  ( 0.6499999999999561684, 2.500000000000000000, -1.818653347947325916 ) ) ;
#70891 = DIRECTION ( 'NONE',  ( 0.000000000000000000, 0.000000000000000000, -1.000000000000000000 ) ) ;
#70892 = CARTESIAN_POINT ( 'NONE',  ( 2.499999999999945377, 12.50000000000000000, 5.022947341949748790 ) ) ;
#70893 = CARTESIAN_POINT ( 'NONE',  ( 2.500000000000002220, 2.500000000000000000, 9.000000000000003553 ) ) ;
#70894 = CARTESIAN_POINT ( 'NONE',  ( -4.400000000000025224, 2.500000000000000000, 0.3464101615137735735 ) ) ;
#70895 = ORIENTED_EDGE ( 'NONE', *, *, #30432, .F. ) ;
#70896 = AXIS2_PLACEMENT_3D ( 'NONE', #79482, #40859, #59858 ) ;
#70898 = CARTESIAN_POINT ( 'NONE',  ( 2.299999999999948752, 2.500000000000000000, 0.4464101615137735513 ) ) ;
#70897 = CIRCLE ( 'NONE', #125183, 0.06509327318403745899 ) ;
#70899 = ORIENTED_EDGE ( 'NONE', *, *, #109735, .T. ) ;
#70900 = EDGE_CURVE ( 'NONE', #49424, #26182, #39261, .T. ) ;
#70901 = CIRCLE ( 'NONE', #98073, 0.09999999999999982514 ) ;
#70902 = VERTEX_POINT ( 'NONE', #102767 ) ;
#70903 = VERTEX_POINT ( 'NONE', #13092 ) ;
#70904 = EDGE_CURVE ( 'NONE', #45275, #102428, #22619, .T. ) ;
#70905 = DIRECTION ( 'NONE',  ( -0.000000000000000000, 1.000000000000000000, -0.000000000000000000 ) ) ;
#70906 = ORIENTED_EDGE ( 'NONE', *, *, #99495, .T. ) ;
#70907 = ORIENTED_EDGE ( 'NONE', *, *, #125512, .F. ) ;
#70908 = ORIENTED_EDGE ( 'NONE', *, *, #86841, .T. ) ;
#70909 = CIRCLE ( 'NONE', #6133, 0.1000000000000000472 ) ;
#70910 = DIRECTION ( 'NONE',  ( -0.000000000000000000, -1.000000000000000000, -0.000000000000000000 ) ) ;
#70911 = EDGE_CURVE ( 'NONE', #17629, #72830, #91554, .T. ) ;
#70912 = CIRCLE ( 'NONE', #114805, 0.09999999999999999167 ) ;
#70913 = CARTESIAN_POINT ( 'NONE',  ( -10.60000000000000320, 12.50000000000000000, -4.048810130592459089 ) ) ;
#70914 = DIRECTION ( 'NONE',  ( 0.000000000000000000, -0.000000000000000000, 1.000000000000000000 ) ) ;
#70915 = PLANE ( 'NONE',  #118092 ) ;
#70916 = DIRECTION ( 'NONE',  ( -0.000000000000000000, -1.000000000000000000, -0.000000000000000000 ) ) ;
#70917 = DIRECTION ( 'NONE',  ( 0.000000000000000000, 1.000000000000000000, 0.000000000000000000 ) ) ;
#70918 = ORIENTED_EDGE ( 'NONE', *, *, #91526, .T. ) ;
#70919 = DIRECTION ( 'NONE',  ( -0.000000000000000000, 1.000000000000000000, -0.000000000000000000 ) ) ;
#70920 = ORIENTED_EDGE ( 'NONE', *, *, #127123, .T. ) ;
#70921 = CARTESIAN_POINT ( 'NONE',  ( 108.0000000000000142, 7.119691004531020440, 5.000000000000004441 ) ) ;
#70922 = DIRECTION ( 'NONE',  ( 0.000000000000000000, 0.000000000000000000, 1.000000000000000000 ) ) ;
#70923 = AXIS2_PLACEMENT_3D ( 'NONE', #67647, #85363, #106293 ) ;
#70924 = EDGE_LOOP ( 'NONE', ( #37444, #64651 ) ) ;
#70925 = PLANE ( 'NONE',  #82299 ) ;
#70926 = CARTESIAN_POINT ( 'NONE',  ( -4.400000000000028777, 2.500000000000000000, -3.983716857408426293 ) ) ;
#70927 = VERTEX_POINT ( 'NONE', #62229 ) ;
#70928 = FACE_OUTER_BOUND ( 'NONE', #97622, .T. ) ;
#70929 = EDGE_LOOP ( 'NONE', ( #104019, #95006, #111196, #92086 ) ) ;
#70930 = ORIENTED_EDGE ( 'NONE', *, *, #96224, .F. ) ;
#70931 = DIRECTION ( 'NONE',  ( -0.000000000000000000, -1.000000000000000000, -0.000000000000000000 ) ) ;
#70932 = LINE ( 'NONE', #101035, #9542 ) ;
#70933 = CARTESIAN_POINT ( 'NONE',  ( 184.3802083336747444, 4.367472073101515306, 7.564683531250000925 ) ) ;
#70935 = VECTOR ( 'NONE', #93770, 1000.000000000000000 ) ;
#70934 = CARTESIAN_POINT ( 'NONE',  ( 7.049999999999930544, 2.500000000000000000, -6.395190528383301931 ) ) ;
#70936 = DIRECTION ( 'NONE',  ( -0.000000000000000000, -1.000000000000000000, -0.000000000000000000 ) ) ;
#70937 = ORIENTED_EDGE ( 'NONE', *, *, #92327, .F. ) ;
#70938 = DIRECTION ( 'NONE',  ( 0.000000000000000000, 0.000000000000000000, 1.000000000000000000 ) ) ;
#70939 = CONICAL_SURFACE ( 'NONE', #14475, 0.1000000000000000472, 0.003490658503988666988 ) ;
#70940 = EDGE_LOOP ( 'NONE', ( #48151, #62243, #74402, #108690 ) ) ;
#70941 = FACE_OUTER_BOUND ( 'NONE', #20078, .T. ) ;
#70942 = FACE_OUTER_BOUND ( 'NONE', #85437, .T. ) ;
#70944 = VECTOR ( 'NONE', #56786, 1000.000000000000000 ) ;
#70943 = CIRCLE ( 'NONE', #64675, 0.1000000000000000056 ) ;
#70945 = EDGE_CURVE ( 'NONE', #124866, #24620, #120794, .T. ) ;
#70946 = CIRCLE ( 'NONE', #114755, 0.06509327318403745899 ) ;
#70947 = CARTESIAN_POINT ( 'NONE',  ( 185.9635416670080872, -4.367472073101519747, 7.564683531249999149 ) ) ;
#70948 = DIRECTION ( 'NONE',  ( 0.000000000000000000, 1.000000000000000000, 0.000000000000000000 ) ) ;
#70949 = DIRECTION ( 'NONE',  ( 0.000000000000000000, 0.000000000000000000, 1.000000000000000000 ) ) ;
#70950 = EDGE_CURVE ( 'NONE', #103996, #42757, #7916, .T. ) ;
#70951 = DIRECTION ( 'NONE',  ( 0.000000000000000000, 0.000000000000000000, 1.000000000000000000 ) ) ;
#70952 = FACE_OUTER_BOUND ( 'NONE', #94240, .T. ) ;
#70953 = EDGE_LOOP ( 'NONE', ( #45492, #129562, #7095, #81327 ) ) ;
#70955 = AXIS2_PLACEMENT_3D ( 'NONE', #16685, #86738, #6224 ) ;
#70954 = AXIS2_PLACEMENT_3D ( 'NONE', #27934, #67855, #98588 ) ;
#70956 = DIRECTION ( 'NONE',  ( 0.000000000000000000, 1.000000000000000000, 0.000000000000000000 ) ) ;
#70957 = DIRECTION ( 'NONE',  ( 0.000000000000000000, 1.000000000000000000, 0.000000000000000000 ) ) ;
#70958 = DIRECTION ( 'NONE',  ( 0.000000000000000000, 0.000000000000000000, 1.000000000000000000 ) ) ;
#70959 = EDGE_CURVE ( 'NONE', #93541, #46350, #83161, .T. ) ;
#70960 = ORIENTED_EDGE ( 'NONE', *, *, #3499, .T. ) ;
#70961 = DIRECTION ( 'NONE',  ( 0.000000000000000000, 1.000000000000000000, 0.000000000000000000 ) ) ;
#70962 = VERTEX_POINT ( 'NONE', #128573 ) ;
#70963 = ORIENTED_EDGE ( 'NONE', *, *, #88125, .F. ) ;
#70964 = DIRECTION ( 'NONE',  ( -0.000000000000000000, -1.000000000000000000, -0.000000000000000000 ) ) ;
#70965 = AXIS2_PLACEMENT_3D ( 'NONE', #74236, #14646, #4828 ) ;
#70966 = VERTEX_POINT ( 'NONE', #48701 ) ;
#70967 = CARTESIAN_POINT ( 'NONE',  ( 6.849999999999930367, 12.50000000000000000, -6.841600689897078702 ) ) ;
#70968 = DIRECTION ( 'NONE',  ( -0.000000000000000000, 1.000000000000000000, -0.000000000000000000 ) ) ;
#70969 = DIRECTION ( 'NONE',  ( -1.000000000000000000, -0.000000000000000000, 0.000000000000000000 ) ) ;
#70970 = ORIENTED_EDGE ( 'NONE', *, *, #35487, .T. ) ;
#70971 = AXIS2_PLACEMENT_3D ( 'NONE', #55496, #46306, #86220 ) ;
#70972 = DIRECTION ( 'NONE',  ( -0.000000000000000000, 1.000000000000000000, -0.000000000000000000 ) ) ;
#70973 = AXIS2_PLACEMENT_3D ( 'NONE', #15531, #24088, #26022 ) ;
#70974 = EDGE_CURVE ( 'NONE', #53869, #28525, #64356, .T. ) ;
#70975 = DIRECTION ( 'NONE',  ( 0.000000000000000000, 0.000000000000000000, 1.000000000000000000 ) ) ;
#70976 = CARTESIAN_POINT ( 'NONE',  ( -7.900000000000014566, 2.500000000000000000, -3.537306695894649966 ) ) ;
#70977 = VECTOR ( 'NONE', #35536, 1000.000000000000000 ) ;
#70978 = ORIENTED_EDGE ( 'NONE', *, *, #49464, .T. ) ;
#70980 = VECTOR ( 'NONE', #45308, 1000.000000000000000 ) ;
#70979 = AXIS2_PLACEMENT_3D ( 'NONE', #3142, #5050, #75096 ) ;
#70981 = EDGE_CURVE ( 'NONE', #78540, #81821, #29068, .T. ) ;
#70982 = CONICAL_SURFACE ( 'NONE', #8277, 0.09999999999999982514, 0.003490658503988666988 ) ;
#70983 = ORIENTED_EDGE ( 'NONE', *, *, #66565, .F. ) ;
#70984 = ORIENTED_EDGE ( 'NONE', *, *, #71988, .T. ) ;
#70985 = CARTESIAN_POINT ( 'NONE',  ( 7.499999999999925393, 2.500000000000000000, 5.022947341949748790 ) ) ;
#70986 = DIRECTION ( 'NONE',  ( 0.000000000000000000, -0.000000000000000000, 1.000000000000000000 ) ) ;
#70987 = DIRECTION ( 'NONE',  ( 0.000000000000000000, 0.000000000000000000, -1.000000000000000000 ) ) ;
#70988 = ADVANCED_FACE ( 'NONE', ( #73311 ), #35140, .T. ) ;
#70989 = EDGE_CURVE ( 'NONE', #3435, #112348, #38905, .T. ) ;
#70990 = FACE_BOUND ( 'NONE', #3572, .T. ) ;
#70991 = ORIENTED_EDGE ( 'NONE', *, *, #43244, .F. ) ;
#70992 = ADVANCED_FACE ( 'NONE', ( #89259 ), #32784, .T. ) ;
#70994 = ADVANCED_FACE ( 'NONE', ( #22945 ), #93609, .T. ) ;
#70993 = CIRCLE ( 'NONE', #35500, 0.09999999999999982514 ) ;
#70995 = CARTESIAN_POINT ( 'NONE',  ( 7.949999999999922018, 2.500000000000000000, 6.495190528383297135 ) ) ;
#70996 = CARTESIAN_POINT ( 'NONE',  ( 108.0000000000000142, 7.119691004531020440, 5.000000000000004441 ) ) ;
#70997 = ORIENTED_EDGE ( 'NONE', *, *, #95095, .T. ) ;
#70999 = CARTESIAN_POINT ( 'NONE',  ( 1.049999999999953637, 2.500000000000000000, -1.818653347947326138 ) ) ;
#70998 = VECTOR ( 'NONE', #59867, 1000.000000000000000 ) ;
#71000 = CARTESIAN_POINT ( 'NONE',  ( 17.27572160909454624, 2.230096426605390203, 5.047229640871625733 ) ) ;
#71001 = AXIS2_PLACEMENT_3D ( 'NONE', #6073, #76125, #64363 ) ;
#71002 = ADVANCED_FACE ( 'NONE', ( #68970 ), #85286, .T. ) ;
#71003 = DIRECTION ( 'NONE',  ( 0.000000000000000000, 0.000000000000000000, 1.000000000000000000 ) ) ;
#71004 = LINE ( 'NONE', #89980, #90593 ) ;
#71005 = DIRECTION ( 'NONE',  ( 0.000000000000000000, 0.000000000000000000, 1.000000000000000000 ) ) ;
#71006 = ADVANCED_FACE ( 'NONE', ( #69614 ), #11818, .F. ) ;
#71007 = CARTESIAN_POINT ( 'NONE',  ( 1.849999999999951017, 2.500000000000000000, -6.148780366869526226 ) ) ;
#71008 = CARTESIAN_POINT ( 'NONE',  ( -10.00000000000000355, 2.500000000000000000, 3.637306695894644726 ) ) ;
#71009 = EDGE_CURVE ( 'NONE', #129161, #53205, #121768, .T. ) ;
#71010 = EDGE_CURVE ( 'NONE', #1265, #122865, #125002, .T. ) ;
#71011 = ORIENTED_EDGE ( 'NONE', *, *, #41295, .T. ) ;
#71012 = ORIENTED_EDGE ( 'NONE', *, *, #56774, .F. ) ;
#71013 = EDGE_LOOP ( 'NONE', ( #61724, #111691 ) ) ;
#71014 = EDGE_LOOP ( 'NONE', ( #71130, #110113 ) ) ;
#71015 = AXIS2_PLACEMENT_3D ( 'NONE', #4063, #72187, #113376 ) ;
#71016 = CARTESIAN_POINT ( 'NONE',  ( -11.84999999999999609, 2.500000000000000000, 1.918653347947321564 ) ) ;
#71017 = DIRECTION ( 'NONE',  ( 0.000000000000000000, 0.000000000000000000, 1.000000000000000000 ) ) ;
#71018 = EDGE_LOOP ( 'NONE', ( #125808, #17976, #73368, #111726 ) ) ;
#71019 = ADVANCED_FACE ( 'NONE', ( #108880 ), #60281, .T. ) ;
#71020 = FACE_BOUND ( 'NONE', #84728, .T. ) ;
#71021 = EDGE_CURVE ( 'NONE', #112869, #68306, #89499, .T. ) ;
#71022 = CARTESIAN_POINT ( 'NONE',  ( -10.20000000000000639, 12.50000000000000000, -3.983716857408421852 ) ) ;
#71023 = CARTESIAN_POINT ( 'NONE',  ( 16.55763164795904174, 0.1615198509490234913, 6.093150836621333610 ) ) ;
#71024 = FACE_OUTER_BOUND ( 'NONE', #23782, .T. ) ;
#71025 = DIRECTION ( 'NONE',  ( 0.000000000000000000, 0.000000000000000000, 1.000000000000000000 ) ) ;
#71026 = CARTESIAN_POINT ( 'NONE',  ( 184.5000000000000000, 0.000000000000000000, 7.700000000000000178 ) ) ;
#71027 = DIRECTION ( 'NONE',  ( 0.000000000000000000, 0.000000000000000000, 1.000000000000000000 ) ) ;
#71028 = DIRECTION ( 'NONE',  ( 0.000000000000000000, -0.000000000000000000, 1.000000000000000000 ) ) ;
#71029 = LINE ( 'NONE', #61205, #18330 ) ;
#71030 = VERTEX_POINT ( 'NONE', #6382 ) ;
#71031 = EDGE_LOOP ( 'NONE', ( #106462, #111852 ) ) ;
#71032 = EDGE_LOOP ( 'NONE', ( #3909, #113623, #14104, #12112 ) ) ;
#71033 = EDGE_LOOP ( 'NONE', ( #120668, #24953 ) ) ;
#71034 = VERTEX_POINT ( 'NONE', #124909 ) ;
#71035 = ORIENTED_EDGE ( 'NONE', *, *, #79610, .F. ) ;
#71036 = DIRECTION ( 'NONE',  ( -0.000000000000000000, -1.000000000000000000, -0.000000000000000000 ) ) ;
#71037 = AXIS2_PLACEMENT_3D ( 'NONE', #61411, #31310, #52224 ) ;
#71038 = ORIENTED_EDGE ( 'NONE', *, *, #97204, .F. ) ;
#71041 = AXIS2_PLACEMENT_3D ( 'NONE', #8193, #56635, #6882 ) ;
#71040 = CARTESIAN_POINT ( 'NONE',  ( 17.91370874550469949, 0.4812889678260096615, 4.985910759330083764 ) ) ;
#71039 = CIRCLE ( 'NONE', #75235, 0.06509327318403745899 ) ;
#71042 = CARTESIAN_POINT ( 'NONE',  ( 16.31212831497983728, -1.499999999999935163, 6.358242018216646585 ) ) ;
#71043 = DIRECTION ( 'NONE',  ( -4.274815082592931898E-19, -0.9999939076577903929, -0.003490651415223739937 ) ) ;
#71044 = CARTESIAN_POINT ( 'NONE',  ( -12.69999999999999218, 12.50000000000000000, -0.2813168883297366696 ) ) ;
#71045 = AXIS2_PLACEMENT_3D ( 'NONE', #71497, #39497, #20480 ) ;
#71046 = ORIENTED_EDGE ( 'NONE', *, *, #109891, .F. ) ;
#71047 = FACE_OUTER_BOUND ( 'NONE', #43952, .T. ) ;
#71049 = CIRCLE ( 'NONE', #102445, 0.1000000000000002554 ) ;
#71048 = AXIS2_PLACEMENT_3D ( 'NONE', #62418, #121971, #102332 ) ;
#71050 = ORIENTED_EDGE ( 'NONE', *, *, #79539, .F. ) ;
#71051 = ADVANCED_FACE ( 'NONE', ( #5121 ), #16846, .T. ) ;
#71052 = ORIENTED_EDGE ( 'NONE', *, *, #54505, .F. ) ;
#71053 = CARTESIAN_POINT ( 'NONE',  ( 9.799999999999913669, 2.500000000000000000, 4.676537180435972552 ) ) ;
#71054 = EDGE_CURVE ( 'NONE', #88657, #110215, #127163, .T. ) ;
#71055 = DIRECTION ( 'NONE',  ( -4.274815082592931898E-19, -0.9999939076577903929, -0.003490651415223739937 ) ) ;
#71056 = DIRECTION ( 'NONE',  ( 0.000000000000000000, 0.000000000000000000, 1.000000000000000000 ) ) ;
#71057 = VERTEX_POINT ( 'NONE', #126194 ) ;
#71058 = EDGE_LOOP ( 'NONE', ( #16818, #129210 ) ) ;
#71059 = DIRECTION ( 'NONE',  ( 0.000000000000000000, 1.000000000000000000, 0.000000000000000000 ) ) ;
#71060 = CARTESIAN_POINT ( 'NONE',  ( -0.4000000000000396572, 12.50000000000000000, 4.265033745738159077 ) ) ;
#71061 = DIRECTION ( 'NONE',  ( -0.000000000000000000, -1.000000000000000000, -0.000000000000000000 ) ) ;
#71062 = LINE ( 'NONE', #21981, #123524 ) ;
#71063 = ORIENTED_EDGE ( 'NONE', *, *, #67434, .F. ) ;
#71064 = CARTESIAN_POINT ( 'NONE',  ( -11.89999999999999503, 12.50000000000000000, 4.676537180435972552 ) ) ;
#71065 = ORIENTED_EDGE ( 'NONE', *, *, #119741, .T. ) ;
#71066 = DIRECTION ( 'NONE',  ( 0.000000000000000000, 1.000000000000000000, 0.000000000000000000 ) ) ;
#71067 = CONICAL_SURFACE ( 'NONE', #52191, 0.09999999999999999167, 0.003490658503988666988 ) ;
#71068 = CONICAL_SURFACE ( 'NONE', #104507, 0.09999999999999982514, 0.003490658503988666988 ) ;
#71069 = ORIENTED_EDGE ( 'NONE', *, *, #100070, .F. ) ;
#71070 = CARTESIAN_POINT ( 'NONE',  ( 8.749999999999918288, 2.500000000000000000, 7.288010851410849256 ) ) ;
#71071 = DIRECTION ( 'NONE',  ( 0.000000000000000000, 0.000000000000000000, -1.000000000000000000 ) ) ;
#71072 = DIRECTION ( 'NONE',  ( -4.274815082592931898E-19, -0.9999939076577903929, -0.003490651415223739937 ) ) ;
#71073 = DIRECTION ( 'NONE',  ( 0.000000000000000000, 0.000000000000000000, 1.000000000000000000 ) ) ;
#71074 = ORIENTED_EDGE ( 'NONE', *, *, #71618, .T. ) ;
#71075 = VECTOR ( 'NONE', #126443, 1000.000000000000000 ) ;
#71076 = DIRECTION ( 'NONE',  ( 0.000000000000000000, -0.9999939076577903929, 0.003490651415223739937 ) ) ;
#71077 = CARTESIAN_POINT ( 'NONE',  ( -12.09999999999999609, 2.500000000000000000, -3.737306695894647035 ) ) ;
#71078 = ORIENTED_EDGE ( 'NONE', *, *, #99521, .T. ) ;
#71079 = ORIENTED_EDGE ( 'NONE', *, *, #82673, .F. ) ;
#71080 = ORIENTED_EDGE ( 'NONE', *, *, #89942, .F. ) ;
#71081 = CARTESIAN_POINT ( 'NONE',  ( -3.550000000000030909, 2.500000000000000000, -6.941600689897078347 ) ) ;
#71082 = CARTESIAN_POINT ( 'NONE',  ( 9.549999999999918998, 2.500000000000000000, -6.395190528383301931 ) ) ;
#71083 = CARTESIAN_POINT ( 'NONE',  ( 21.23528140090950700, 2.699413673072311948, 2.293764360948889802 ) ) ;
#71084 = CARTESIAN_POINT ( 'NONE',  ( 6.849999999999929479, 12.50000000000000000, -1.818653347947326138 ) ) ;
#71085 = AXIS2_PLACEMENT_3D ( 'NONE', #45889, #18832, #465 ) ;
#71086 = DIRECTION ( 'NONE',  ( -0.000000000000000000, -1.000000000000000000, -0.000000000000000000 ) ) ;
#71087 = DIRECTION ( 'NONE',  ( 0.000000000000000000, -0.9999939076577903929, 0.003490651415223739937 ) ) ;
#71089 = EDGE_CURVE ( 'NONE', #58995, #56093, #8009, .T. ) ;
#71088 = AXIS2_PLACEMENT_3D ( 'NONE', #44716, #23785, #84633 ) ;
#71090 = CONICAL_SURFACE ( 'NONE', #20913, 0.1000000000000000472, 0.003490658503988666988 ) ;
#71091 = CARTESIAN_POINT ( 'NONE',  ( -9.600000000000008527, 2.500000000000000000, -3.637306695894645614 ) ) ;
#71092 = DIRECTION ( 'NONE',  ( 0.000000000000000000, 1.000000000000000000, 0.000000000000000000 ) ) ;
#71093 = DIRECTION ( 'NONE',  ( -0.000000000000000000, 1.000000000000000000, -0.000000000000000000 ) ) ;
#71094 = CONICAL_SURFACE ( 'NONE', #100349, 0.1000000000000002554, 0.003490658503988666988 ) ;
#71095 = ORIENTED_EDGE ( 'NONE', *, *, #43347, .T. ) ;
#71096 = AXIS2_PLACEMENT_3D ( 'NONE', #87718, #96900, #77268 ) ;
#71097 = FACE_OUTER_BOUND ( 'NONE', #49734, .T. ) ;
#71098 = ADVANCED_FACE ( 'NONE', ( #25394 ), #56033, .T. ) ;
#71100 = EDGE_CURVE ( 'NONE', #31773, #108185, #115063, .T. ) ;
#71099 = DIRECTION ( 'NONE',  ( -0.000000000000000000, -1.000000000000000000, -0.000000000000000000 ) ) ;
#71101 = CARTESIAN_POINT ( 'NONE',  ( 7.299999999999926104, 12.50000000000000000, 4.676537180435972552 ) ) ;
#71102 = DIRECTION ( 'NONE',  ( 0.000000000000000000, 0.000000000000000000, -1.000000000000000000 ) ) ;
#71103 = ORIENTED_EDGE ( 'NONE', *, *, #114606, .F. ) ;
#71104 = DIRECTION ( 'NONE',  ( 0.000000000000000000, -0.9999939076577903929, 0.003490651415223739937 ) ) ;
#71105 = DIRECTION ( 'NONE',  ( 0.000000000000000000, 0.000000000000000000, -1.000000000000000000 ) ) ;
#71107 = EDGE_LOOP ( 'NONE', ( #17850, #110159, #50409, #90835 ) ) ;
#71106 = LINE ( 'NONE', #62591, #8642 ) ;
#71108 = EDGE_CURVE ( 'NONE', #121536, #62517, #45073, .T. ) ;
#71109 = ORIENTED_EDGE ( 'NONE', *, *, #71993, .F. ) ;
#71110 = DIRECTION ( 'NONE',  ( -0.000000000000000000, -1.000000000000000000, -0.000000000000000000 ) ) ;
#71111 = ORIENTED_EDGE ( 'NONE', *, *, #103507, .T. ) ;
#71112 = ORIENTED_EDGE ( 'NONE', *, *, #86285, .T. ) ;
#71113 = CARTESIAN_POINT ( 'NONE',  ( 0.1999999999999636513, 2.500000000000000000, -0.3464101615137760715 ) ) ;
#71114 = CONICAL_SURFACE ( 'NONE', #14667, 0.1000000000000002554, 0.003490658503988666988 ) ;
#71115 = AXIS2_PLACEMENT_3D ( 'NONE', #71871, #81043, #42410 ) ;
#71116 = DIRECTION ( 'NONE',  ( -0.000000000000000000, 1.000000000000000000, -0.000000000000000000 ) ) ;
#71117 = DIRECTION ( 'NONE',  ( -4.274815082592931898E-19, -0.9999939076577903929, -0.003490651415223739937 ) ) ;
#71118 = DIRECTION ( 'NONE',  ( -0.000000000000000000, 1.000000000000000000, -0.000000000000000000 ) ) ;
#71119 = ORIENTED_EDGE ( 'NONE', *, *, #76762, .F. ) ;
#71121 = CIRCLE ( 'NONE', #115025, 0.1000000000000000472 ) ;
#71120 = CONICAL_SURFACE ( 'NONE', #106709, 0.1000000000000002554, 0.003490658503988666988 ) ;
#71122 = CARTESIAN_POINT ( 'NONE',  ( 184.6666666666666856, -6.668395609140176816, -3.850000000000003642 ) ) ;
#71123 = VERTEX_POINT ( 'NONE', #64054 ) ;
#71124 = DIRECTION ( 'NONE',  ( 0.000000000000000000, 0.000000000000000000, 1.000000000000000000 ) ) ;
#71125 = PLANE ( 'NONE',  #94786 ) ;
#71126 = VERTEX_POINT ( 'NONE', #124267 ) ;
#71127 = ADVANCED_FACE ( 'NONE', ( #95451 ), #65324, .T. ) ;
#71128 = ORIENTED_EDGE ( 'NONE', *, *, #17003, .F. ) ;
#71129 = ORIENTED_EDGE ( 'NONE', *, *, #38352, .F. ) ;
#71130 = ORIENTED_EDGE ( 'NONE', *, *, #61256, .T. ) ;
#71131 = FACE_OUTER_BOUND ( 'NONE', #42709, .T. ) ;
#71132 = CARTESIAN_POINT ( 'NONE',  ( 13.80679872452938994, 2.500000000000256684, 7.946844944430235813 ) ) ;
#71133 = FACE_OUTER_BOUND ( 'NONE', #88574, .T. ) ;
#71134 = ADVANCED_FACE ( 'NONE', ( #26709 ), #99968, .T. ) ;
#71135 = FACE_BOUND ( 'NONE', #85392, .T. ) ;
#71136 = DIRECTION ( 'NONE',  ( 0.000000000000000000, 0.000000000000000000, -1.000000000000000000 ) ) ;
#71137 = CARTESIAN_POINT ( 'NONE',  ( 187.2343750003414016, 8.734944146203032389, 5.348610694689227483E-16 ) ) ;
#71138 = EDGE_CURVE ( 'NONE', #17715, #53612, #81188, .T. ) ;
#71139 = DIRECTION ( 'NONE',  ( -0.000000000000000000, 1.000000000000000000, -0.000000000000000000 ) ) ;
#71140 = CARTESIAN_POINT ( 'NONE',  ( -10.20000000000000284, 2.500000000000000000, -0.4464101615137782142 ) ) ;
#71141 = ADVANCED_FACE ( 'NONE', ( #55530 ), #93698, .T. ) ;
#71142 = DIRECTION ( 'NONE',  ( 0.000000000000000000, 0.000000000000000000, 1.000000000000000000 ) ) ;
#71143 = EDGE_CURVE ( 'NONE', #37773, #72830, #4450, .T. ) ;
#71144 = DIRECTION ( 'NONE',  ( -4.274815082592931898E-19, -0.9999939076577903929, -0.003490651415223739937 ) ) ;
#71145 = EDGE_CURVE ( 'NONE', #105143, #109777, #56151, .T. ) ;
#71146 = DIRECTION ( 'NONE',  ( -1.000000000000000000, -0.000000000000000000, -0.000000000000000000 ) ) ;
#71147 = EDGE_CURVE ( 'NONE', #13968, #57293, #122952, .T. ) ;
#71148 = CIRCLE ( 'NONE', #121324, 0.06509327318403745899 ) ;
#71149 = CIRCLE ( 'NONE', #44061, 0.1000000000000002554 ) ;
#71150 = CARTESIAN_POINT ( 'NONE',  ( -9.600000000000008527, 12.50000000000000000, -5.022947341949749678 ) ) ;
#71151 = EDGE_CURVE ( 'NONE', #5884, #113395, #74925, .T. ) ;
#71152 = ORIENTED_EDGE ( 'NONE', *, *, #49877, .F. ) ;
#71153 = VERTEX_POINT ( 'NONE', #14292 ) ;
#71154 = ORIENTED_EDGE ( 'NONE', *, *, #73101, .F. ) ;
#71155 = EDGE_LOOP ( 'NONE', ( #103449, #45236 ) ) ;
#71156 = ORIENTED_EDGE ( 'NONE', *, *, #4298, .T. ) ;
#71157 = CARTESIAN_POINT ( 'NONE',  ( 129.5000000000000000, -1.500000000000000000, 2.598076211353316900 ) ) ;
#71158 = LINE ( 'NONE', #41724, #117676 ) ;
#71159 = VERTEX_POINT ( 'NONE', #54238 ) ;
#71160 = FACE_BOUND ( 'NONE', #6360, .T. ) ;
#71162 = ADVANCED_FACE ( 'NONE', ( #84336 ), #41503, .T. ) ;
#71161 = CIRCLE ( 'NONE', #31467, 0.06509327318403745899 ) ;
#71163 = DIRECTION ( 'NONE',  ( 0.000000000000000000, 1.000000000000000000, 0.000000000000000000 ) ) ;
#71164 = VERTEX_POINT ( 'NONE', #14913 ) ;
#71165 = CARTESIAN_POINT ( 'NONE',  ( -6.700000000000019718, 2.500000000000000000, -0.1000000000000023925 ) ) ;
#71166 = CARTESIAN_POINT ( 'NONE',  ( 7.899999999999924860, 12.50000000000000000, -5.022947341949754119 ) ) ;
#71167 = DIRECTION ( 'NONE',  ( 0.000000000000000000, -0.000000000000000000, 1.000000000000000000 ) ) ;
#71168 = CARTESIAN_POINT ( 'NONE',  ( -2.499999999999996003, 12.50000000000000000, -2.276824562219559311E-15 ) ) ;
#71169 = VERTEX_POINT ( 'NONE', #54860 ) ;
#71170 = CARTESIAN_POINT ( 'NONE',  ( -10.65000000000000213, 2.500000000000000000, 6.741600689897071952 ) ) ;
#71171 = AXIS2_PLACEMENT_3D ( 'NONE', #114564, #15716, #24909 ) ;
#71172 = AXIS2_PLACEMENT_3D ( 'NONE', #16845, #43790, #75165 ) ;
#71173 = ORIENTED_EDGE ( 'NONE', *, *, #46458, .T. ) ;
#71174 = ORIENTED_EDGE ( 'NONE', *, *, #77187, .F. ) ;
#71175 = CARTESIAN_POINT ( 'NONE',  ( -5.200000000000025935, 12.50000000000000000, -3.983716857408426293 ) ) ;
#71176 = LINE ( 'NONE', #75675, #62305 ) ;
#71177 = ORIENTED_EDGE ( 'NONE', *, *, #91674, .T. ) ;
#71178 = DIRECTION ( 'NONE',  ( 0.000000000000000000, 0.000000000000000000, 1.000000000000000000 ) ) ;
#71179 = AXIS2_PLACEMENT_3D ( 'NONE', #117793, #28803, #78558 ) ;
#71180 = CARTESIAN_POINT ( 'NONE',  ( 0.8499999999999557909, 2.500000000000000000, -6.395190528383301931 ) ) ;
#71181 = DIRECTION ( 'NONE',  ( 0.000000000000000000, 1.000000000000000000, 0.000000000000000000 ) ) ;
#71182 = CARTESIAN_POINT ( 'NONE',  ( 179.5000000000000000, -1.375000000000000222, 6.000000000000000000 ) ) ;
#71183 = CIRCLE ( 'NONE', #29431, 0.09999999999999982514 ) ;
#71184 = CARTESIAN_POINT ( 'NONE',  ( 3.749999999999978684, 12.50000000000000000, -2.165063509461101710 ) ) ;
#71185 = ORIENTED_EDGE ( 'NONE', *, *, #37876, .T. ) ;
#71186 = DIRECTION ( 'NONE',  ( 0.000000000000000000, 0.000000000000000000, 1.000000000000000000 ) ) ;
#71187 = ORIENTED_EDGE ( 'NONE', *, *, #22168, .T. ) ;
#71188 = DIRECTION ( 'NONE',  ( -0.000000000000000000, 1.000000000000000000, -0.000000000000000000 ) ) ;
#71189 = ORIENTED_EDGE ( 'NONE', *, *, #16594, .T. ) ;
#71190 = EDGE_CURVE ( 'NONE', #68306, #112869, #43545, .T. ) ;
#71191 = DIRECTION ( 'NONE',  ( 0.000000000000000000, 0.000000000000000000, 1.000000000000000000 ) ) ;
#71192 = EDGE_LOOP ( 'NONE', ( #117993, #56360 ) ) ;
#71193 = CARTESIAN_POINT ( 'NONE',  ( 9.599999999999917932, 12.50000000000000000, -0.06509327318403970719 ) ) ;
#71194 = DIRECTION ( 'NONE',  ( 0.000000000000000000, 0.000000000000000000, 1.000000000000000000 ) ) ;
#71195 = SHAPE_REPRESENTATION ( 'coupler', ( #108296 ), #66615 ) ;
#71196 = CARTESIAN_POINT ( 'NONE',  ( 9.149999999999920419, 2.500000000000000000, 1.372243186433545370 ) ) ;
#71197 = CARTESIAN_POINT ( 'NONE',  ( 2.699999999999945555, 2.500000000000000000, 3.883716857408420431 ) ) ;
#71198 = DIRECTION ( 'NONE',  ( 0.000000000000000000, -0.9999939076577903929, 0.003490651415223739937 ) ) ;
#71199 = ORIENTED_EDGE ( 'NONE', *, *, #126441, .F. ) ;
#71200 = ORIENTED_EDGE ( 'NONE', *, *, #69404, .T. ) ;
#71201 = EDGE_CURVE ( 'NONE', #1964, #91540, #106225, .T. ) ;
#71202 = ORIENTED_EDGE ( 'NONE', *, *, #57527, .F. ) ;
#71203 = FACE_OUTER_BOUND ( 'NONE', #62300, .T. ) ;
#71204 = DIRECTION ( 'NONE',  ( 0.000000000000000000, 0.000000000000000000, 1.000000000000000000 ) ) ;
#71206 = FACE_OUTER_BOUND ( 'NONE', #120953, .T. ) ;
#71205 = CIRCLE ( 'NONE', #16876, 0.06509327318403745899 ) ;
#71208 = EDGE_LOOP ( 'NONE', ( #52868, #84972 ) ) ;
#71207 = ORIENTED_EDGE ( 'NONE', *, *, #76052, .T. ) ;
#71209 = ORIENTED_EDGE ( 'NONE', *, *, #37876, .F. ) ;
#71210 = VECTOR ( 'NONE', #102319, 1000.000000000000000 ) ;
#71211 = AXIS2_PLACEMENT_3D ( 'NONE', #10817, #80246, #1028 ) ;
#71212 = DIRECTION ( 'NONE',  ( 1.000000000000000000, 0.000000000000000000, 0.000000000000000000 ) ) ;
#71213 = ORIENTED_EDGE ( 'NONE', *, *, #34484, .T. ) ;
#71214 = DIRECTION ( 'NONE',  ( 0.000000000000000000, 1.000000000000000000, 0.000000000000000000 ) ) ;
#71215 = DIRECTION ( 'NONE',  ( 0.000000000000000000, 0.000000000000000000, 1.000000000000000000 ) ) ;
#71216 = DIRECTION ( 'NONE',  ( 0.000000000000000000, 0.000000000000000000, 1.000000000000000000 ) ) ;
#71217 = DIRECTION ( 'NONE',  ( -1.000000000000000000, 0.000000000000000000, 0.000000000000000000 ) ) ;
#71218 = DIRECTION ( 'NONE',  ( -0.000000000000000000, 1.000000000000000000, -0.000000000000000000 ) ) ;
#71219 = CARTESIAN_POINT ( 'NONE',  ( 1.049999999999952083, 12.50000000000000000, 6.841600689897072485 ) ) ;
#71220 = DIRECTION ( 'NONE',  ( 0.000000000000000000, 0.000000000000000000, 1.000000000000000000 ) ) ;
#71221 = CONICAL_SURFACE ( 'NONE', #85873, 0.1000000000000002554, 0.003490658503988666988 ) ;
#71222 = CARTESIAN_POINT ( 'NONE',  ( -2.300000000000033573, 12.50000000000000000, 0.3464101615137735735 ) ) ;
#71223 = ORIENTED_EDGE ( 'NONE', *, *, #10919, .F. ) ;
#71224 = LINE ( 'NONE', #103277, #19478 ) ;
#71225 = CARTESIAN_POINT ( 'NONE',  ( 6.449999999999933564, 12.50000000000000000, -6.776507416713040577 ) ) ;
#71226 = EDGE_LOOP ( 'NONE', ( #69302, #106797 ) ) ;
#71227 = ORIENTED_EDGE ( 'NONE', *, *, #116238, .F. ) ;
#71228 = CARTESIAN_POINT ( 'NONE',  ( 186.5052083336747444, -6.551208109652278289, 3.782341765624995134 ) ) ;
#71229 = DIRECTION ( 'NONE',  ( 0.000000000000000000, 1.000000000000000000, 0.000000000000000000 ) ) ;
#71230 = CARTESIAN_POINT ( 'NONE',  ( -11.89999999999999680, 2.500000000000000000, 0.2464101615137776757 ) ) ;
#71231 = DIRECTION ( 'NONE',  ( 0.000000000000000000, 1.000000000000000000, 0.000000000000000000 ) ) ;
#71232 = DIRECTION ( 'NONE',  ( 0.000000000000000000, 1.000000000000000000, 0.000000000000000000 ) ) ;
#71233 = EDGE_CURVE ( 'NONE', #64042, #39804, #108479, .T. ) ;
#71234 = DIRECTION ( 'NONE',  ( 0.000000000000000000, 0.000000000000000000, 1.000000000000000000 ) ) ;
#71235 = DIRECTION ( 'NONE',  ( -0.000000000000000000, -1.000000000000000000, -0.000000000000000000 ) ) ;
#71236 = PLANE ( 'NONE',  #1767 ) ;
#71237 = CARTESIAN_POINT ( 'NONE',  ( 2.949999999999945111, 2.500000000000000000, 2.065063509461097624 ) ) ;
#71238 = CIRCLE ( 'NONE', #14772, 0.06509327318403745899 ) ;
#71239 = ADVANCED_FACE ( 'NONE', ( #47639 ), #64448, .T. ) ;
#71240 = ORIENTED_EDGE ( 'NONE', *, *, #94273, .T. ) ;
#71241 = ORIENTED_EDGE ( 'NONE', *, *, #46752, .F. ) ;
#71242 = ORIENTED_EDGE ( 'NONE', *, *, #1382, .F. ) ;
#71243 = EDGE_CURVE ( 'NONE', #66158, #102525, #58218, .T. ) ;
#71244 = ORIENTED_EDGE ( 'NONE', *, *, #17313, .F. ) ;
#71245 = ORIENTED_EDGE ( 'NONE', *, *, #34112, .T. ) ;
#71246 = EDGE_CURVE ( 'NONE', #74727, #885, #37814, .T. ) ;
#71247 = CARTESIAN_POINT ( 'NONE',  ( 10.64999999999990976, 2.500000000000000000, 2.611473670974873151 ) ) ;
#71248 = CARTESIAN_POINT ( 'NONE',  ( -8.950000000000006395, 12.50000000000000000, 6.776507416713035248 ) ) ;
#71249 = CIRCLE ( 'NONE', #102723, 0.1000000000000002554 ) ;
#71250 = ORIENTED_EDGE ( 'NONE', *, *, #4506, .F. ) ;
#71251 = DIRECTION ( 'NONE',  ( 0.000000000000000000, 0.000000000000000000, 1.000000000000000000 ) ) ;
#71252 = CARTESIAN_POINT ( 'NONE',  ( -8.350000000000012079, 2.500000000000000000, 2.857883832488649301 ) ) ;
#71253 = EDGE_CURVE ( 'NONE', #79119, #91313, #31038, .T. ) ;
#71254 = CARTESIAN_POINT ( 'NONE',  ( 10.79999999999991012, 2.500000000000000000, -4.230127018922201998 ) ) ;
#71256 = ORIENTED_EDGE ( 'NONE', *, *, #121216, .F. ) ;
#71255 = CARTESIAN_POINT ( 'NONE',  ( 195.0000000000000000, 4.898587196589412829E-16, 4.000000000000000000 ) ) ;
#71257 = EDGE_CURVE ( 'NONE', #17899, #125450, #119580, .T. ) ;
#71258 = DIRECTION ( 'NONE',  ( -0.000000000000000000, 1.000000000000000000, -0.000000000000000000 ) ) ;
#71259 = LINE ( 'NONE', #111846, #52016 ) ;
#71260 = CONICAL_SURFACE ( 'NONE', #87970, 0.1000000000000002554, 0.003490658503988666988 ) ;
#71261 = VERTEX_POINT ( 'NONE', #8984 ) ;
#71262 = AXIS2_PLACEMENT_3D ( 'NONE', #100586, #91423, #22702 ) ;
#71263 = ORIENTED_EDGE ( 'NONE', *, *, #6056, .T. ) ;
#71264 = ORIENTED_EDGE ( 'NONE', *, *, #58466, .T. ) ;
#71265 = ORIENTED_EDGE ( 'NONE', *, *, #121482, .T. ) ;
#71266 = DIRECTION ( 'NONE',  ( 0.000000000000000000, 1.000000000000000000, 0.000000000000000000 ) ) ;
#71267 = AXIS2_PLACEMENT_3D ( 'NONE', #68555, #38485, #117635 ) ;
#71268 = DIRECTION ( 'NONE',  ( 0.000000000000000000, 0.000000000000000000, 1.000000000000000000 ) ) ;
#71269 = CARTESIAN_POINT ( 'NONE',  ( 9.149999999999915090, 2.500000000000000000, 6.495190528383297135 ) ) ;
#71270 = ORIENTED_EDGE ( 'NONE', *, *, #128148, .T. ) ;
#71271 = VECTOR ( 'NONE', #71645, 1000.000000000000000 ) ;
#71272 = DIRECTION ( 'NONE',  ( 0.000000000000000000, 1.000000000000000000, 0.000000000000000000 ) ) ;
#71273 = EDGE_LOOP ( 'NONE', ( #47614, #508, #111022, #126467 ) ) ;
#71274 = DIRECTION ( 'NONE',  ( 0.000000000000000000, -0.9999939076577903929, 0.003490651415223739937 ) ) ;
#71275 = DIRECTION ( 'NONE',  ( -0.000000000000000000, 1.000000000000000000, -0.000000000000000000 ) ) ;
#71276 = FACE_OUTER_BOUND ( 'NONE', #31204, .T. ) ;
#71277 = DIRECTION ( 'NONE',  ( 0.000000000000000000, 0.000000000000000000, 1.000000000000000000 ) ) ;
#71278 = ORIENTED_EDGE ( 'NONE', *, *, #111965, .T. ) ;
#71279 = ORIENTED_EDGE ( 'NONE', *, *, #17211, .F. ) ;
#71280 = ORIENTED_EDGE ( 'NONE', *, *, #76671, .T. ) ;
#71281 = CARTESIAN_POINT ( 'NONE',  ( -11.69999999999999929, 2.500000000000000000, 1.734723475976807094E-15 ) ) ;
#71282 = CARTESIAN_POINT ( 'NONE',  ( 13.09999999999989839, 2.500000000000000000, 0.3464101615137735735 ) ) ;
#71283 = FACE_BOUND ( 'NONE', #101077, .T. ) ;
#71284 = FACE_OUTER_BOUND ( 'NONE', #88622, .T. ) ;
#71285 = DIRECTION ( 'NONE',  ( 0.000000000000000000, 1.000000000000000000, 0.000000000000000000 ) ) ;
#71286 = EDGE_CURVE ( 'NONE', #85304, #103182, #1746, .T. ) ;
#71287 = DIRECTION ( 'NONE',  ( 0.000000000000000000, 0.000000000000000000, 1.000000000000000000 ) ) ;
#71289 = ADVANCED_FACE ( 'NONE', ( #107842 ), #28962, .T. ) ;
#71288 = CIRCLE ( 'NONE', #56697, 0.1000000000000002554 ) ;
#71290 = AXIS2_PLACEMENT_3D ( 'NONE', #58383, #98276, #88454 ) ;
#71291 = EDGE_CURVE ( 'NONE', #82484, #27176, #66499, .T. ) ;
#71293 = CONICAL_SURFACE ( 'NONE', #65016, 0.09999999999999982514, 0.003490658503988666988 ) ;
#71292 = DIRECTION ( 'NONE',  ( 0.000000000000000000, -0.000000000000000000, 1.000000000000000000 ) ) ;
#71294 = EDGE_CURVE ( 'NONE', #81079, #89242, #12212, .T. ) ;
#71295 = CARTESIAN_POINT ( 'NONE',  ( 8.349999999999923261, 12.50000000000000000, 2.857883832488649301 ) ) ;
#71296 = VERTEX_POINT ( 'NONE', #79668 ) ;
#71297 = EDGE_CURVE ( 'NONE', #114385, #23310, #7694, .T. ) ;
#71298 = FACE_OUTER_BOUND ( 'NONE', #98772, .T. ) ;
#71299 = AXIS2_PLACEMENT_3D ( 'NONE', #62277, #72097, #81882 ) ;
#71300 = CARTESIAN_POINT ( 'NONE',  ( 9.549999999999918998, 2.500000000000000000, 2.165063509461097713 ) ) ;
#71301 = ADVANCED_FACE ( 'NONE', ( #69858 ), #112584, .T. ) ;
#71302 = VERTEX_POINT ( 'NONE', #56779 ) ;
#71303 = EDGE_LOOP ( 'NONE', ( #121915, #91643 ) ) ;
#71304 = AXIS2_PLACEMENT_3D ( 'NONE', #109541, #86664, #27738 ) ;
#71305 = DIRECTION ( 'NONE',  ( 0.000000000000000000, 0.000000000000000000, -1.000000000000000000 ) ) ;
#71306 = CARTESIAN_POINT ( 'NONE',  ( 17.49862860983209600, -2.500000000000000000, 4.081131818001135336 ) ) ;
#71307 = FACE_BOUND ( 'NONE', #26518, .T. ) ;
#71308 = DIRECTION ( 'NONE',  ( 0.000000000000000000, 0.000000000000000000, -1.000000000000000000 ) ) ;
#71309 = EDGE_CURVE ( 'NONE', #36155, #43212, #93561, .T. ) ;
#71310 = EDGE_CURVE ( 'NONE', #13136, #12586, #127493, .T. ) ;
#71311 = ORIENTED_EDGE ( 'NONE', *, *, #74503, .F. ) ;
#71312 = LINE ( 'NONE', #40611, #19422 ) ;
#71313 = DIRECTION ( 'NONE',  ( -0.000000000000000000, -1.000000000000000000, -0.000000000000000000 ) ) ;
#71314 = VERTEX_POINT ( 'NONE', #78402 ) ;
#71315 = CARTESIAN_POINT ( 'NONE',  ( 10.64999999999990976, 2.500000000000000000, -6.248780366869526759 ) ) ;
#71316 = DIRECTION ( 'NONE',  ( 0.000000000000000000, 0.000000000000000000, 1.000000000000000000 ) ) ;
#71317 = AXIS2_PLACEMENT_3D ( 'NONE', #28059, #37868, #28708 ) ;
#71318 = CARTESIAN_POINT ( 'NONE',  ( -8.300000000000009592, 2.500000000000000000, 4.330127018922196314 ) ) ;
#71319 = DIRECTION ( 'NONE',  ( 0.000000000000000000, 0.000000000000000000, 1.000000000000000000 ) ) ;
#71320 = VECTOR ( 'NONE', #123707, 1000.000000000000000 ) ;
#71321 = CONICAL_SURFACE ( 'NONE', #104764, 0.1000000000000000472, 0.003490658503988666988 ) ;
#71322 = ORIENTED_EDGE ( 'NONE', *, *, #107356, .F. ) ;
#71323 = CARTESIAN_POINT ( 'NONE',  ( -14.34999999999998543, 2.500000000000000000, -2.511473670974875727 ) ) ;
#71324 = DIRECTION ( 'NONE',  ( 0.000000000000000000, 0.000000000000000000, -1.000000000000000000 ) ) ;
#71325 = DIRECTION ( 'NONE',  ( 0.000000000000000000, -0.9999939076577903929, 0.003490651415223739937 ) ) ;
#71326 = VERTEX_POINT ( 'NONE', #37185 ) ;
#71327 = ORIENTED_EDGE ( 'NONE', *, *, #82245, .T. ) ;
#71328 = FACE_OUTER_BOUND ( 'NONE', #75501, .T. ) ;
#71329 = AXIS2_PLACEMENT_3D ( 'NONE', #95592, #26207, #66120 ) ;
#71330 = VERTEX_POINT ( 'NONE', #77099 ) ;
#71331 = CARTESIAN_POINT ( 'NONE',  ( -6.900000000000019007, 2.500000000000000000, -0.3464101615137783474 ) ) ;
#71332 = AXIS2_PLACEMENT_3D ( 'NONE', #80428, #30042, #128900 ) ;
#71333 = DIRECTION ( 'NONE',  ( 0.000000000000000000, 0.000000000000000000, 1.000000000000000000 ) ) ;
#71334 = DIRECTION ( 'NONE',  ( -0.000000000000000000, 1.000000000000000000, -0.000000000000000000 ) ) ;
#71335 = EDGE_LOOP ( 'NONE', ( #61849, #51057 ) ) ;
#71336 = CARTESIAN_POINT ( 'NONE',  ( 0.8499999999999536815, 2.500000000000000000, 6.395190528383296602 ) ) ;
#71337 = PLANE ( 'NONE',  #66482 ) ;
#71338 = DIRECTION ( 'NONE',  ( -4.274815082592931898E-19, -0.9999939076577903929, -0.003490651415223739937 ) ) ;
#71339 = CARTESIAN_POINT ( 'NONE',  ( 6.649999999999929301, 12.50000000000000000, 6.560283801567334372 ) ) ;
#71340 = CARTESIAN_POINT ( 'NONE',  ( -6.700000000000016165, 2.500000000000000000, 4.330127018922196314 ) ) ;
#71341 = PLANE ( 'NONE',  #110053 ) ;
#71342 = VERTEX_POINT ( 'NONE', #116996 ) ;
#71343 = CIRCLE ( 'NONE', #65079, 0.06509327318403745899 ) ;
#71344 = EDGE_CURVE ( 'NONE', #86952, #14798, #37282, .T. ) ;
#71345 = ORIENTED_EDGE ( 'NONE', *, *, #110312, .T. ) ;
#71346 = DIRECTION ( 'NONE',  ( -0.000000000000000000, 1.000000000000000000, -0.000000000000000000 ) ) ;
#71347 = ORIENTED_EDGE ( 'NONE', *, *, #22674, .F. ) ;
#71348 = DIRECTION ( 'NONE',  ( 0.000000000000000000, 0.000000000000000000, -1.000000000000000000 ) ) ;
#71350 = ORIENTED_EDGE ( 'NONE', *, *, #96267, .F. ) ;
#71349 = VERTEX_POINT ( 'NONE', #90773 ) ;
#71351 = ORIENTED_EDGE ( 'NONE', *, *, #76511, .F. ) ;
#71352 = CARTESIAN_POINT ( 'NONE',  ( 13.74999999999989697, 12.50000000000000000, 2.922977105672686982 ) ) ;
#71353 = AXIS2_PLACEMENT_3D ( 'NONE', #89495, #119583, #29938 ) ;
#71354 = CARTESIAN_POINT ( 'NONE',  ( -9.150000000000009237, 2.500000000000000000, 1.572243186433545548 ) ) ;
#71355 = CARTESIAN_POINT ( 'NONE',  ( -13.09999999999999254, 12.50000000000000000, 0.2813168883297403888 ) ) ;
#71356 = FILL_AREA_STYLE_COLOUR ( '', #120907 ) ;
#71357 = DIRECTION ( 'NONE',  ( 0.000000000000000000, 1.000000000000000000, 0.000000000000000000 ) ) ;
#71358 = VECTOR ( 'NONE', #79386, 1000.000000000000000 ) ;
#71359 = CIRCLE ( 'NONE', #14900, 0.1000000000000002554 ) ;
#71360 = DIRECTION ( 'NONE',  ( 0.000000000000000000, -0.9999939076577903929, 0.003490651415223739937 ) ) ;
#71361 = CARTESIAN_POINT ( 'NONE',  ( 21.24754738303277080, -0.7337760880902354232, 4.182111650399362723 ) ) ;
#71362 = DIRECTION ( 'NONE',  ( 0.000000000000000000, 0.000000000000000000, 1.000000000000000000 ) ) ;
#71363 = DIRECTION ( 'NONE',  ( -0.000000000000000000, -1.000000000000000000, -0.000000000000000000 ) ) ;
#71364 = CARTESIAN_POINT ( 'NONE',  ( -15.39999999999997904, 2.500000000000000000, -0.6928203230275519209 ) ) ;
#71365 = ORIENTED_EDGE ( 'NONE', *, *, #106183, .F. ) ;
#71366 = DIRECTION ( 'NONE',  ( 0.000000000000000000, 0.000000000000000000, 1.000000000000000000 ) ) ;
#71367 = VERTEX_POINT ( 'NONE', #12205 ) ;
#71368 = ORIENTED_EDGE ( 'NONE', *, *, #116654, .T. ) ;
#71369 = DIRECTION ( 'NONE',  ( -0.000000000000000000, 1.000000000000000000, -0.000000000000000000 ) ) ;
#71370 = CARTESIAN_POINT ( 'NONE',  ( -9.150000000000009237, 2.500000000000000000, -1.472243186433550122 ) ) ;
#71371 = CARTESIAN_POINT ( 'NONE',  ( 9.799999999999913669, 2.500000000000000000, 4.676537180435972552 ) ) ;
#71372 = DIRECTION ( 'NONE',  ( 0.000000000000000000, 1.000000000000000000, 0.000000000000000000 ) ) ;
#71373 = CARTESIAN_POINT ( 'NONE',  ( -10.80000000000000249, 2.500000000000000000, -4.430127018922197735 ) ) ;
#71374 = VECTOR ( 'NONE', #70023, 1000.000000000000000 ) ;
#71375 = DIRECTION ( 'NONE',  ( 0.000000000000000000, 0.000000000000000000, 1.000000000000000000 ) ) ;
#71376 = VERTEX_POINT ( 'NONE', #102527 ) ;
#71377 = CONICAL_SURFACE ( 'NONE', #67242, 0.09999999999999999167, 0.003490658503988666988 ) ;
#71378 = CIRCLE ( 'NONE', #83991, 0.06509327318403745899 ) ;
#71379 = ORIENTED_EDGE ( 'NONE', *, *, #7684, .F. ) ;
#71380 = ADVANCED_FACE ( 'NONE', ( #32529 ), #66594, .T. ) ;
#71381 = VECTOR ( 'NONE', #103332, 1000.000000000000000 ) ;
#71382 = ORIENTED_EDGE ( 'NONE', *, *, #2026, .F. ) ;
#71384 = DIRECTION ( 'NONE',  ( 0.000000000000000000, 0.000000000000000000, 1.000000000000000000 ) ) ;
#71383 = CONICAL_SURFACE ( 'NONE', #83914, 0.1000000000000002554, 0.003490658503988666988 ) ;
#71385 = EDGE_LOOP ( 'NONE', ( #69304, #45495, #117282, #3595 ) ) ;
#71386 = VECTOR ( 'NONE', #96468, 1000.000000000000000 ) ;
#71387 = EDGE_CURVE ( 'NONE', #3248, #92137, #111710, .T. ) ;
#71388 = VERTEX_POINT ( 'NONE', #121506 ) ;
#71389 = ADVANCED_FACE ( 'NONE', ( #71792 ), #105232, .T. ) ;
#71390 = CARTESIAN_POINT ( 'NONE',  ( 187.5000000000000000, 0.000000000000000000, 0.000000000000000000 ) ) ;
#71391 = DIRECTION ( 'NONE',  ( 0.000000000000000000, 0.000000000000000000, -1.000000000000000000 ) ) ;
#71392 = CARTESIAN_POINT ( 'NONE',  ( -9.350000000000004974, 12.50000000000000000, 6.841600689897072485 ) ) ;
#71393 = CARTESIAN_POINT ( 'NONE',  ( -9.600000000000008527, 2.500000000000000000, -4.230127018922197557 ) ) ;
#71394 = EDGE_CURVE ( 'NONE', #2839, #51372, #72870, .T. ) ;
#71395 = CARTESIAN_POINT ( 'NONE',  ( -2.100000000000033840, 2.500000000000000000, 5.022947341949748790 ) ) ;
#71397 = VERTEX_POINT ( 'NONE', #64534 ) ;
#71396 = EDGE_CURVE ( 'NONE', #74917, #118649, #95293, .T. ) ;
#71398 = DIRECTION ( 'NONE',  ( -0.000000000000000000, -1.000000000000000000, -0.000000000000000000 ) ) ;
#71399 = FACE_OUTER_BOUND ( 'NONE', #104197, .T. ) ;
#71400 = ADVANCED_FACE ( 'NONE', ( #46186 ), #129421, .T. ) ;
#71401 = DIRECTION ( 'NONE',  ( 0.000000000000000000, 0.000000000000000000, -1.000000000000000000 ) ) ;
#71402 = EDGE_CURVE ( 'NONE', #36999, #102877, #14354, .T. ) ;
#71403 = CARTESIAN_POINT ( 'NONE',  ( 6.249999999999967137, 12.50000000000000000, -2.165063509461101710 ) ) ;
#71404 = DIRECTION ( 'NONE',  ( 0.000000000000000000, 0.000000000000000000, 1.000000000000000000 ) ) ;
#71405 = ORIENTED_EDGE ( 'NONE', *, *, #90882, .T. ) ;
#71406 = ORIENTED_EDGE ( 'NONE', *, *, #15872, .T. ) ;
#71407 = ORIENTED_EDGE ( 'NONE', *, *, #70959, .F. ) ;
#71408 = DIRECTION ( 'NONE',  ( 0.000000000000000000, 0.000000000000000000, 1.000000000000000000 ) ) ;
#71409 = ADVANCED_FACE ( 'NONE', ( #75630 ), #114277, .T. ) ;
#71410 = EDGE_LOOP ( 'NONE', ( #33210, #79400, #113683, #8380 ) ) ;
#71411 = CARTESIAN_POINT ( 'NONE',  ( -12.09999999999999432, 2.500000000000000000, 4.922947341949748257 ) ) ;
#71412 = AXIS2_PLACEMENT_3D ( 'NONE', #113107, #84295, #45033 ) ;
#71413 = CARTESIAN_POINT ( 'NONE',  ( -9.350000000000004974, 2.500000000000000000, 6.148780366869520897 ) ) ;
#71414 = AXIS2_PLACEMENT_3D ( 'NONE', #82017, #36156, #64946 ) ;
#71415 = ORIENTED_EDGE ( 'NONE', *, *, #31519, .F. ) ;
#71416 = LINE ( 'NONE', #39430, #114254 ) ;
#71417 = DIRECTION ( 'NONE',  ( 0.000000000000000000, -0.9999939076577903929, 0.003490651415223739937 ) ) ;
#71418 = DIRECTION ( 'NONE',  ( -0.000000000000000000, -1.000000000000000000, -0.000000000000000000 ) ) ;
#71419 = FACE_OUTER_BOUND ( 'NONE', #121693, .T. ) ;
#71420 = AXIS2_PLACEMENT_3D ( 'NONE', #58896, #38629, #109933 ) ;
#71421 = AXIS2_PLACEMENT_3D ( 'NONE', #40976, #82825, #32452 ) ;
#71422 = CIRCLE ( 'NONE', #48455, 0.1000000000000000472 ) ;
#71423 = DIRECTION ( 'NONE',  ( -0.000000000000000000, -1.000000000000000000, -0.000000000000000000 ) ) ;
#71424 = CIRCLE ( 'NONE', #34083, 0.1000000000000002554 ) ;
#71425 = CIRCLE ( 'NONE', #14974, 0.06509327318403745899 ) ;
#71426 = ORIENTED_EDGE ( 'NONE', *, *, #33329, .T. ) ;
#71427 = ORIENTED_EDGE ( 'NONE', *, *, #12456, .F. ) ;
#71428 = CARTESIAN_POINT ( 'NONE',  ( 187.0833333333333144, -6.668395609140180369, 3.849999999999994760 ) ) ;
#71429 = FACE_OUTER_BOUND ( 'NONE', #91751, .T. ) ;
#71430 = LINE ( 'NONE', #70169, #42970 ) ;
#71431 = AXIS2_PLACEMENT_3D ( 'NONE', #1087, #2350, #12180 ) ;
#71433 = CARTESIAN_POINT ( 'NONE',  ( 0.1999999999999627909, 2.500000000000000000, 0.4464101615137758272 ) ) ;
#71432 = AXIS2_PLACEMENT_3D ( 'NONE', #46046, #85938, #6718 ) ;
#71434 = ORIENTED_EDGE ( 'NONE', *, *, #78524, .F. ) ;
#71435 = CONICAL_SURFACE ( 'NONE', #31761, 0.1000000000000000472, 0.003490658503988666988 ) ;
#71436 = CIRCLE ( 'NONE', #79860, 0.1000000000000002554 ) ;
#71437 = ADVANCED_FACE ( 'NONE', ( #35727 ), #33175, .T. ) ;
#71438 = EDGE_LOOP ( 'NONE', ( #57776, #3188 ) ) ;
#71439 = ADVANCED_FACE ( 'NONE', ( #25907 ), #16394, .T. ) ;
#71440 = DIRECTION ( 'NONE',  ( -4.274815082592931898E-19, -0.9999939076577903929, -0.003490651415223739937 ) ) ;
#71441 = CARTESIAN_POINT ( 'NONE',  ( -6.071532165918824830E-15, 12.50000000000000000, -4.330127018922201643 ) ) ;
#71442 = CIRCLE ( 'NONE', #119475, 0.06509327318403745899 ) ;
#71443 = CARTESIAN_POINT ( 'NONE',  ( -6.700000000000019718, 12.50000000000000000, -0.06509327318403980434 ) ) ;
#71444 = ADVANCED_FACE ( 'NONE', ( #73700 ), #106312, .T. ) ;
#71445 = CARTESIAN_POINT ( 'NONE',  ( 12.94999999999990337, 2.500000000000000000, 2.165063509461097713 ) ) ;
#71446 = EDGE_LOOP ( 'NONE', ( #74110, #46723 ) ) ;
#71447 = DIRECTION ( 'NONE',  ( 0.000000000000000000, 1.000000000000000000, 0.000000000000000000 ) ) ;
#71448 = EDGE_CURVE ( 'NONE', #10245, #114788, #125193, .T. ) ;
#71449 = CARTESIAN_POINT ( 'NONE',  ( 4.349999999999941025, 2.500000000000000000, -1.918653347947326004 ) ) ;
#71450 = CONICAL_SURFACE ( 'NONE', #75651, 0.1000000000000002554, 0.003490658503988666988 ) ;
#71451 = VERTEX_POINT ( 'NONE', #63899 ) ;
#71452 = DIRECTION ( 'NONE',  ( -0.000000000000000000, -1.000000000000000000, -0.000000000000000000 ) ) ;
#71453 = ADVANCED_FACE ( 'NONE', ( #36389 ), #95939, .T. ) ;
#71454 = ORIENTED_EDGE ( 'NONE', *, *, #100494, .T. ) ;
#71455 = DIRECTION ( 'NONE',  ( 0.000000000000000000, 0.000000000000000000, 1.000000000000000000 ) ) ;
#71456 = EDGE_CURVE ( 'NONE', #4651, #5028, #100061, .T. ) ;
#71457 = EDGE_CURVE ( 'NONE', #109551, #114610, #12311, .T. ) ;
#71458 = EDGE_LOOP ( 'NONE', ( #122901, #49977 ) ) ;
#71459 = EDGE_CURVE ( 'NONE', #21383, #44658, #49895, .T. ) ;
#71460 = ORIENTED_EDGE ( 'NONE', *, *, #76917, .T. ) ;
#71461 = DIRECTION ( 'NONE',  ( 0.000000000000000000, 0.000000000000000000, -1.000000000000000000 ) ) ;
#71462 = CARTESIAN_POINT ( 'NONE',  ( 2.500000000000002220, 2.500000000000000000, -8.999999999999998224 ) ) ;
#71463 = ORIENTED_EDGE ( 'NONE', *, *, #125351, .F. ) ;
#71464 = VERTEX_POINT ( 'NONE', #94000 ) ;
#71465 = PLANE ( 'NONE',  #39418 ) ;
#71466 = DIRECTION ( 'NONE',  ( -4.274815082592931898E-19, -0.9999939076577903929, -0.003490651415223739937 ) ) ;
#71467 = ORIENTED_EDGE ( 'NONE', *, *, #95807, .F. ) ;
#71468 = EDGE_CURVE ( 'NONE', #67282, #74692, #84168, .T. ) ;
#71469 = CARTESIAN_POINT ( 'NONE',  ( 187.0885416670080872, -6.551208109652273848, -3.782341765625003571 ) ) ;
#71470 = CARTESIAN_POINT ( 'NONE',  ( 184.0677083336747160, -4.367472073101514418, -7.564683531250002702 ) ) ;
#71471 = DIRECTION ( 'NONE',  ( 0.000000000000000000, -0.9999939076577903929, 0.003490651415223739937 ) ) ;
#71472 = CIRCLE ( 'NONE', #84086, 5.000000000000004441 ) ;
#71473 = DIRECTION ( 'NONE',  ( 0.000000000000000000, 1.000000000000000000, 0.000000000000000000 ) ) ;
#71474 = DIRECTION ( 'NONE',  ( 0.000000000000000000, 1.000000000000000000, 0.000000000000000000 ) ) ;
#71475 = CIRCLE ( 'NONE', #121554, 0.06509327318403745899 ) ;
#71476 = CIRCLE ( 'NONE', #38041, 0.06509327318403745899 ) ;
#71477 = CARTESIAN_POINT ( 'NONE',  ( -14.34999999999998543, 2.500000000000000000, 2.411473670974877415 ) ) ;
#71478 = CARTESIAN_POINT ( 'NONE',  ( -10.40000000000000213, 2.500000000000000000, 5.122947341949749323 ) ) ;
#71479 = CIRCLE ( 'NONE', #111182, 0.09999999999999982514 ) ;
#71481 = ORIENTED_EDGE ( 'NONE', *, *, #38964, .F. ) ;
#71480 = AXIS2_PLACEMENT_3D ( 'NONE', #13114, #113266, #43264 ) ;
#71483 = EDGE_LOOP ( 'NONE', ( #98367, #6575, #18282, #41112 ) ) ;
#71482 = CONICAL_SURFACE ( 'NONE', #84001, 0.1000000000000000472, 0.003490658503988666988 ) ;
#71484 = FACE_OUTER_BOUND ( 'NONE', #120646, .T. ) ;
#71485 = EDGE_LOOP ( 'NONE', ( #9012, #20244 ) ) ;
#71486 = CARTESIAN_POINT ( 'NONE',  ( 8.149999999999920419, 2.500000000000000000, -1.918653347947325782 ) ) ;
#71487 = CARTESIAN_POINT ( 'NONE',  ( 2.699999999999946443, 2.500000000000000000, -3.983716857408426293 ) ) ;
#71488 = CIRCLE ( 'NONE', #115289, 0.06509327318403745899 ) ;
#71489 = CARTESIAN_POINT ( 'NONE',  ( 12.04999999999990479, 2.500000000000000000, 2.165063509461097713 ) ) ;
#71492 = VERTEX_POINT ( 'NONE', #25239 ) ;
#71491 = ORIENTED_EDGE ( 'NONE', *, *, #55306, .F. ) ;
#71490 = AXIS2_PLACEMENT_3D ( 'NONE', #116671, #6685, #125842 ) ;
#71493 = FACE_BOUND ( 'NONE', #48390, .T. ) ;
#71494 = ORIENTED_EDGE ( 'NONE', *, *, #9637, .F. ) ;
#71495 = ADVANCED_FACE ( 'NONE', ( #65158 ), #39544, .T. ) ;
#71496 = CARTESIAN_POINT ( 'NONE',  ( -10.20000000000000639, 2.500000000000000000, -3.883716857408422207 ) ) ;
#71497 = CARTESIAN_POINT ( 'NONE',  ( 8.949999999999921130, 12.50000000000000000, -6.841600689897078702 ) ) ;
#71498 = CIRCLE ( 'NONE', #8691, 0.06509327318403741736 ) ;
#71499 = CARTESIAN_POINT ( 'NONE',  ( 9.549999999999915445, 2.500000000000000000, 6.395190528383296602 ) ) ;
#71500 = CARTESIAN_POINT ( 'NONE',  ( 11.84999999999990372, 2.500000000000000000, 1.818653347947321475 ) ) ;
#71501 = CARTESIAN_POINT ( 'NONE',  ( -11.64999999999999680, 2.500000000000000000, 2.757883832488649656 ) ) ;
#71502 = CARTESIAN_POINT ( 'NONE',  ( 6.849999999999929479, 12.50000000000000000, -2.576566944158915184 ) ) ;
#71503 = PLANE ( 'NONE',  #62078 ) ;
#71504 = DIRECTION ( 'NONE',  ( 0.000000000000000000, 0.000000000000000000, 1.000000000000000000 ) ) ;
#71505 = CARTESIAN_POINT ( 'NONE',  ( 7.699999999999922018, 2.500000000000000000, 0.4464101615137735513 ) ) ;
#71506 = DIRECTION ( 'NONE',  ( 0.000000000000000000, 0.000000000000000000, -1.000000000000000000 ) ) ;
#71507 = CARTESIAN_POINT ( 'NONE',  ( -2.300000000000033573, 2.500000000000000000, 0.4464101615137735513 ) ) ;
#71508 = ORIENTED_EDGE ( 'NONE', *, *, #17938, .F. ) ;
#71509 = ORIENTED_EDGE ( 'NONE', *, *, #7664, .T. ) ;
#71510 = EDGE_CURVE ( 'NONE', #13848, #50242, #29062, .T. ) ;
#71511 = EDGE_LOOP ( 'NONE', ( #113473, #4684 ) ) ;
#71512 = EDGE_LOOP ( 'NONE', ( #61908, #116179 ) ) ;
#71513 = DIRECTION ( 'NONE',  ( -0.000000000000000000, -1.000000000000000000, -0.000000000000000000 ) ) ;
#71514 = CARTESIAN_POINT ( 'NONE',  ( 4.599999999999940137, 2.500000000000000000, -4.330127018922201643 ) ) ;
#71516 = ORIENTED_EDGE ( 'NONE', *, *, #67874, .T. ) ;
#71515 = ORIENTED_EDGE ( 'NONE', *, *, #71257, .F. ) ;
#71517 = ORIENTED_EDGE ( 'NONE', *, *, #30639, .T. ) ;
#71518 = DIRECTION ( 'NONE',  ( 0.000000000000000000, 0.000000000000000000, 1.000000000000000000 ) ) ;
#71519 = AXIS2_PLACEMENT_3D ( 'NONE', #129410, #93966, #22661 ) ;
#71520 = CARTESIAN_POINT ( 'NONE',  ( 9.999999999999911182, 12.50000000000000000, -3.702399969078687292 ) ) ;
#71521 = DIRECTION ( 'NONE',  ( 0.000000000000000000, 1.000000000000000000, 0.000000000000000000 ) ) ;
#71522 = DIRECTION ( 'NONE',  ( 0.000000000000000000, 0.000000000000000000, 1.000000000000000000 ) ) ;
#71523 = PLANE ( 'NONE',  #114554 ) ;
#71524 = FACE_OUTER_BOUND ( 'NONE', #18806, .T. ) ;
#71525 = ADVANCED_FACE ( 'NONE', ( #97222 ), #31122, .T. ) ;
#71526 = ORIENTED_EDGE ( 'NONE', *, *, #45971, .F. ) ;
#71527 = AXIS2_PLACEMENT_3D ( 'NONE', #78391, #98638, #8975 ) ;
#71528 = CIRCLE ( 'NONE', #67378, 0.1000000000000002554 ) ;
#71529 = DIRECTION ( 'NONE',  ( -4.274815082592931898E-19, -0.9999939076577903929, -0.003490651415223739937 ) ) ;
#71530 = ORIENTED_EDGE ( 'NONE', *, *, #96140, .T. ) ;
#71531 = CONICAL_SURFACE ( 'NONE', #46386, 0.1000000000000002554, 0.003490658503988666988 ) ;
#71532 = EDGE_LOOP ( 'NONE', ( #49286, #10336, #44806, #6935 ) ) ;
#71533 = AXIS2_PLACEMENT_3D ( 'NONE', #86048, #66422, #27781 ) ;
#71534 = VERTEX_POINT ( 'NONE', #18007 ) ;
#71535 = PLANE ( 'NONE',  #63141 ) ;
#71536 = ORIENTED_EDGE ( 'NONE', *, *, #92749, .F. ) ;
#71537 = ORIENTED_EDGE ( 'NONE', *, *, #62027, .F. ) ;
#71538 = EDGE_LOOP ( 'NONE', ( #20822, #27688 ) ) ;
#71539 = AXIS2_PLACEMENT_3D ( 'NONE', #35401, #16998, #15737 ) ;
#71540 = DIRECTION ( 'NONE',  ( 0.000000000000000000, 0.000000000000000000, 1.000000000000000000 ) ) ;
#71541 = CIRCLE ( 'NONE', #75740, 0.06509327318403745899 ) ;
#71542 = FACE_OUTER_BOUND ( 'NONE', #96465, .T. ) ;
#71543 = DIRECTION ( 'NONE',  ( 0.000000000000000000, 0.000000000000000000, 1.000000000000000000 ) ) ;
#71544 = CIRCLE ( 'NONE', #42224, 0.1000000000000002554 ) ;
#71545 = CARTESIAN_POINT ( 'NONE',  ( 10.64999999999990976, 2.500000000000000000, 2.411473670974873862 ) ) ;
#71546 = CONICAL_SURFACE ( 'NONE', #73679, 0.1000000000000000472, 0.003490658503988666988 ) ;
#71547 = AXIS2_PLACEMENT_3D ( 'NONE', #66830, #106758, #17061 ) ;
#71548 = DIRECTION ( 'NONE',  ( 0.000000000000000000, 0.000000000000000000, 1.000000000000000000 ) ) ;
#71549 = CIRCLE ( 'NONE', #4621, 0.06509327318403745899 ) ;
#71550 = CARTESIAN_POINT ( 'NONE',  ( -6.850000000000017408, 2.500000000000000000, -6.148780366869526226 ) ) ;
#71551 = ORIENTED_EDGE ( 'NONE', *, *, #39014, .T. ) ;
#71552 = CARTESIAN_POINT ( 'NONE',  ( 12.04999999999990479, 2.500000000000000000, 2.165063509461097713 ) ) ;
#71553 = EDGE_CURVE ( 'NONE', #70779, #113276, #117468, .T. ) ;
#71554 = VERTEX_POINT ( 'NONE', #68397 ) ;
#71555 = AXIS2_PLACEMENT_3D ( 'NONE', #41249, #71990, #3246 ) ;
#71556 = DIRECTION ( 'NONE',  ( -0.000000000000000000, -1.000000000000000000, -0.000000000000000000 ) ) ;
#71557 = EDGE_LOOP ( 'NONE', ( #20861, #61326, #62764, #123887 ) ) ;
#71558 = CARTESIAN_POINT ( 'NONE',  ( 8.149999999999920419, 2.500000000000000000, -2.511473670974877948 ) ) ;
#71559 = ORIENTED_EDGE ( 'NONE', *, *, #68882, .T. ) ;
#71560 = EDGE_CURVE ( 'NONE', #83874, #91821, #112668, .T. ) ;
#71561 = CARTESIAN_POINT ( 'NONE',  ( -12.29999999999999538, 2.500000000000000000, -0.4464101615137742174 ) ) ;
#71562 = FACE_OUTER_BOUND ( 'NONE', #84379, .T. ) ;
#71563 = ORIENTED_EDGE ( 'NONE', *, *, #128595, .F. ) ;
#71564 = EDGE_CURVE ( 'NONE', #125928, #60150, #86751, .T. ) ;
#71566 = VERTEX_POINT ( 'NONE', #69039 ) ;
#71565 = EDGE_CURVE ( 'NONE', #35564, #78919, #43637, .T. ) ;
#71567 = CARTESIAN_POINT ( 'NONE',  ( 11.24999999999990763, 12.50000000000000000, 1.472243186433545459 ) ) ;
#71568 = DIRECTION ( 'NONE',  ( 0.000000000000000000, 0.000000000000000000, 1.000000000000000000 ) ) ;
#71569 = EDGE_CURVE ( 'NONE', #37534, #114066, #96557, .T. ) ;
#71570 = CARTESIAN_POINT ( 'NONE',  ( 183.9218750003414016, 0.000000000000000000, 7.564683531250000925 ) ) ;
#71571 = ADVANCED_FACE ( 'NONE', ( #126688 ), #3900, .T. ) ;
#71572 = CARTESIAN_POINT ( 'NONE',  ( 11.44999999999990514, 12.50000000000000000, -6.083687093685488989 ) ) ;
#71573 = CARTESIAN_POINT ( 'NONE',  ( 10.64999999999991331, 12.50000000000000000, 6.148780366869520897 ) ) ;
#71574 = EDGE_LOOP ( 'NONE', ( #76569, #99794, #27760, #30270 ) ) ;
#71575 = CARTESIAN_POINT ( 'NONE',  ( 2.500000000000002220, -1.761799387799148686, 10.00000000000000000 ) ) ;
#71576 = VECTOR ( 'NONE', #97232, 1000.000000000000000 ) ;
#71577 = AXIS2_PLACEMENT_3D ( 'NONE', #118837, #27632, #106223 ) ;
#71578 = CIRCLE ( 'NONE', #73712, 0.06509327318403745899 ) ;
#71579 = EDGE_CURVE ( 'NONE', #62336, #119953, #20647, .T. ) ;
#71580 = EDGE_LOOP ( 'NONE', ( #26446, #101810, #68782, #45470 ) ) ;
#71581 = ADVANCED_FACE ( 'NONE', ( #27827 ), #66465, .T. ) ;
#71582 = CARTESIAN_POINT ( 'NONE',  ( 13.74999999999989519, 12.50000000000000000, -2.792790559304616504 ) ) ;
#71583 = LINE ( 'NONE', #99125, #22891 ) ;
#71585 = ADVANCED_FACE ( 'NONE', ( #38312 ), #54084, .T. ) ;
#71584 = CIRCLE ( 'NONE', #6798, 0.06509327318403745899 ) ;
#71586 = CIRCLE ( 'NONE', #38138, 7.699999999999999289 ) ;
#71587 = AXIS2_PLACEMENT_3D ( 'NONE', #38724, #128387, #118529 ) ;
#71588 = CIRCLE ( 'NONE', #86236, 0.1000000000000002554 ) ;
#71589 = AXIS2_PLACEMENT_3D ( 'NONE', #9071, #88930, #128882 ) ;
#71590 = CARTESIAN_POINT ( 'NONE',  ( 187.0052083336747444, -6.551208109652278289, 3.782341765624995134 ) ) ;
#71591 = CARTESIAN_POINT ( 'NONE',  ( 2.099999999999949463, 12.50000000000000000, 0.6277270498435120194 ) ) ;
#71592 = PLANE ( 'NONE',  #17291 ) ;
#71593 = DIRECTION ( 'NONE',  ( 0.000000000000000000, 0.000000000000000000, -1.000000000000000000 ) ) ;
#71594 = FACE_OUTER_BOUND ( 'NONE', #5440, .T. ) ;
#71595 = ORIENTED_EDGE ( 'NONE', *, *, #3748, .F. ) ;
#71596 = CIRCLE ( 'NONE', #36008, 0.1000000000000000472 ) ;
#71597 = DIRECTION ( 'NONE',  ( 0.000000000000000000, 0.000000000000000000, 1.000000000000000000 ) ) ;
#71598 = DIRECTION ( 'NONE',  ( 0.000000000000000000, 1.000000000000000000, 0.000000000000000000 ) ) ;
#71599 = DIRECTION ( 'NONE',  ( 0.000000000000000000, 1.000000000000000000, 0.000000000000000000 ) ) ;
#71600 = VERTEX_POINT ( 'NONE', #106392 ) ;
#71601 = CARTESIAN_POINT ( 'NONE',  ( -12.89999999999999147, 2.500000000000000000, 4.430127018922196847 ) ) ;
#71602 = VERTEX_POINT ( 'NONE', #56628 ) ;
#71603 = VERTEX_POINT ( 'NONE', #28490 ) ;
#71604 = CARTESIAN_POINT ( 'NONE',  ( -1.900000000000034106, 2.500000000000000000, -3.983716857408426293 ) ) ;
#71605 = ORIENTED_EDGE ( 'NONE', *, *, #117361, .T. ) ;
#71606 = CARTESIAN_POINT ( 'NONE',  ( 19.61395058415432402, -2.556813634647812084, -4.305699210822446332 ) ) ;
#71607 = CARTESIAN_POINT ( 'NONE',  ( -0.4000000000000396572, 12.50000000000000000, 4.395220292106234439 ) ) ;
#71608 = CARTESIAN_POINT ( 'NONE',  ( 16.79927703354126933, 2.472530191752442263, 3.248144252800958309 ) ) ;
#71609 = VECTOR ( 'NONE', #19926, 1000.000000000000000 ) ;
#71610 = ORIENTED_EDGE ( 'NONE', *, *, #45144, .T. ) ;
#71611 = AXIS2_PLACEMENT_3D ( 'NONE', #45907, #106739, #75346 ) ;
#71612 = DIRECTION ( 'NONE',  ( 0.000000000000000000, 1.000000000000000000, 0.000000000000000000 ) ) ;
#71613 = CARTESIAN_POINT ( 'NONE',  ( -13.34999999999999076, 2.500000000000000000, 2.165063509461101265 ) ) ;
#71614 = EDGE_CURVE ( 'NONE', #48774, #4494, #7539, .T. ) ;
#71615 = VECTOR ( 'NONE', #118783, 1000.000000000000000 ) ;
#71616 = ORIENTED_EDGE ( 'NONE', *, *, #65797, .F. ) ;
#71617 = CIRCLE ( 'NONE', #59016, 0.06509327318403745899 ) ;
#71618 = EDGE_CURVE ( 'NONE', #102929, #2990, #104262, .T. ) ;
#71619 = CIRCLE ( 'NONE', #121787, 0.1000000000000002554 ) ;
#71620 = AXIS2_PLACEMENT_3D ( 'NONE', #127926, #108282, #6198 ) ;
#71621 = ORIENTED_EDGE ( 'NONE', *, *, #60526, .T. ) ;
#71622 = ADVANCED_FACE ( 'NONE', ( #47481 ), #70801, .T. ) ;
#71623 = EDGE_LOOP ( 'NONE', ( #32291, #24159 ) ) ;
#71624 = DIRECTION ( 'NONE',  ( 0.000000000000000000, -0.000000000000000000, 1.000000000000000000 ) ) ;
#71625 = PLANE ( 'NONE',  #47931 ) ;
#71626 = DIRECTION ( 'NONE',  ( 0.000000000000000000, 1.000000000000000000, 0.000000000000000000 ) ) ;
#71627 = FACE_BOUND ( 'NONE', #120733, .T. ) ;
#71628 = VERTEX_POINT ( 'NONE', #116204 ) ;
#71629 = DIRECTION ( 'NONE',  ( -0.000000000000000000, 1.000000000000000000, -0.000000000000000000 ) ) ;
#71630 = FACE_OUTER_BOUND ( 'NONE', #50005, .T. ) ;
#71631 = CONICAL_SURFACE ( 'NONE', #98815, 0.1000000000000002554, 0.003490658503988666988 ) ;
#71632 = ORIENTED_EDGE ( 'NONE', *, *, #127579, .T. ) ;
#71633 = EDGE_CURVE ( 'NONE', #55439, #128871, #127256, .T. ) ;
#71634 = CONICAL_SURFACE ( 'NONE', #25450, 0.1000000000000002554, 0.003490658503988666988 ) ;
#71635 = DIRECTION ( 'NONE',  ( 0.000000000000000000, 0.000000000000000000, 1.000000000000000000 ) ) ;
#71636 = LINE ( 'NONE', #122669, #97229 ) ;
#71637 = AXIS2_PLACEMENT_3D ( 'NONE', #102131, #101491, #104061 ) ;
#71638 = CIRCLE ( 'NONE', #88339, 0.09999999999999982514 ) ;
#71639 = CIRCLE ( 'NONE', #113409, 0.1000000000000002554 ) ;
#71640 = DIRECTION ( 'NONE',  ( 0.000000000000000000, 0.000000000000000000, 1.000000000000000000 ) ) ;
#71641 = CARTESIAN_POINT ( 'NONE',  ( 2.500000000000002220, 1.499999999999999334, 10.00000000000000178 ) ) ;
#71642 = DIRECTION ( 'NONE',  ( 0.000000000000000000, 1.000000000000000000, 0.000000000000000000 ) ) ;
#71643 = DIRECTION ( 'NONE',  ( 0.000000000000000000, -0.000000000000000000, 1.000000000000000000 ) ) ;
#71644 = CIRCLE ( 'NONE', #529, 0.06509327318403745899 ) ;
#71645 = DIRECTION ( 'NONE',  ( 0.000000000000000000, -0.9999939076577903929, 0.003490651415223739937 ) ) ;
#71646 = VERTEX_POINT ( 'NONE', #87387 ) ;
#71647 = CONICAL_SURFACE ( 'NONE', #67513, 0.1000000000000002554, 0.003490658503988666988 ) ;
#71648 = ORIENTED_EDGE ( 'NONE', *, *, #6500, .F. ) ;
#71649 = ORIENTED_EDGE ( 'NONE', *, *, #58402, .T. ) ;
#71650 = EDGE_LOOP ( 'NONE', ( #44173, #38478, #86503, #66937 ) ) ;
#71651 = CARTESIAN_POINT ( 'NONE',  ( 4.999999999999936939, 12.50000000000000000, -3.637306695894650055 ) ) ;
#71652 = FACE_OUTER_BOUND ( 'NONE', #76742, .T. ) ;
#71653 = EDGE_LOOP ( 'NONE', ( #78629, #33809 ) ) ;
#71654 = FACE_BOUND ( 'NONE', #109393, .T. ) ;
#71655 = EDGE_CURVE ( 'NONE', #51914, #56997, #88016, .T. ) ;
#71656 = CARTESIAN_POINT ( 'NONE',  ( -13.34999999999999076, 2.500000000000000000, 1.572243186433549544 ) ) ;
#71657 = CARTESIAN_POINT ( 'NONE',  ( -9.800000000000006040, 2.500000000000000000, 4.676537180435972552 ) ) ;
#71658 = DIRECTION ( 'NONE',  ( 0.000000000000000000, 1.000000000000000000, 0.000000000000000000 ) ) ;
#71659 = CARTESIAN_POINT ( 'NONE',  ( 9.599999999999917932, 2.500000000000000000, 0.6928203230275494784 ) ) ;
#71660 = CARTESIAN_POINT ( 'NONE',  ( -10.65000000000000213, 2.500000000000000000, 1.718653347947321386 ) ) ;
#71661 = FACE_OUTER_BOUND ( 'NONE', #113439, .T. ) ;
#71662 = DIRECTION ( 'NONE',  ( 0.000000000000000000, 1.000000000000000000, 0.000000000000000000 ) ) ;
#71663 = DIRECTION ( 'NONE',  ( 0.000000000000000000, 1.000000000000000000, 0.000000000000000000 ) ) ;
#71664 = DIRECTION ( 'NONE',  ( 0.000000000000000000, 1.000000000000000000, 0.000000000000000000 ) ) ;
#71665 = ORIENTED_EDGE ( 'NONE', *, *, #70432, .T. ) ;
#71666 = EDGE_LOOP ( 'NONE', ( #109929, #106188, #24460, #111725 ) ) ;
#71667 = VERTEX_POINT ( 'NONE', #1585 ) ;
#71668 = ORIENTED_EDGE ( 'NONE', *, *, #58465, .F. ) ;
#71669 = EDGE_CURVE ( 'NONE', #62648, #125139, #112199, .T. ) ;
#71670 = ORIENTED_EDGE ( 'NONE', *, *, #99922, .T. ) ;
#71671 = VECTOR ( 'NONE', #37680, 1000.000000000000000 ) ;
#71672 = ORIENTED_EDGE ( 'NONE', *, *, #41872, .T. ) ;
#71673 = CONICAL_SURFACE ( 'NONE', #15210, 0.1000000000000000472, 0.003490658503988666988 ) ;
#71674 = DIRECTION ( 'NONE',  ( 0.000000000000000000, 0.000000000000000000, 1.000000000000000000 ) ) ;
#71675 = EDGE_LOOP ( 'NONE', ( #77608, #102048 ) ) ;
#71676 = ORIENTED_EDGE ( 'NONE', *, *, #95623, .T. ) ;
#71677 = CIRCLE ( 'NONE', #126040, 0.06509327318403745899 ) ;
#71678 = CONICAL_SURFACE ( 'NONE', #38243, 0.1000000000000002554, 0.003490658503988666988 ) ;
#71679 = AXIS2_PLACEMENT_3D ( 'NONE', #48085, #8136, #97814 ) ;
#71680 = DIRECTION ( 'NONE',  ( -0.000000000000000000, 1.000000000000000000, -0.000000000000000000 ) ) ;
#71681 = CARTESIAN_POINT ( 'NONE',  ( 15.83209681635537258, -2.499999999999999556, 5.404881881984330505 ) ) ;
#71682 = DIRECTION ( 'NONE',  ( 0.000000000000000000, -0.000000000000000000, 1.000000000000000000 ) ) ;
#71683 = FACE_OUTER_BOUND ( 'NONE', #49361, .T. ) ;
#71684 = AXIS2_PLACEMENT_3D ( 'NONE', #96146, #36612, #95509 ) ;
#71685 = AXIS2_PLACEMENT_3D ( 'NONE', #100452, #9498, #30448 ) ;
#71686 = EDGE_CURVE ( 'NONE', #56285, #84308, #121074, .T. ) ;
#71687 = EDGE_LOOP ( 'NONE', ( #30483, #43408, #87997, #43760 ) ) ;
#71688 = DIRECTION ( 'NONE',  ( -0.000000000000000000, 1.000000000000000000, -0.000000000000000000 ) ) ;
#71689 = AXIS2_PLACEMENT_3D ( 'NONE', #67858, #107790, #18110 ) ;
#71690 = ORIENTED_EDGE ( 'NONE', *, *, #64374, .F. ) ;
#71691 = ORIENTED_EDGE ( 'NONE', *, *, #78684, .F. ) ;
#71692 = CARTESIAN_POINT ( 'NONE',  ( -5.000000000000022204, 2.500000000000000000, -0.5928203230275541635 ) ) ;
#71693 = CARTESIAN_POINT ( 'NONE',  ( -10.00000000000000533, 2.500000000000000000, 0.5928203230275495006 ) ) ;
#71695 = EDGE_CURVE ( 'NONE', #80059, #69479, #122064, .T. ) ;
#71694 = DIRECTION ( 'NONE',  ( 0.000000000000000000, 0.000000000000000000, 1.000000000000000000 ) ) ;
#71696 = ORIENTED_EDGE ( 'NONE', *, *, #33764, .T. ) ;
#71697 = ORIENTED_EDGE ( 'NONE', *, *, #107753, .F. ) ;
#71698 = AXIS2_PLACEMENT_3D ( 'NONE', #79509, #121349, #70328 ) ;
#71699 = FACE_OUTER_BOUND ( 'NONE', #72763, .T. ) ;
#71700 = DIRECTION ( 'NONE',  ( -0.000000000000000000, 1.000000000000000000, -0.000000000000000000 ) ) ;
#71701 = DIRECTION ( 'NONE',  ( -0.000000000000000000, 1.000000000000000000, -0.000000000000000000 ) ) ;
#71702 = DIRECTION ( 'NONE',  ( 0.000000000000000000, 0.000000000000000000, -1.000000000000000000 ) ) ;
#71703 = ORIENTED_EDGE ( 'NONE', *, *, #19648, .F. ) ;
#71704 = CARTESIAN_POINT ( 'NONE',  ( 13.74999999999989519, 2.500000000000000000, -2.757883832488654097 ) ) ;
#71706 = ORIENTED_EDGE ( 'NONE', *, *, #88419, .T. ) ;
#71705 = AXIS2_PLACEMENT_3D ( 'NONE', #12653, #113448, #92515 ) ;
#71707 = CARTESIAN_POINT ( 'NONE',  ( -3.950000000000028155, 12.50000000000000000, -6.776507416713039689 ) ) ;
#71708 = CIRCLE ( 'NONE', #98893, 0.06509327318403745899 ) ;
#71709 = ORIENTED_EDGE ( 'NONE', *, *, #31836, .F. ) ;
#71710 = FACE_OUTER_BOUND ( 'NONE', #1628, .T. ) ;
#71711 = ADVANCED_FACE ( 'NONE', ( #89968 ), #71625, .T. ) ;
#71712 = CARTESIAN_POINT ( 'NONE',  ( 14.14999999999989200, 12.50000000000000000, -2.099970236277064473 ) ) ;
#71713 = DIRECTION ( 'NONE',  ( 0.000000000000000000, 1.000000000000000000, 0.000000000000000000 ) ) ;
#71714 = CARTESIAN_POINT ( 'NONE',  ( 3.149999999999946176, 2.500000000000000000, -6.841600689897077814 ) ) ;
#71716 = CIRCLE ( 'NONE', #63303, 0.06509327318403745899 ) ;
#71715 = DIRECTION ( 'NONE',  ( 0.000000000000000000, 0.000000000000000000, 1.000000000000000000 ) ) ;
#71717 = ORIENTED_EDGE ( 'NONE', *, *, #53579, .T. ) ;
#71718 = AXIS2_PLACEMENT_3D ( 'NONE', #58210, #59511, #98106 ) ;
#71720 = EDGE_CURVE ( 'NONE', #127250, #71628, #35399, .T. ) ;
#71719 = CIRCLE ( 'NONE', #115618, 0.1000000000000002554 ) ;
#71721 = DIRECTION ( 'NONE',  ( -4.274815082592931898E-19, -0.9999939076577903929, -0.003490651415223739937 ) ) ;
#71722 = CIRCLE ( 'NONE', #59223, 0.06509327318403745899 ) ;
#71723 = DIRECTION ( 'NONE',  ( 0.000000000000000000, -0.000000000000000000, 1.000000000000000000 ) ) ;
#71724 = VERTEX_POINT ( 'NONE', #121361 ) ;
#71725 = VERTEX_POINT ( 'NONE', #110894 ) ;
#71726 = ADVANCED_FACE ( 'NONE', ( #69692 ), #21901, .T. ) ;
#71728 = EDGE_LOOP ( 'NONE', ( #100071, #6152, #15492, #93256 ) ) ;
#71727 = EDGE_CURVE ( 'NONE', #32033, #51297, #77161, .T. ) ;
#71729 = DIRECTION ( 'NONE',  ( 0.000000000000000000, 0.000000000000000000, 1.000000000000000000 ) ) ;
#71730 = DIRECTION ( 'NONE',  ( -0.000000000000000000, -1.000000000000000000, -0.000000000000000000 ) ) ;
#71731 = ADVANCED_FACE ( 'NONE', ( #52000 ), #101086, .T. ) ;
#71732 = CARTESIAN_POINT ( 'NONE',  ( 187.1927083336747160, 6.551208109652275624, -3.782341765624998686 ) ) ;
#71733 = EDGE_CURVE ( 'NONE', #117143, #4956, #64635, .T. ) ;
#71734 = VECTOR ( 'NONE', #93520, 1000.000000000000000 ) ;
#71735 = DIRECTION ( 'NONE',  ( 0.000000000000000000, 1.000000000000000000, 0.000000000000000000 ) ) ;
#71736 = DIRECTION ( 'NONE',  ( 0.000000000000000000, -0.000000000000000000, 1.000000000000000000 ) ) ;
#71737 = CARTESIAN_POINT ( 'NONE',  ( -5.850000000000018296, 2.500000000000000000, 2.757883832488649656 ) ) ;
#71738 = AXIS2_PLACEMENT_3D ( 'NONE', #117721, #20193, #40502 ) ;
#71739 = DIRECTION ( 'NONE',  ( 0.000000000000000000, 1.000000000000000000, 0.000000000000000000 ) ) ;
#71740 = CIRCLE ( 'NONE', #128084, 0.1000000000000002554 ) ;
#71741 = AXIS2_PLACEMENT_3D ( 'NONE', #92118, #43064, #50279 ) ;
#71742 = FACE_OUTER_BOUND ( 'NONE', #40093, .T. ) ;
#71743 = EDGE_CURVE ( 'NONE', #54236, #109083, #18664, .T. ) ;
#71744 = EDGE_CURVE ( 'NONE', #92818, #16529, #39622, .T. ) ;
#71745 = AXIS2_PLACEMENT_3D ( 'NONE', #122206, #93384, #102546 ) ;
#71746 = EDGE_CURVE ( 'NONE', #39809, #19040, #98082, .T. ) ;
#71747 = ADVANCED_FACE ( 'NONE', ( #51366 ), #85565, .T. ) ;
#71748 = ADVANCED_FACE ( 'NONE', ( #120094 ), #30440, .T. ) ;
#71749 = AXIS2_PLACEMENT_3D ( 'NONE', #65205, #105140, #34501 ) ;
#71750 = VERTEX_POINT ( 'NONE', #20600 ) ;
#71751 = CARTESIAN_POINT ( 'NONE',  ( 8.549999999999924327, 2.500000000000000000, 1.718653347947321386 ) ) ;
#71752 = DIRECTION ( 'NONE',  ( -0.000000000000000000, -1.000000000000000000, -0.000000000000000000 ) ) ;
#71753 = DIRECTION ( 'NONE',  ( 0.000000000000000000, 0.000000000000000000, 1.000000000000000000 ) ) ;
#71754 = FACE_OUTER_BOUND ( 'NONE', #43905, .T. ) ;
#71755 = ADVANCED_FACE ( 'NONE', ( #10742 ), #60547, .T. ) ;
#71756 = VERTEX_POINT ( 'NONE', #2893 ) ;
#71757 = CARTESIAN_POINT ( 'NONE',  ( 10.39999999999991154, 2.500000000000000000, -3.737306695894649700 ) ) ;
#71758 = DIRECTION ( 'NONE',  ( 0.000000000000000000, 0.000000000000000000, 1.000000000000000000 ) ) ;
#71760 = EDGE_LOOP ( 'NONE', ( #43750, #62226, #9566, #23550 ) ) ;
#71759 = CARTESIAN_POINT ( 'NONE',  ( 3.099999999999944134, 2.500000000000000000, 4.676537180435972552 ) ) ;
#71761 = VECTOR ( 'NONE', #23519, 1000.000000000000000 ) ;
#71762 = ORIENTED_EDGE ( 'NONE', *, *, #8946, .F. ) ;
#71763 = CARTESIAN_POINT ( 'NONE',  ( 14.59999999999989484, 2.500000000000000000, 0.6928203230275494784 ) ) ;
#71764 = CIRCLE ( 'NONE', #11102, 0.1000000000000002554 ) ;
#71765 = ORIENTED_EDGE ( 'NONE', *, *, #43687, .T. ) ;
#71766 = CIRCLE ( 'NONE', #50836, 0.06509327318403745899 ) ;
#71767 = ORIENTED_EDGE ( 'NONE', *, *, #48069, .F. ) ;
#71768 = CARTESIAN_POINT ( 'NONE',  ( -1.650000000000035216, 2.500000000000000000, -1.372243186433550033 ) ) ;
#71769 = AXIS2_PLACEMENT_3D ( 'NONE', #82964, #31298, #100644 ) ;
#71770 = AXIS2_PLACEMENT_3D ( 'NONE', #64472, #124040, #15356 ) ;
#71771 = LINE ( 'NONE', #41040, #101143 ) ;
#71772 = CARTESIAN_POINT ( 'NONE',  ( -2.100000000000033396, 12.50000000000000000, -0.7579135962115917113 ) ) ;
#71773 = CARTESIAN_POINT ( 'NONE',  ( -1.650000000000034772, 12.50000000000000000, 5.867463478539781896 ) ) ;
#71775 = ORIENTED_EDGE ( 'NONE', *, *, #27677, .F. ) ;
#71774 = AXIS2_PLACEMENT_3D ( 'NONE', #3968, #116497, #66109 ) ;
#71776 = CIRCLE ( 'NONE', #21594, 0.1000000000000002554 ) ;
#71777 = AXIS2_PLACEMENT_3D ( 'NONE', #123311, #3540, #103686 ) ;
#71778 = DIRECTION ( 'NONE',  ( -0.000000000000000000, -1.000000000000000000, -0.000000000000000000 ) ) ;
#71780 = EDGE_LOOP ( 'NONE', ( #41086, #81023, #94730, #101382 ) ) ;
#71779 = AXIS2_PLACEMENT_3D ( 'NONE', #106460, #114343, #75699 ) ;
#71781 = AXIS2_PLACEMENT_3D ( 'NONE', #78658, #46598, #17775 ) ;
#71782 = CARTESIAN_POINT ( 'NONE',  ( -4.350000000000023626, 2.500000000000000000, 2.511473670974873507 ) ) ;
#71783 = CARTESIAN_POINT ( 'NONE',  ( 7.899999999999924860, 12.50000000000000000, 4.330127018922196314 ) ) ;
#71784 = AXIS2_PLACEMENT_3D ( 'NONE', #121157, #129072, #21017 ) ;
#71785 = ORIENTED_EDGE ( 'NONE', *, *, #44284, .F. ) ;
#71786 = EDGE_CURVE ( 'NONE', #31778, #50468, #91836, .T. ) ;
#71787 = EDGE_LOOP ( 'NONE', ( #48437, #63092 ) ) ;
#71789 = ORIENTED_EDGE ( 'NONE', *, *, #86531, .T. ) ;
#71788 = ADVANCED_FACE ( 'NONE', ( #122660 ), #103012, .T. ) ;
#71790 = ORIENTED_EDGE ( 'NONE', *, *, #58101, .T. ) ;
#71791 = DIRECTION ( 'NONE',  ( 0.000000000000000000, 0.000000000000000000, -1.000000000000000000 ) ) ;
#71792 = FACE_OUTER_BOUND ( 'NONE', #34496, .T. ) ;
#71793 = PLANE ( 'NONE',  #54628 ) ;
#71794 = FACE_BOUND ( 'NONE', #119716, .T. ) ;
#71795 = ORIENTED_EDGE ( 'NONE', *, *, #4311, .T. ) ;
#71796 = LINE ( 'NONE', #5444, #80876 ) ;
#71797 = CARTESIAN_POINT ( 'NONE',  ( 185.3645833340161175, -6.668395609140180369, 3.849999999999994760 ) ) ;
#71798 = DIRECTION ( 'NONE',  ( 0.000000000000000000, 0.000000000000000000, 1.000000000000000000 ) ) ;
#71799 = CARTESIAN_POINT ( 'NONE',  ( 7.949999999999925571, 2.500000000000000000, -6.395190528383301931 ) ) ;
#71800 = AXIS2_PLACEMENT_3D ( 'NONE', #57120, #28318, #126519 ) ;
#71801 = ADVANCED_FACE ( 'NONE', ( #42847 ), #25100, .T. ) ;
#71802 = LINE ( 'NONE', #60699, #111259 ) ;
#71803 = DIRECTION ( 'NONE',  ( 0.000000000000000000, 0.000000000000000000, 1.000000000000000000 ) ) ;
#71804 = LINE ( 'NONE', #103188, #49209 ) ;
#71805 = CONICAL_SURFACE ( 'NONE', #94783, 0.09999999999999982514, 0.003490658503988666988 ) ;
#71806 = AXIS2_PLACEMENT_3D ( 'NONE', #23970, #26546, #4951 ) ;
#71807 = DIRECTION ( 'NONE',  ( -0.000000000000000000, -1.000000000000000000, -0.000000000000000000 ) ) ;
#71808 = ORIENTED_EDGE ( 'NONE', *, *, #28275, .T. ) ;
#71809 = VERTEX_POINT ( 'NONE', #74210 ) ;
#71810 = VERTEX_POINT ( 'NONE', #43473 ) ;
#71811 = EDGE_LOOP ( 'NONE', ( #102106, #126898, #68910, #45099 ) ) ;
#71812 = VERTEX_POINT ( 'NONE', #114130 ) ;
#71813 = CARTESIAN_POINT ( 'NONE',  ( 3.949999999999941558, 2.500000000000000000, -1.718653347947326049 ) ) ;
#71814 = CARTESIAN_POINT ( 'NONE',  ( -3.750000000000027534, 2.500000000000000000, 2.857883832488649301 ) ) ;
#71815 = ORIENTED_EDGE ( 'NONE', *, *, #49541, .T. ) ;
#71816 = FACE_BOUND ( 'NONE', #25798, .T. ) ;
#71817 = VECTOR ( 'NONE', #11077, 1000.000000000000000 ) ;
#71818 = AXIS2_PLACEMENT_3D ( 'NONE', #66551, #75101, #106490 ) ;
#71819 = FACE_OUTER_BOUND ( 'NONE', #117384, .T. ) ;
#71820 = AXIS2_PLACEMENT_3D ( 'NONE', #35155, #75061, #16109 ) ;
#71821 = AXIS2_PLACEMENT_3D ( 'NONE', #94281, #52430, #81257 ) ;
#71822 = ORIENTED_EDGE ( 'NONE', *, *, #27956, .T. ) ;
#71823 = CARTESIAN_POINT ( 'NONE',  ( 129.5000000000000000, 1.375000000000002665, -7.634788798650556707 ) ) ;
#71824 = CARTESIAN_POINT ( 'NONE',  ( 2.899999999999946620, 2.500000000000000000, -5.122947341949753763 ) ) ;
#71825 = CARTESIAN_POINT ( 'NONE',  ( 9.349999999999916156, 12.50000000000000000, 6.841600689897072485 ) ) ;
#71826 = DIRECTION ( 'NONE',  ( 0.000000000000000000, 1.000000000000000000, 0.000000000000000000 ) ) ;
#71827 = CONICAL_SURFACE ( 'NONE', #15363, 0.1000000000000002554, 0.003490658503988666988 ) ;
#71828 = ORIENTED_EDGE ( 'NONE', *, *, #38032, .T. ) ;
#71829 = CARTESIAN_POINT ( 'NONE',  ( -5.850000000000022737, 12.50000000000000000, -2.165063509461101710 ) ) ;
#71830 = EDGE_CURVE ( 'NONE', #97166, #84391, #29150, .T. ) ;
#71831 = ORIENTED_EDGE ( 'NONE', *, *, #30894, .F. ) ;
#71832 = AXIS2_PLACEMENT_3D ( 'NONE', #28503, #109640, #11428 ) ;
#71833 = VECTOR ( 'NONE', #48717, 1000.000000000000000 ) ;
#71834 = ORIENTED_EDGE ( 'NONE', *, *, #126281, .T. ) ;
#71835 = ORIENTED_EDGE ( 'NONE', *, *, #119046, .T. ) ;
#71836 = CARTESIAN_POINT ( 'NONE',  ( -5.600000000000023626, 2.500000000000000000, -4.083716857408426826 ) ) ;
#71837 = DIRECTION ( 'NONE',  ( 0.000000000000000000, 1.000000000000000000, 0.000000000000000000 ) ) ;
#71838 = CONICAL_SURFACE ( 'NONE', #99018, 0.1000000000000002554, 0.003490658503988666988 ) ;
#71839 = ORIENTED_EDGE ( 'NONE', *, *, #128749, .T. ) ;
#71840 = CARTESIAN_POINT ( 'NONE',  ( 0.1999999999999562961, 2.500000000000000000, 4.676537180435972552 ) ) ;
#71841 = VECTOR ( 'NONE', #32387, 1000.000000000000000 ) ;
#71842 = DIRECTION ( 'NONE',  ( 0.000000000000000000, 1.000000000000000000, 0.000000000000000000 ) ) ;
#71843 = DIRECTION ( 'NONE',  ( -0.000000000000000000, 1.000000000000000000, -0.000000000000000000 ) ) ;
#71844 = DIRECTION ( 'NONE',  ( -0.000000000000000000, -1.000000000000000000, -0.000000000000000000 ) ) ;
#71845 = CARTESIAN_POINT ( 'NONE',  ( 187.0312500006828031, 9.429780353434619030E-16, -7.700000000000000178 ) ) ;
#71846 = VERTEX_POINT ( 'NONE', #94475 ) ;
#71847 = EDGE_CURVE ( 'NONE', #93896, #78285, #3983, .T. ) ;
#71848 = DIRECTION ( 'NONE',  ( 0.000000000000000000, 1.000000000000000000, 0.000000000000000000 ) ) ;
#71849 = EDGE_CURVE ( 'NONE', #39661, #74932, #5451, .T. ) ;
#71850 = ORIENTED_EDGE ( 'NONE', *, *, #109904, .T. ) ;
#71851 = DIRECTION ( 'NONE',  ( 0.000000000000000000, 1.000000000000000000, -1.224646799147353207E-16 ) ) ;
#71852 = VERTEX_POINT ( 'NONE', #53924 ) ;
#71853 = DIRECTION ( 'NONE',  ( -0.000000000000000000, 1.000000000000000000, -0.000000000000000000 ) ) ;
#71854 = ORIENTED_EDGE ( 'NONE', *, *, #61346, .F. ) ;
#71855 = CARTESIAN_POINT ( 'NONE',  ( -6.050000000000022027, 2.500000000000000000, -6.148780366869526226 ) ) ;
#71856 = DIRECTION ( 'NONE',  ( 0.000000000000000000, 1.000000000000000000, 0.000000000000000000 ) ) ;
#71857 = CARTESIAN_POINT ( 'NONE',  ( -7.100000000000018296, 12.50000000000000000, -2.385244779468109755E-15 ) ) ;
#71858 = AXIS2_PLACEMENT_3D ( 'NONE', #91619, #13037, #22261 ) ;
#71860 = EDGE_CURVE ( 'NONE', #120640, #125450, #110602, .T. ) ;
#71859 = DIRECTION ( 'NONE',  ( 0.000000000000000000, -0.000000000000000000, 1.000000000000000000 ) ) ;
#71861 = FACE_OUTER_BOUND ( 'NONE', #26858, .T. ) ;
#71862 = ORIENTED_EDGE ( 'NONE', *, *, #81342, .F. ) ;
#71863 = EDGE_LOOP ( 'NONE', ( #47127, #22449, #65717, #71515 ) ) ;
#71864 = CARTESIAN_POINT ( 'NONE',  ( -8.100000000000013856, 2.500000000000000000, 0.3464101615137736845 ) ) ;
#71865 = AXIS2_PLACEMENT_3D ( 'NONE', #12034, #91250, #91896 ) ;
#71866 = CONICAL_SURFACE ( 'NONE', #103149, 0.09999999999999982514, 0.003490658503988666988 ) ;
#71867 = AXIS2_PLACEMENT_3D ( 'NONE', #121544, #1138, #60081 ) ;
#71868 = DIRECTION ( 'NONE',  ( 0.000000000000000000, -0.9999939076577903929, 0.003490651415223739937 ) ) ;
#71869 = CIRCLE ( 'NONE', #46729, 0.06509327318403745899 ) ;
#71871 = CARTESIAN_POINT ( 'NONE',  ( 0.5999999999999621192, 12.50000000000000000, 0.3464101615137758494 ) ) ;
#71870 = VECTOR ( 'NONE', #3472, 1000.000000000000000 ) ;
#71873 = ORIENTED_EDGE ( 'NONE', *, *, #52156, .F. ) ;
#71872 = EDGE_LOOP ( 'NONE', ( #55777, #60570 ) ) ;
#71874 = EDGE_LOOP ( 'NONE', ( #2610, #23224 ) ) ;
#71875 = CARTESIAN_POINT ( 'NONE',  ( -4.600000000000024514, 12.50000000000000000, -0.6928203230275542523 ) ) ;
#71876 = ORIENTED_EDGE ( 'NONE', *, *, #103124, .F. ) ;
#71877 = CARTESIAN_POINT ( 'NONE',  ( 8.749999999999920064, 2.500000000000000000, -2.857883832488653741 ) ) ;
#71878 = PLANE ( 'NONE',  #116670 ) ;
#71879 = CIRCLE ( 'NONE', #103266, 0.06509327318403745899 ) ;
#71880 = CONICAL_SURFACE ( 'NONE', #76075, 0.1000000000000000472, 0.003490658503988666988 ) ;
#71881 = FACE_OUTER_BOUND ( 'NONE', #23347, .T. ) ;
#71882 = CARTESIAN_POINT ( 'NONE',  ( -6.050000000000022027, 2.500000000000000000, -1.818653347947326138 ) ) ;
#71883 = LINE ( 'NONE', #50956, #59132 ) ;
#71884 = DIRECTION ( 'NONE',  ( 0.000000000000000000, 1.000000000000000000, 0.000000000000000000 ) ) ;
#71885 = CARTESIAN_POINT ( 'NONE',  ( 9.599999999999917932, 12.50000000000000000, 0.7579135962115869374 ) ) ;
#71886 = VECTOR ( 'NONE', #30849, 1000.000000000000000 ) ;
#71887 = DIRECTION ( 'NONE',  ( 0.000000000000000000, 0.000000000000000000, 1.000000000000000000 ) ) ;
#71888 = VERTEX_POINT ( 'NONE', #33012 ) ;
#71889 = EDGE_CURVE ( 'NONE', #34976, #4024, #15914, .T. ) ;
#71890 = CARTESIAN_POINT ( 'NONE',  ( -9.350000000000006750, 2.500000000000000000, 1.818653347947321475 ) ) ;
#71891 = CARTESIAN_POINT ( 'NONE',  ( 59.88087687668669901, -3.776023963385989557, 4.996435080087643144 ) ) ;
#71892 = ORIENTED_EDGE ( 'NONE', *, *, #25025, .T. ) ;
#71893 = ORIENTED_EDGE ( 'NONE', *, *, #43491, .T. ) ;
#71894 = ADVANCED_FACE ( 'NONE', ( #4152 ), #22886, .T. ) ;
#71895 = CARTESIAN_POINT ( 'NONE',  ( 184.3177083336747160, 4.367472073101515306, 7.564683531250000925 ) ) ;
#71896 = PLANE ( 'NONE',  #76162 ) ;
#71897 = CARTESIAN_POINT ( 'NONE',  ( 7.099999999999925926, 2.500000000000000000, 0.7928203230275495672 ) ) ;
#71898 = EDGE_CURVE ( 'NONE', #62131, #25372, #65005, .T. ) ;
#71899 = CIRCLE ( 'NONE', #50973, 0.06509327318403745899 ) ;
#71900 = DIRECTION ( 'NONE',  ( -0.000000000000000000, -1.000000000000000000, -0.000000000000000000 ) ) ;
#71901 = CARTESIAN_POINT ( 'NONE',  ( -6.250000000000015987, 2.500000000000000000, 1.372243186433545370 ) ) ;
#71902 = CARTESIAN_POINT ( 'NONE',  ( 15.19999999999989271, 2.500000000000000000, -0.2464101615137783419 ) ) ;
#71903 = DIRECTION ( 'NONE',  ( 0.000000000000000000, 0.000000000000000000, 1.000000000000000000 ) ) ;
#71904 = FACE_OUTER_BOUND ( 'NONE', #123428, .T. ) ;
#71905 = EDGE_CURVE ( 'NONE', #123378, #26594, #93894, .T. ) ;
#71906 = EDGE_CURVE ( 'NONE', #41184, #34349, #70909, .T. ) ;
#71907 = EDGE_CURVE ( 'NONE', #109647, #30034, #25744, .T. ) ;
#71908 = CIRCLE ( 'NONE', #17489, 0.09999999999999982514 ) ;
#71910 = AXIS2_PLACEMENT_3D ( 'NONE', #120587, #62324, #110754 ) ;
#71909 = CARTESIAN_POINT ( 'NONE',  ( 8.949999999999921130, 12.50000000000000000, 1.818653347947321475 ) ) ;
#71911 = ORIENTED_EDGE ( 'NONE', *, *, #46574, .F. ) ;
#71912 = CONICAL_SURFACE ( 'NONE', #111604, 0.09999999999999999167, 0.003490658503988666988 ) ;
#71913 = VERTEX_POINT ( 'NONE', #84014 ) ;
#71914 = EDGE_CURVE ( 'NONE', #66570, #120306, #63094, .T. ) ;
#71915 = ORIENTED_EDGE ( 'NONE', *, *, #41419, .F. ) ;
#71916 = ORIENTED_EDGE ( 'NONE', *, *, #28106, .T. ) ;
#71917 = VECTOR ( 'NONE', #116859, 1000.000000000000000 ) ;
#71918 = DIRECTION ( 'NONE',  ( 0.000000000000000000, 1.000000000000000000, 0.000000000000000000 ) ) ;
#71919 = DIRECTION ( 'NONE',  ( -0.000000000000000000, -1.000000000000000000, -0.000000000000000000 ) ) ;
#71920 = ADVANCED_FACE ( 'NONE', ( #33643 ), #23823, .T. ) ;
#71921 = VECTOR ( 'NONE', #14033, 1000.000000000000000 ) ;
#71922 = ORIENTED_EDGE ( 'NONE', *, *, #45751, .T. ) ;
#71923 = CARTESIAN_POINT ( 'NONE',  ( 14.14999999999989555, 12.50000000000000000, 2.165063509461097713 ) ) ;
#71924 = AXIS2_PLACEMENT_3D ( 'NONE', #92036, #120219, #110386 ) ;
#71925 = CARTESIAN_POINT ( 'NONE',  ( 5.849999999999932143, 2.500000000000000000, 1.472243186433545459 ) ) ;
#71927 = EDGE_LOOP ( 'NONE', ( #5365, #108833 ) ) ;
#71926 = DIRECTION ( 'NONE',  ( 0.000000000000000000, 1.000000000000000000, 0.000000000000000000 ) ) ;
#71928 = LINE ( 'NONE', #111845, #47452 ) ;
#71929 = DIRECTION ( 'NONE',  ( -0.000000000000000000, 1.000000000000000000, -0.000000000000000000 ) ) ;
#71930 = ORIENTED_EDGE ( 'NONE', *, *, #121424, .F. ) ;
#71931 = CONICAL_SURFACE ( 'NONE', #84437, 0.1000000000000002554, 0.003490658503988666988 ) ;
#71932 = AXIS2_PLACEMENT_3D ( 'NONE', #107526, #17849, #28329 ) ;
#71933 = ORIENTED_EDGE ( 'NONE', *, *, #6090, .F. ) ;
#71934 = EDGE_LOOP ( 'NONE', ( #5507, #67775, #94574, #60460 ) ) ;
#71935 = ORIENTED_EDGE ( 'NONE', *, *, #97659, .F. ) ;
#71936 = DIRECTION ( 'NONE',  ( -0.000000000000000000, 1.000000000000000000, -0.000000000000000000 ) ) ;
#71937 = CONICAL_SURFACE ( 'NONE', #113693, 0.09999999999999982514, 0.003490658503988666988 ) ;
#71938 = CARTESIAN_POINT ( 'NONE',  ( -8.950000000000009948, 2.500000000000000000, -6.741600689897071952 ) ) ;
#71939 = CARTESIAN_POINT ( 'NONE',  ( 2.500000000000002220, -1.500000000000000000, -9.999999999999998224 ) ) ;
#71940 = AXIS2_PLACEMENT_3D ( 'NONE', #28659, #118311, #118955 ) ;
#71941 = EDGE_LOOP ( 'NONE', ( #54098, #5929 ) ) ;
#71942 = CARTESIAN_POINT ( 'NONE',  ( 12.89999999999990266, 2.500000000000000000, -3.737306695894649700 ) ) ;
#71943 = ORIENTED_EDGE ( 'NONE', *, *, #104727, .T. ) ;
#71944 = DIRECTION ( 'NONE',  ( -0.000000000000000000, 1.000000000000000000, -0.000000000000000000 ) ) ;
#71945 = DIRECTION ( 'NONE',  ( 0.000000000000000000, 1.000000000000000000, 0.000000000000000000 ) ) ;
#71946 = DIRECTION ( 'NONE',  ( 0.000000000000000000, -0.9999939076577903929, 0.003490651415223739937 ) ) ;
#71947 = FACE_OUTER_BOUND ( 'NONE', #98240, .T. ) ;
#71948 = ORIENTED_EDGE ( 'NONE', *, *, #45210, .T. ) ;
#71949 = EDGE_CURVE ( 'NONE', #18148, #29100, #45867, .T. ) ;
#71950 = VERTEX_POINT ( 'NONE', #26410 ) ;
#71951 = VERTEX_POINT ( 'NONE', #46047 ) ;
#71952 = LINE ( 'NONE', #128463, #20999 ) ;
#71954 = CIRCLE ( 'NONE', #61586, 0.06509327318403741736 ) ;
#71953 = DIRECTION ( 'NONE',  ( 0.000000000000000000, 0.000000000000000000, 1.000000000000000000 ) ) ;
#71955 = AXIS2_PLACEMENT_3D ( 'NONE', #7090, #57506, #28694 ) ;
#71956 = CARTESIAN_POINT ( 'NONE',  ( -0.8500000000000382805, 2.500000000000000000, -1.572243186433550211 ) ) ;
#71957 = FACE_BOUND ( 'NONE', #45231, .T. ) ;
#71958 = CARTESIAN_POINT ( 'NONE',  ( -0.6000000000000323963, 2.500000000000000000, 0.3464101615137759604 ) ) ;
#71959 = CARTESIAN_POINT ( 'NONE',  ( -10.84999999999999964, 12.50000000000000000, 1.472243186433545459 ) ) ;
#71960 = CARTESIAN_POINT ( 'NONE',  ( -15.79999999999998117, 2.500000000000000000, 0.000000000000000000 ) ) ;
#71961 = ADVANCED_FACE ( 'NONE', ( #7382 ), #19125, .T. ) ;
#71962 = AXIS2_PLACEMENT_3D ( 'NONE', #48597, #95762, #27636 ) ;
#71963 = AXIS2_PLACEMENT_3D ( 'NONE', #68503, #8926, #85571 ) ;
#71964 = CIRCLE ( 'NONE', #13349, 0.09999999999999982514 ) ;
#71965 = AXIS2_PLACEMENT_3D ( 'NONE', #58659, #8889, #18069 ) ;
#71966 = DIRECTION ( 'NONE',  ( 0.000000000000000000, 1.000000000000000000, 0.000000000000000000 ) ) ;
#71967 = CARTESIAN_POINT ( 'NONE',  ( 108.0000000000000142, 8.500000000000000000, 0.000000000000000000 ) ) ;
#71968 = DIRECTION ( 'NONE',  ( 0.000000000000000000, 0.000000000000000000, -1.000000000000000000 ) ) ;
#71969 = ORIENTED_EDGE ( 'NONE', *, *, #35434, .F. ) ;
#71971 = DIRECTION ( 'NONE',  ( -0.000000000000000000, -1.000000000000000000, -0.000000000000000000 ) ) ;
#71970 = CIRCLE ( 'NONE', #115861, 0.06509327318403745899 ) ;
#71972 = CIRCLE ( 'NONE', #103360, 2.000000000000000000 ) ;
#71973 = FACE_OUTER_BOUND ( 'NONE', #111948, .T. ) ;
#71974 = ORIENTED_EDGE ( 'NONE', *, *, #87411, .T. ) ;
#71975 = ORIENTED_EDGE ( 'NONE', *, *, #8617, .F. ) ;
#71976 = CIRCLE ( 'NONE', #32283, 0.09999999999999982514 ) ;
#71977 = PLANE ( 'NONE',  #31403 ) ;
#71978 = FACE_OUTER_BOUND ( 'NONE', #20775, .T. ) ;
#71979 = FACE_BOUND ( 'NONE', #12983, .T. ) ;
#71980 = LINE ( 'NONE', #81770, #38940 ) ;
#71981 = EDGE_LOOP ( 'NONE', ( #72004, #45292, #114030, #3271 ) ) ;
#71982 = CARTESIAN_POINT ( 'NONE',  ( 12.09999999999990550, 12.50000000000000000, -3.637306695894650055 ) ) ;
#71983 = DIRECTION ( 'NONE',  ( 0.000000000000000000, 0.000000000000000000, 1.000000000000000000 ) ) ;
#71985 = ORIENTED_EDGE ( 'NONE', *, *, #89935, .F. ) ;
#71984 = CIRCLE ( 'NONE', #15524, 0.09999999999999982514 ) ;
#71986 = FACE_OUTER_BOUND ( 'NONE', #98202, .T. ) ;
#71987 = PLANE ( 'NONE',  #72101 ) ;
#71988 = EDGE_CURVE ( 'NONE', #111575, #117378, #33271, .T. ) ;
#71989 = ORIENTED_EDGE ( 'NONE', *, *, #128331, .F. ) ;
#71990 = DIRECTION ( 'NONE',  ( -0.000000000000000000, 1.000000000000000000, -0.000000000000000000 ) ) ;
#71991 = CARTESIAN_POINT ( 'NONE',  ( -3.950000000000026379, 2.500000000000000000, 6.941600689897073018 ) ) ;
#71992 = CIRCLE ( 'NONE', #120016, 0.1000000000000002554 ) ;
#71993 = EDGE_CURVE ( 'NONE', #95287, #70361, #127812, .T. ) ;
#71994 = AXIS2_PLACEMENT_3D ( 'NONE', #92898, #73885, #4468 ) ;
#71995 = ORIENTED_EDGE ( 'NONE', *, *, #105840, .T. ) ;
#71996 = CARTESIAN_POINT ( 'NONE',  ( -3.950000000000026379, 12.50000000000000000, -1.818653347947326138 ) ) ;
#71997 = CARTESIAN_POINT ( 'NONE',  ( -8.150000000000012790, 2.500000000000000000, -2.411473670974877859 ) ) ;
#71998 = DIRECTION ( 'NONE',  ( 0.000000000000000000, 0.000000000000000000, -1.000000000000000000 ) ) ;
#71999 = EDGE_LOOP ( 'NONE', ( #39208, #28220 ) ) ;
#72000 = ADVANCED_FACE ( 'NONE', ( #47983 ), #57798, .T. ) ;
#72001 = VERTEX_POINT ( 'NONE', #6089 ) ;
#72002 = EDGE_CURVE ( 'NONE', #17444, #120069, #123132, .T. ) ;
#72003 = DIRECTION ( 'NONE',  ( 0.000000000000000000, 0.000000000000000000, -1.000000000000000000 ) ) ;
#72004 = ORIENTED_EDGE ( 'NONE', *, *, #45111, .F. ) ;
#72005 = FACE_OUTER_BOUND ( 'NONE', #5748, .T. ) ;
#72006 = CARTESIAN_POINT ( 'NONE',  ( -8.950000000000009948, 12.50000000000000000, -1.818653347947326138 ) ) ;
#72007 = VECTOR ( 'NONE', #46158, 1000.000000000000000 ) ;
#72008 = LINE ( 'NONE', #61545, #80134 ) ;
#72009 = EDGE_LOOP ( 'NONE', ( #52369, #14817 ) ) ;
#72010 = ADVANCED_FACE ( 'NONE', ( #108165 ), #43738, .T. ) ;
#72011 = CARTESIAN_POINT ( 'NONE',  ( -13.09999999999999254, 2.500000000000000000, -4.676537180435975216 ) ) ;
#72012 = FACE_OUTER_BOUND ( 'NONE', #82381, .T. ) ;
#72013 = CARTESIAN_POINT ( 'NONE',  ( 8.349999999999919709, 12.50000000000000000, -2.857883832488653741 ) ) ;
#72014 = DIRECTION ( 'NONE',  ( -0.000000000000000000, -1.000000000000000000, -0.000000000000000000 ) ) ;
#72015 = FACE_OUTER_BOUND ( 'NONE', #91205, .T. ) ;
#72016 = EDGE_CURVE ( 'NONE', #109879, #113918, #100153, .T. ) ;
#72017 = DIRECTION ( 'NONE',  ( 0.000000000000000000, 0.000000000000000000, 1.000000000000000000 ) ) ;
#72018 = VERTEX_POINT ( 'NONE', #8659 ) ;
#72019 = ORIENTED_EDGE ( 'NONE', *, *, #91207, .F. ) ;
#72020 = CARTESIAN_POINT ( 'NONE',  ( 11.64999999999990443, 2.500000000000000000, 1.572243186433545548 ) ) ;
#72022 = EDGE_LOOP ( 'NONE', ( #88007, #66116 ) ) ;
#72021 = CIRCLE ( 'NONE', #88730, 0.06509327318403745899 ) ;
#72023 = CIRCLE ( 'NONE', #3062, 0.1000000000000002554 ) ;
#72024 = CARTESIAN_POINT ( 'NONE',  ( 103.1711462153774903, 7.589803906595561145, 1.339608020536842581 ) ) ;
#72026 = VERTEX_POINT ( 'NONE', #48617 ) ;
#72025 = VERTEX_POINT ( 'NONE', #86591 ) ;
#72027 = VERTEX_POINT ( 'NONE', #107535 ) ;
#72028 = CIRCLE ( 'NONE', #42801, 0.06509327318403745899 ) ;
#72029 = CARTESIAN_POINT ( 'NONE',  ( 2.049999999999948308, 2.500000000000000000, 6.495190528383297135 ) ) ;
#72030 = AXIS2_PLACEMENT_3D ( 'NONE', #49436, #108328, #89345 ) ;
#72031 = CARTESIAN_POINT ( 'NONE',  ( 1.899999999999949507, 2.500000000000000000, 4.776537180435972196 ) ) ;
#72032 = DIRECTION ( 'NONE',  ( 0.000000000000000000, -0.000000000000000000, 1.000000000000000000 ) ) ;
#72033 = FACE_OUTER_BOUND ( 'NONE', #116882, .T. ) ;
#72034 = LINE ( 'NONE', #9881, #85635 ) ;
#72035 = CARTESIAN_POINT ( 'NONE',  ( -1.250000000000001554, 2.500000000000000000, 2.065063509461097624 ) ) ;
#72036 = DIRECTION ( 'NONE',  ( 0.000000000000000000, 1.000000000000000000, 0.000000000000000000 ) ) ;
#72037 = DIRECTION ( 'NONE',  ( -0.000000000000000000, 1.000000000000000000, -0.000000000000000000 ) ) ;
#72038 = FACE_OUTER_BOUND ( 'NONE', #5766, .T. ) ;
#72039 = EDGE_LOOP ( 'NONE', ( #57208, #306 ) ) ;
#72040 = EDGE_CURVE ( 'NONE', #11303, #125704, #37468, .T. ) ;
#72041 = AXIS2_PLACEMENT_3D ( 'NONE', #76707, #57050, #26329 ) ;
#72042 = AXIS2_PLACEMENT_3D ( 'NONE', #38425, #78345, #18756 ) ;
#72043 = DIRECTION ( 'NONE',  ( 0.000000000000000000, -0.000000000000000000, 1.000000000000000000 ) ) ;
#72044 = AXIS2_PLACEMENT_3D ( 'NONE', #46233, #58005, #127384 ) ;
#72045 = ORIENTED_EDGE ( 'NONE', *, *, #64059, .F. ) ;
#72046 = ORIENTED_EDGE ( 'NONE', *, *, #10720, .F. ) ;
#72047 = DIRECTION ( 'NONE',  ( 0.000000000000000000, 0.000000000000000000, 1.000000000000000000 ) ) ;
#72048 = DIRECTION ( 'NONE',  ( 0.000000000000000000, 1.000000000000000000, 0.000000000000000000 ) ) ;
#72049 = PLANE ( 'NONE',  #34026 ) ;
#72050 = EDGE_CURVE ( 'NONE', #74488, #73563, #87612, .T. ) ;
#72051 = AXIS2_PLACEMENT_3D ( 'NONE', #120327, #39855, #30676 ) ;
#72052 = DIRECTION ( 'NONE',  ( 0.000000000000000000, -0.000000000000000000, 1.000000000000000000 ) ) ;
#72053 = CIRCLE ( 'NONE', #72343, 0.1000000000000002554 ) ;
#72055 = DIRECTION ( 'NONE',  ( 0.000000000000000000, 1.000000000000000000, 0.000000000000000000 ) ) ;
#72054 = CIRCLE ( 'NONE', #124278, 0.1000000000000000056 ) ;
#72056 = CARTESIAN_POINT ( 'NONE',  ( 4.599999999999939249, 2.500000000000000000, -3.637306695894650055 ) ) ;
#72057 = DIRECTION ( 'NONE',  ( -0.000000000000000000, -1.000000000000000000, -0.000000000000000000 ) ) ;
#72058 = ORIENTED_EDGE ( 'NONE', *, *, #121799, .F. ) ;
#72059 = EDGE_CURVE ( 'NONE', #109722, #73210, #48021, .T. ) ;
#72060 = AXIS2_PLACEMENT_3D ( 'NONE', #58239, #86383, #118424 ) ;
#72061 = EDGE_CURVE ( 'NONE', #29100, #73228, #28986, .T. ) ;
#72062 = EDGE_CURVE ( 'NONE', #77164, #122473, #114888, .T. ) ;
#72064 = ORIENTED_EDGE ( 'NONE', *, *, #40132, .T. ) ;
#72063 = CIRCLE ( 'NONE', #113916, 0.1000000000000000472 ) ;
#72065 = CIRCLE ( 'NONE', #53284, 0.06509327318403745899 ) ;
#72066 = VERTEX_POINT ( 'NONE', #66312 ) ;
#72067 = ADVANCED_FACE ( 'NONE', ( #106245 ), #127437, .T. ) ;
#72068 = EDGE_LOOP ( 'NONE', ( #38131, #99986 ) ) ;
#72069 = VECTOR ( 'NONE', #38431, 1000.000000000000000 ) ;
#72070 = ORIENTED_EDGE ( 'NONE', *, *, #9898, .F. ) ;
#72071 = DIRECTION ( 'NONE',  ( 0.000000000000000000, 0.000000000000000000, 1.000000000000000000 ) ) ;
#72072 = DIRECTION ( 'NONE',  ( 0.000000000000000000, 1.000000000000000000, 0.000000000000000000 ) ) ;
#72073 = EDGE_CURVE ( 'NONE', #54151, #19741, #70993, .T. ) ;
#72074 = EDGE_CURVE ( 'NONE', #57754, #12097, #121165, .T. ) ;
#72075 = CARTESIAN_POINT ( 'NONE',  ( -5.650000000000023448, 2.500000000000000000, -1.818653347947326138 ) ) ;
#72076 = DIRECTION ( 'NONE',  ( 0.000000000000000000, 0.000000000000000000, 1.000000000000000000 ) ) ;
#72077 = FACE_OUTER_BOUND ( 'NONE', #81688, .T. ) ;
#72078 = VERTEX_POINT ( 'NONE', #17183 ) ;
#72079 = CARTESIAN_POINT ( 'NONE',  ( 4.799999999999935874, 2.500000000000000000, 0.3464101615137735735 ) ) ;
#72080 = FACE_OUTER_BOUND ( 'NONE', #8858, .T. ) ;
#72081 = CARTESIAN_POINT ( 'NONE',  ( -6.900000000000015454, 12.50000000000000000, 4.676537180435972552 ) ) ;
#72082 = CARTESIAN_POINT ( 'NONE',  ( 0.4499999999999569344, 12.50000000000000000, -2.165063509461101710 ) ) ;
#72083 = VECTOR ( 'NONE', #94413, 1000.000000000000000 ) ;
#72084 = DIRECTION ( 'NONE',  ( 0.000000000000000000, 0.000000000000000000, 1.000000000000000000 ) ) ;
#72085 = ORIENTED_EDGE ( 'NONE', *, *, #27937, .T. ) ;
#72086 = ORIENTED_EDGE ( 'NONE', *, *, #80627, .F. ) ;
#72087 = ORIENTED_EDGE ( 'NONE', *, *, #20456, .F. ) ;
#72088 = CARTESIAN_POINT ( 'NONE',  ( 6.449999999999931788, 2.500000000000000000, -2.511473670974877948 ) ) ;
#72089 = VERTEX_POINT ( 'NONE', #57141 ) ;
#72090 = CONICAL_SURFACE ( 'NONE', #69932, 0.09999999999999999167, 0.003490658503988666988 ) ;
#72091 = DIRECTION ( 'NONE',  ( 0.000000000000000000, 0.000000000000000000, 1.000000000000000000 ) ) ;
#72092 = DIRECTION ( 'NONE',  ( -0.000000000000000000, -1.000000000000000000, -0.000000000000000000 ) ) ;
#72093 = AXIS2_PLACEMENT_3D ( 'NONE', #89504, #68566, #119596 ) ;
#72094 = ORIENTED_EDGE ( 'NONE', *, *, #101275, .F. ) ;
#72095 = CARTESIAN_POINT ( 'NONE',  ( 7.299999999999926104, 2.500000000000000000, -0.2464101615137782308 ) ) ;
#72096 = DIRECTION ( 'NONE',  ( 0.000000000000000000, 0.000000000000000000, -1.000000000000000000 ) ) ;
#72097 = DIRECTION ( 'NONE',  ( -0.000000000000000000, -1.000000000000000000, -0.000000000000000000 ) ) ;
#72098 = DIRECTION ( 'NONE',  ( -4.274815082592931898E-19, -0.9999939076577903929, -0.003490651415223739937 ) ) ;
#72099 = CONICAL_SURFACE ( 'NONE', #57427, 0.1000000000000002554, 0.003490658503988666988 ) ;
#72100 = DIRECTION ( 'NONE',  ( 0.000000000000000000, 0.000000000000000000, 1.000000000000000000 ) ) ;
#72101 = AXIS2_PLACEMENT_3D ( 'NONE', #2562, #90304, #80521 ) ;
#72102 = ORIENTED_EDGE ( 'NONE', *, *, #110520, .F. ) ;
#72103 = VERTEX_POINT ( 'NONE', #97066 ) ;
#72104 = CARTESIAN_POINT ( 'NONE',  ( 187.2500000000000000, 9.429780353434619030E-16, -7.700000000000000178 ) ) ;
#72105 = DIRECTION ( 'NONE',  ( 0.000000000000000000, 0.000000000000000000, -1.000000000000000000 ) ) ;
#72106 = DIRECTION ( 'NONE',  ( -0.000000000000000000, 1.000000000000000000, -0.000000000000000000 ) ) ;
#72107 = FACE_OUTER_BOUND ( 'NONE', #37668, .T. ) ;
#72108 = ADVANCED_FACE ( 'NONE', ( #127191 ), #32219, .T. ) ;
#72109 = ORIENTED_EDGE ( 'NONE', *, *, #47643, .F. ) ;
#72110 = AXIS2_PLACEMENT_3D ( 'NONE', #101772, #12090, #91948 ) ;
#72111 = EDGE_LOOP ( 'NONE', ( #17237, #3447, #59749, #97898 ) ) ;
#72112 = DIRECTION ( 'NONE',  ( 0.000000000000000000, 1.000000000000000000, 0.000000000000000000 ) ) ;
#72113 = CARTESIAN_POINT ( 'NONE',  ( 13.09999999999989839, 2.500000000000000000, -0.2464101615137783419 ) ) ;
#72114 = DIRECTION ( 'NONE',  ( 0.000000000000000000, 0.000000000000000000, 1.000000000000000000 ) ) ;
#72115 = AXIS2_PLACEMENT_3D ( 'NONE', #12689, #2229, #80166 ) ;
#72116 = DIRECTION ( 'NONE',  ( -0.000000000000000000, 1.000000000000000000, -0.000000000000000000 ) ) ;
#72117 = ORIENTED_EDGE ( 'NONE', *, *, #17098, .T. ) ;
#72118 = DIRECTION ( 'NONE',  ( -0.000000000000000000, 1.000000000000000000, -0.000000000000000000 ) ) ;
#72119 = FACE_OUTER_BOUND ( 'NONE', #77092, .T. ) ;
#72120 = ORIENTED_EDGE ( 'NONE', *, *, #97039, .T. ) ;
#72121 = CARTESIAN_POINT ( 'NONE',  ( -8.150000000000014566, 2.500000000000000000, -6.741600689897072840 ) ) ;
#72122 = ORIENTED_EDGE ( 'NONE', *, *, #34704, .F. ) ;
#72123 = DIRECTION ( 'NONE',  ( 0.000000000000000000, 0.000000000000000000, 1.000000000000000000 ) ) ;
#72124 = AXIS2_PLACEMENT_3D ( 'NONE', #85715, #96178, #68016 ) ;
#72125 = ORIENTED_EDGE ( 'NONE', *, *, #56952, .T. ) ;
#72126 = CARTESIAN_POINT ( 'NONE',  ( 11.64999999999990621, 2.500000000000000000, 6.395190528383296602 ) ) ;
#72127 = PLANE ( 'NONE',  #8285 ) ;
#72128 = CIRCLE ( 'NONE', #30376, 0.06509327318403745899 ) ;
#72129 = CIRCLE ( 'NONE', #17827, 0.06509327318403745899 ) ;
#72130 = ORIENTED_EDGE ( 'NONE', *, *, #98488, .T. ) ;
#72131 = ORIENTED_EDGE ( 'NONE', *, *, #73614, .F. ) ;
#72132 = DIRECTION ( 'NONE',  ( 0.000000000000000000, 0.000000000000000000, 1.000000000000000000 ) ) ;
#72133 = DIRECTION ( 'NONE',  ( 0.000000000000000000, 0.000000000000000000, -1.000000000000000000 ) ) ;
#72134 = CARTESIAN_POINT ( 'NONE',  ( -6.517459502904499961E-15, 2.500000000000000000, 4.230127018922196669 ) ) ;
#72135 = CARTESIAN_POINT ( 'NONE',  ( 185.1510416670080872, 4.367472073101518859, -7.564683531249999149 ) ) ;
#72136 = VECTOR ( 'NONE', #61541, 1000.000000000000000 ) ;
#72137 = CIRCLE ( 'NONE', #30294, 0.1000000000000002554 ) ;
#72138 = DIRECTION ( 'NONE',  ( 0.000000000000000000, 0.000000000000000000, -1.000000000000000000 ) ) ;
#72139 = DIRECTION ( 'NONE',  ( -4.274815082592931898E-19, -0.9999939076577903929, -0.003490651415223739937 ) ) ;
#72140 = LINE ( 'NONE', #32873, #117836 ) ;
#72141 = CIRCLE ( 'NONE', #28228, 0.1000000000000000472 ) ;
#72142 = FACE_OUTER_BOUND ( 'NONE', #59979, .T. ) ;
#72143 = DIRECTION ( 'NONE',  ( 0.000000000000000000, 0.000000000000000000, -1.000000000000000000 ) ) ;
#72144 = AXIS2_PLACEMENT_3D ( 'NONE', #63353, #63995, #125487 ) ;
#72146 = ADVANCED_FACE ( 'NONE', ( #2074 ), #72127, .T. ) ;
#72145 = AXIS2_PLACEMENT_3D ( 'NONE', #91947, #71658, #54577 ) ;
#72147 = ORIENTED_EDGE ( 'NONE', *, *, #71253, .F. ) ;
#72148 = ORIENTED_EDGE ( 'NONE', *, *, #20040, .F. ) ;
#72149 = CARTESIAN_POINT ( 'NONE',  ( 4.999999999999973355, 12.50000000000000000, -4.395220292106239768 ) ) ;
#72150 = VERTEX_POINT ( 'NONE', #89183 ) ;
#72151 = LINE ( 'NONE', #32241, #32920 ) ;
#72152 = CARTESIAN_POINT ( 'NONE',  ( -8.350000000000012079, 2.500000000000000000, -1.472243186433550122 ) ) ;
#72153 = VECTOR ( 'NONE', #92020, 1000.000000000000000 ) ;
#72154 = CARTESIAN_POINT ( 'NONE',  ( -10.84999999999999964, 2.500000000000000000, 1.572243186433545548 ) ) ;
#72156 = EDGE_LOOP ( 'NONE', ( #86825, #79952 ) ) ;
#72155 = ORIENTED_EDGE ( 'NONE', *, *, #31543, .T. ) ;
#72157 = EDGE_CURVE ( 'NONE', #119700, #95333, #100248, .T. ) ;
#72158 = FACE_BOUND ( 'NONE', #5268, .T. ) ;
#72159 = EDGE_LOOP ( 'NONE', ( #80347, #2898, #78983, #37976 ) ) ;
#72160 = ADVANCED_FACE ( 'NONE', ( #110744 ), #83522, .T. ) ;
#72161 = DIRECTION ( 'NONE',  ( 0.000000000000000000, 1.000000000000000000, 0.000000000000000000 ) ) ;
#72162 = CARTESIAN_POINT ( 'NONE',  ( -1.650000000000034772, 12.50000000000000000, 5.802370205355744659 ) ) ;
#72163 = PLANE ( 'NONE',  #103633 ) ;
#72164 = DIRECTION ( 'NONE',  ( 0.000000000000000000, -0.9999939076577903929, 0.003490651415223739937 ) ) ;
#72165 = DIRECTION ( 'NONE',  ( -4.274815082592931898E-19, -0.9999939076577903929, -0.003490651415223739937 ) ) ;
#72166 = CARTESIAN_POINT ( 'NONE',  ( -7.499999999999980460, 12.50000000000000000, -4.330127018922201643 ) ) ;
#72167 = ADVANCED_FACE ( 'NONE', ( #30922 ), #18755, .T. ) ;
#72168 = DIRECTION ( 'NONE',  ( 0.000000000000000000, 0.000000000000000000, -1.000000000000000000 ) ) ;
#72169 = EDGE_CURVE ( 'NONE', #19824, #32526, #119109, .T. ) ;
#72170 = CARTESIAN_POINT ( 'NONE',  ( -8.300000000000011369, 2.500000000000000000, -0.1000000000000022815 ) ) ;
#72171 = CARTESIAN_POINT ( 'NONE',  ( -14.14999999999998792, 12.50000000000000000, 2.857883832488652853 ) ) ;
#72172 = FACE_OUTER_BOUND ( 'NONE', #74766, .T. ) ;
#72173 = ADVANCED_FACE ( 'NONE', ( #21077 ), #81462, .T. ) ;
#72174 = VECTOR ( 'NONE', #34156, 1000.000000000000000 ) ;
#72175 = CARTESIAN_POINT ( 'NONE',  ( -5.650000000000023448, 12.50000000000000000, -1.753560074763288679 ) ) ;
#72176 = ORIENTED_EDGE ( 'NONE', *, *, #88422, .T. ) ;
#72177 = VERTEX_POINT ( 'NONE', #70190 ) ;
#72178 = EDGE_LOOP ( 'NONE', ( #25651, #67101 ) ) ;
#72179 = DIRECTION ( 'NONE',  ( 0.000000000000000000, 0.000000000000000000, -1.000000000000000000 ) ) ;
#72180 = VERTEX_POINT ( 'NONE', #61002 ) ;
#72181 = FACE_OUTER_BOUND ( 'NONE', #117950, .T. ) ;
#72182 = DIRECTION ( 'NONE',  ( 0.000000000000000000, 0.000000000000000000, 1.000000000000000000 ) ) ;
#72184 = VERTEX_POINT ( 'NONE', #42015 ) ;
#72183 = ORIENTED_EDGE ( 'NONE', *, *, #69497, .T. ) ;
#72185 = AXIS2_PLACEMENT_3D ( 'NONE', #66181, #104805, #76006 ) ;
#72186 = ORIENTED_EDGE ( 'NONE', *, *, #129551, .F. ) ;
#72187 = DIRECTION ( 'NONE',  ( -0.000000000000000000, -1.000000000000000000, -0.000000000000000000 ) ) ;
#72188 = AXIS2_PLACEMENT_3D ( 'NONE', #33678, #73582, #14014 ) ;
#72189 = CONICAL_SURFACE ( 'NONE', #22110, 0.1000000000000002554, 0.003490658503988666988 ) ;
#72190 = DIRECTION ( 'NONE',  ( 0.000000000000000000, 1.000000000000000000, 0.000000000000000000 ) ) ;
#72191 = FACE_OUTER_BOUND ( 'NONE', #82380, .T. ) ;
#72192 = CARTESIAN_POINT ( 'NONE',  ( 9.599999999999917932, 2.500000000000000000, -0.5928203230275541635 ) ) ;
#72193 = CARTESIAN_POINT ( 'NONE',  ( -12.69999999999999218, 12.50000000000000000, -4.676537180435975216 ) ) ;
#72194 = DIRECTION ( 'NONE',  ( 0.000000000000000000, 1.000000000000000000, 0.000000000000000000 ) ) ;
#72195 = ORIENTED_EDGE ( 'NONE', *, *, #81032, .F. ) ;
#72196 = CARTESIAN_POINT ( 'NONE',  ( 6.249999999999932498, 2.500000000000000000, 5.802370205355744659 ) ) ;
#72197 = ORIENTED_EDGE ( 'NONE', *, *, #101860, .F. ) ;
#72198 = AXIS2_PLACEMENT_3D ( 'NONE', #9955, #91089, #100270 ) ;
#72199 = VERTEX_POINT ( 'NONE', #119276 ) ;
#72200 = ORIENTED_EDGE ( 'NONE', *, *, #96025, .F. ) ;
#72201 = AXIS2_PLACEMENT_3D ( 'NONE', #74398, #43671, #54739 ) ;
#72202 = LINE ( 'NONE', #112121, #12948 ) ;
#72203 = VERTEX_POINT ( 'NONE', #90450 ) ;
#72204 = ORIENTED_EDGE ( 'NONE', *, *, #110458, .T. ) ;
#72205 = ORIENTED_EDGE ( 'NONE', *, *, #55096, .F. ) ;
#72206 = DIRECTION ( 'NONE',  ( -0.000000000000000000, 1.000000000000000000, -0.000000000000000000 ) ) ;
#72208 = CONICAL_SURFACE ( 'NONE', #47071, 0.1000000000000002554, 0.003490658503988666988 ) ;
#72207 = DIRECTION ( 'NONE',  ( -0.000000000000000000, 1.000000000000000000, -0.000000000000000000 ) ) ;
#72209 = CARTESIAN_POINT ( 'NONE',  ( 6.249999999999930722, 12.50000000000000000, 7.188010851410848723 ) ) ;
#72210 = CARTESIAN_POINT ( 'NONE',  ( -11.69999999999999929, 12.50000000000000000, -4.395220292106237103 ) ) ;
#72211 = DIRECTION ( 'NONE',  ( 0.000000000000000000, -0.000000000000000000, 1.000000000000000000 ) ) ;
#72212 = EDGE_CURVE ( 'NONE', #115792, #31757, #81925, .T. ) ;
#72213 = DIRECTION ( 'NONE',  ( 0.000000000000000000, 0.000000000000000000, 1.000000000000000000 ) ) ;
#72214 = EDGE_CURVE ( 'NONE', #123959, #20030, #4085, .T. ) ;
#72215 = EDGE_CURVE ( 'NONE', #88410, #42865, #13937, .T. ) ;
#72216 = CARTESIAN_POINT ( 'NONE',  ( -2.900000000000030553, 2.500000000000000000, 5.122947341949749323 ) ) ;
#72217 = VERTEX_POINT ( 'NONE', #109466 ) ;
#72218 = LINE ( 'NONE', #3464, #42104 ) ;
#72219 = EDGE_LOOP ( 'NONE', ( #123243, #116350 ) ) ;
#72220 = DIRECTION ( 'NONE',  ( 0.000000000000000000, -0.000000000000000000, 1.000000000000000000 ) ) ;
#72221 = VECTOR ( 'NONE', #69250, 1000.000000000000000 ) ;
#72223 = EDGE_LOOP ( 'NONE', ( #45845, #116192, #87606, #96042 ) ) ;
#72222 = EDGE_CURVE ( 'NONE', #63429, #102522, #9977, .T. ) ;
#72224 = CARTESIAN_POINT ( 'NONE',  ( 4.399999999999939071, 2.500000000000000000, -0.3464101615137782364 ) ) ;
#72225 = ADVANCED_FACE ( 'NONE', ( #89820 ), #116943, .T. ) ;
#72226 = AXIS2_PLACEMENT_3D ( 'NONE', #78490, #79127, #76541 ) ;
#72227 = ORIENTED_EDGE ( 'NONE', *, *, #4945, .F. ) ;
#72228 = EDGE_CURVE ( 'NONE', #99657, #107914, #110112, .T. ) ;
#72229 = DIRECTION ( 'NONE',  ( 0.000000000000000000, 0.000000000000000000, 1.000000000000000000 ) ) ;
#72230 = ADVANCED_FACE ( 'NONE', ( #34791 ), #104434, .T. ) ;
#72231 = ADVANCED_FACE ( 'NONE', ( #2722 ), #79417, .T. ) ;
#72232 = AXIS2_PLACEMENT_3D ( 'NONE', #73178, #94104, #2483 ) ;
#72233 = CARTESIAN_POINT ( 'NONE',  ( -3.150000000000033218, 12.50000000000000000, -6.776507416713040577 ) ) ;
#72234 = EDGE_LOOP ( 'NONE', ( #82461, #128330, #114156, #49473 ) ) ;
#72235 = ORIENTED_EDGE ( 'NONE', *, *, #13510, .F. ) ;
#72236 = CARTESIAN_POINT ( 'NONE',  ( 9.599999999999917932, 2.500000000000000000, 0.6928203230275494784 ) ) ;
#72237 = DIRECTION ( 'NONE',  ( 0.000000000000000000, 0.000000000000000000, 1.000000000000000000 ) ) ;
#72238 = LINE ( 'NONE', #84622, #18801 ) ;
#72239 = CARTESIAN_POINT ( 'NONE',  ( 8.349999999999923261, 12.50000000000000000, -6.495190528383302464 ) ) ;
#72240 = EDGE_CURVE ( 'NONE', #11992, #100514, #112852, .T. ) ;
#72241 = CONICAL_SURFACE ( 'NONE', #101471, 0.1000000000000000472, 0.003490658503988666988 ) ;
#72242 = FACE_OUTER_BOUND ( 'NONE', #21790, .T. ) ;
#72243 = AXIS2_PLACEMENT_3D ( 'NONE', #111769, #11625, #122245 ) ;
#72244 = ORIENTED_EDGE ( 'NONE', *, *, #17145, .T. ) ;
#72245 = AXIS2_PLACEMENT_3D ( 'NONE', #55780, #26332, #66235 ) ;
#72246 = CARTESIAN_POINT ( 'NONE',  ( 2.500000000000002220, -2.500000000000000000, -8.999999999999998224 ) ) ;
#72247 = CONICAL_SURFACE ( 'NONE', #124457, 0.09999999999999982514, 0.003490658503988666988 ) ;
#72248 = ORIENTED_EDGE ( 'NONE', *, *, #52274, .T. ) ;
#72249 = DIRECTION ( 'NONE',  ( -1.000000000000000000, 0.000000000000000000, 0.000000000000000000 ) ) ;
#72251 = AXIS2_PLACEMENT_3D ( 'NONE', #106905, #27075, #35611 ) ;
#72250 = DIRECTION ( 'NONE',  ( 0.000000000000000000, 0.000000000000000000, -1.000000000000000000 ) ) ;
#72252 = VECTOR ( 'NONE', #26461, 1000.000000000000000 ) ;
#72253 = CONICAL_SURFACE ( 'NONE', #95231, 0.1000000000000002554, 0.003490658503988666988 ) ;
#72254 = CARTESIAN_POINT ( 'NONE',  ( 6.849999999999927702, 2.500000000000000000, 1.818653347947321475 ) ) ;
#72255 = FACE_OUTER_BOUND ( 'NONE', #35699, .T. ) ;
#72256 = DIRECTION ( 'NONE',  ( -0.000000000000000000, -1.000000000000000000, -0.000000000000000000 ) ) ;
#72257 = DIRECTION ( 'NONE',  ( 0.000000000000000000, 0.000000000000000000, 1.000000000000000000 ) ) ;
#72258 = DIRECTION ( 'NONE',  ( 0.000000000000000000, 0.000000000000000000, 1.000000000000000000 ) ) ;
#72259 = ORIENTED_EDGE ( 'NONE', *, *, #128966, .F. ) ;
#72260 = PLANE ( 'NONE',  #25002 ) ;
#72261 = FACE_OUTER_BOUND ( 'NONE', #117170, .T. ) ;
#72262 = DIRECTION ( 'NONE',  ( -0.000000000000000000, 1.000000000000000000, -0.000000000000000000 ) ) ;
#72263 = ORIENTED_EDGE ( 'NONE', *, *, #20914, .F. ) ;
#72264 = ORIENTED_EDGE ( 'NONE', *, *, #119268, .T. ) ;
#72265 = DIRECTION ( 'NONE',  ( 0.000000000000000000, 1.000000000000000000, 0.000000000000000000 ) ) ;
#72266 = EDGE_CURVE ( 'NONE', #87169, #85514, #58494, .T. ) ;
#72267 = ORIENTED_EDGE ( 'NONE', *, *, #47822, .T. ) ;
#72268 = PRODUCT ( 'Multi-Function Power _ Mode Button', 'Multi-Function Power _ Mode Button', '', ( #108567 ) ) ;
#72269 = ORIENTED_EDGE ( 'NONE', *, *, #7719, .F. ) ;
#72270 = CARTESIAN_POINT ( 'NONE',  ( -4.400000000000028777, 2.500000000000000000, -4.676537180435978769 ) ) ;
#72271 = CONICAL_SURFACE ( 'NONE', #109922, 0.09999999999999982514, 0.003490658503988666988 ) ;
#72272 = ORIENTED_EDGE ( 'NONE', *, *, #77041, .F. ) ;
#72273 = CARTESIAN_POINT ( 'NONE',  ( 16.58100817949905803, -2.557139044001862427, -6.067820687739756025 ) ) ;
#72274 = CARTESIAN_POINT ( 'NONE',  ( -9.150000000000009237, 2.500000000000000000, 2.857883832488649301 ) ) ;
#72275 = CARTESIAN_POINT ( 'NONE',  ( 16.53754090007008415, 0.4856821978169202358, 6.114873053042321871 ) ) ;
#72276 = CIRCLE ( 'NONE', #24148, 0.1000000000000000472 ) ;
#72277 = CONICAL_SURFACE ( 'NONE', #78637, 0.1000000000000002554, 0.003490658503988666988 ) ;
#72278 = EDGE_LOOP ( 'NONE', ( #50671, #83693 ) ) ;
#72279 = DIRECTION ( 'NONE',  ( 0.000000000000000000, 0.000000000000000000, 1.000000000000000000 ) ) ;
#72280 = CARTESIAN_POINT ( 'NONE',  ( -5.200000000000022382, 2.500000000000000000, 0.4464101615137735513 ) ) ;
#72281 = ADVANCED_FACE ( 'NONE', ( #123775 ), #75193, .T. ) ;
#72282 = VERTEX_POINT ( 'NONE', #124444 ) ;
#72283 = CIRCLE ( 'NONE', #34642, 0.06509327318403745899 ) ;
#72284 = ORIENTED_EDGE ( 'NONE', *, *, #106281, .F. ) ;
#72285 = AXIS2_PLACEMENT_3D ( 'NONE', #57496, #97409, #7728 ) ;
#72286 = ORIENTED_EDGE ( 'NONE', *, *, #73924, .T. ) ;
#72287 = FACE_OUTER_BOUND ( 'NONE', #17282, .T. ) ;
#72288 = CARTESIAN_POINT ( 'NONE',  ( 183.8229166673494319, -4.445597072760122614, 7.699999999999997513 ) ) ;
#72289 = PLANE ( 'NONE',  #102750 ) ;
#72290 = FACE_BOUND ( 'NONE', #103872, .T. ) ;
#72291 = ORIENTED_EDGE ( 'NONE', *, *, #47576, .T. ) ;
#72292 = CARTESIAN_POINT ( 'NONE',  ( 5.199999999999937117, 12.50000000000000000, -4.676537180435978769 ) ) ;
#72293 = DIRECTION ( 'NONE',  ( 0.000000000000000000, 0.000000000000000000, 1.000000000000000000 ) ) ;
#72294 = ORIENTED_EDGE ( 'NONE', *, *, #36207, .F. ) ;
#72295 = DIRECTION ( 'NONE',  ( -0.000000000000000000, -1.000000000000000000, -0.000000000000000000 ) ) ;
#72297 = DIRECTION ( 'NONE',  ( 0.000000000000000000, 0.000000000000000000, 1.000000000000000000 ) ) ;
#72296 = AXIS2_PLACEMENT_3D ( 'NONE', #43482, #103021, #13347 ) ;
#72298 = AXIS2_PLACEMENT_3D ( 'NONE', #56368, #34173, #4669 ) ;
#72299 = PLANE ( 'NONE',  #75769 ) ;
#72300 = DIRECTION ( 'NONE',  ( 0.000000000000000000, 0.000000000000000000, -1.000000000000000000 ) ) ;
#72301 = CARTESIAN_POINT ( 'NONE',  ( -8.750000000000010658, 2.500000000000000000, 2.957883832488649389 ) ) ;
#72302 = DIRECTION ( 'NONE',  ( 0.000000000000000000, -0.9999939076577903929, 0.003490651415223739937 ) ) ;
#72303 = DIRECTION ( 'NONE',  ( 0.000000000000000000, 0.000000000000000000, 1.000000000000000000 ) ) ;
#72304 = EDGE_CURVE ( 'NONE', #72798, #52727, #84517, .T. ) ;
#72305 = VERTEX_POINT ( 'NONE', #34138 ) ;
#72306 = EDGE_LOOP ( 'NONE', ( #97748, #37962, #6786, #66053 ) ) ;
#72307 = ORIENTED_EDGE ( 'NONE', *, *, #16166, .T. ) ;
#72308 = VERTEX_POINT ( 'NONE', #55059 ) ;
#72309 = DIRECTION ( 'NONE',  ( 0.000000000000000000, 1.000000000000000000, 0.000000000000000000 ) ) ;
#72310 = DIRECTION ( 'NONE',  ( -4.274815082592931898E-19, -0.9999939076577903929, -0.003490651415223739937 ) ) ;
#72311 = DIRECTION ( 'NONE',  ( 0.000000000000000000, 0.000000000000000000, 1.000000000000000000 ) ) ;
#72312 = ORIENTED_EDGE ( 'NONE', *, *, #123740, .T. ) ;
#72313 = FACE_BOUND ( 'NONE', #44187, .T. ) ;
#72314 = ADVANCED_FACE ( 'NONE', ( #45244 ), #106578, .T. ) ;
#72315 = DIRECTION ( 'NONE',  ( 0.000000000000000000, 1.000000000000000000, 0.000000000000000000 ) ) ;
#72316 = CARTESIAN_POINT ( 'NONE',  ( 2.499999999999948930, 2.500000000000000000, -0.6928203230275541413 ) ) ;
#72317 = CARTESIAN_POINT ( 'NONE',  ( -6.650000000000014566, 12.50000000000000000, 1.407149913249508000 ) ) ;
#72318 = CIRCLE ( 'NONE', #3259, 0.06509327318403745899 ) ;
#72319 = DIRECTION ( 'NONE',  ( -0.000000000000000000, -1.000000000000000000, -0.000000000000000000 ) ) ;
#72320 = CIRCLE ( 'NONE', #122487, 0.1000000000000002554 ) ;
#72321 = DIRECTION ( 'NONE',  ( 0.000000000000000000, 0.000000000000000000, 1.000000000000000000 ) ) ;
#72322 = EDGE_CURVE ( 'NONE', #129134, #124382, #74699, .T. ) ;
#72323 = CARTESIAN_POINT ( 'NONE',  ( 1.049999999999954969, 12.50000000000000000, -6.841600689897077814 ) ) ;
#72324 = EDGE_CURVE ( 'NONE', #99720, #113921, #54267, .T. ) ;
#72325 = DIRECTION ( 'NONE',  ( 0.000000000000000000, 0.000000000000000000, 1.000000000000000000 ) ) ;
#72326 = DIRECTION ( 'NONE',  ( -0.000000000000000000, -1.000000000000000000, -0.000000000000000000 ) ) ;
#72327 = EDGE_CURVE ( 'NONE', #8589, #83800, #43822, .T. ) ;
#72328 = FACE_OUTER_BOUND ( 'NONE', #98391, .T. ) ;
#72329 = ADVANCED_FACE ( 'NONE', ( #33502 ), #73142, .T. ) ;
#72330 = ADVANCED_FACE ( 'NONE', ( #63594 ), #27084, .T. ) ;
#72331 = EDGE_LOOP ( 'NONE', ( #129518, #126634, #99837, #35430 ) ) ;
#72332 = EDGE_LOOP ( 'NONE', ( #72432, #113867 ) ) ;
#72333 = ORIENTED_EDGE ( 'NONE', *, *, #15560, .F. ) ;
#72334 = EDGE_LOOP ( 'NONE', ( #18635, #44395, #9083, #52045 ) ) ;
#72335 = EDGE_LOOP ( 'NONE', ( #5861, #42962, #96337, #120709 ) ) ;
#72336 = ORIENTED_EDGE ( 'NONE', *, *, #50360, .T. ) ;
#72337 = VECTOR ( 'NONE', #19257, 1000.000000000000000 ) ;
#72338 = DIRECTION ( 'NONE',  ( 1.000000000000000000, 0.000000000000000000, 0.000000000000000000 ) ) ;
#72339 = ORIENTED_EDGE ( 'NONE', *, *, #122118, .T. ) ;
#72340 = ADVANCED_FACE ( 'NONE', ( #113978 ), #6301, .T. ) ;
#72341 = VERTEX_POINT ( 'NONE', #82596 ) ;
#72342 = EDGE_CURVE ( 'NONE', #102565, #40749, #122513, .T. ) ;
#72343 = AXIS2_PLACEMENT_3D ( 'NONE', #11930, #32250, #102883 ) ;
#72344 = EDGE_CURVE ( 'NONE', #121499, #49607, #102849, .T. ) ;
#72345 = CARTESIAN_POINT ( 'NONE',  ( -4.200000000000025935, 2.500000000000000000, 4.330127018922196314 ) ) ;
#72346 = DIRECTION ( 'NONE',  ( 0.000000000000000000, 0.000000000000000000, 1.000000000000000000 ) ) ;
#72347 = CARTESIAN_POINT ( 'NONE',  ( -5.850000000000021849, 12.50000000000000000, -1.537336459617587581 ) ) ;
#72349 = AXIS2_PLACEMENT_3D ( 'NONE', #71925, #61464, #31356 ) ;
#72348 = DIRECTION ( 'NONE',  ( 0.000000000000000000, 0.000000000000000000, 1.000000000000000000 ) ) ;
#72350 = ORIENTED_EDGE ( 'NONE', *, *, #55551, .T. ) ;
#72351 = CARTESIAN_POINT ( 'NONE',  ( 187.5000000000000000, 0.000000000000000000, 7.700000000000000178 ) ) ;
#72352 = VERTEX_POINT ( 'NONE', #73397 ) ;
#72353 = ORIENTED_EDGE ( 'NONE', *, *, #45455, .F. ) ;
#72354 = DIRECTION ( 'NONE',  ( 0.000000000000000000, 1.000000000000000000, 0.000000000000000000 ) ) ;
#72355 = DIRECTION ( 'NONE',  ( 0.000000000000000000, 0.000000000000000000, 1.000000000000000000 ) ) ;
#72356 = VECTOR ( 'NONE', #95493, 1000.000000000000000 ) ;
#72357 = EDGE_LOOP ( 'NONE', ( #106506, #93131 ) ) ;
#72358 = EDGE_LOOP ( 'NONE', ( #23287, #30588 ) ) ;
#72359 = CARTESIAN_POINT ( 'NONE',  ( 7.299999999999927880, 2.500000000000000000, -4.776537180435977525 ) ) ;
#72360 = CARTESIAN_POINT ( 'NONE',  ( 10.84999999999990905, 12.50000000000000000, -7.253104124594891289 ) ) ;
#72361 = CARTESIAN_POINT ( 'NONE',  ( -3.750000000000025757, 2.500000000000000000, 1.472243186433545459 ) ) ;
#72362 = FACE_OUTER_BOUND ( 'NONE', #23327, .T. ) ;
#72363 = CARTESIAN_POINT ( 'NONE',  ( 3.549999999999942091, 2.500000000000000000, 2.411473670974873862 ) ) ;
#72364 = VECTOR ( 'NONE', #94207, 1000.000000000000000 ) ;
#72365 = AXIS2_PLACEMENT_3D ( 'NONE', #62950, #61013, #81312 ) ;
#72366 = EDGE_LOOP ( 'NONE', ( #61358, #54539, #22424, #115259 ) ) ;
#72367 = ADVANCED_FACE ( 'NONE', ( #83240 ), #93693, .T. ) ;
#72369 = VECTOR ( 'NONE', #114777, 1000.000000000000000 ) ;
#72368 = CARTESIAN_POINT ( 'NONE',  ( 7.499999999999925393, 12.50000000000000000, -0.6928203230275541413 ) ) ;
#72370 = EDGE_LOOP ( 'NONE', ( #115407, #36765, #32316, #118345 ) ) ;
#72371 = AXIS2_PLACEMENT_3D ( 'NONE', #59599, #101428, #80511 ) ;
#72373 = EDGE_CURVE ( 'NONE', #58339, #39516, #89945, .T. ) ;
#72372 = CARTESIAN_POINT ( 'NONE',  ( 17.50000000000000000, 2.499999999999999556, 0.6666666666666699603 ) ) ;
#72374 = DIRECTION ( 'NONE',  ( 0.000000000000000000, 0.000000000000000000, 1.000000000000000000 ) ) ;
#72375 = DIRECTION ( 'NONE',  ( 0.000000000000000000, 0.000000000000000000, 1.000000000000000000 ) ) ;
#72376 = PLANE ( 'NONE',  #15183 ) ;
#72377 = EDGE_CURVE ( 'NONE', #3400, #54303, #18842, .T. ) ;
#72378 = DIRECTION ( 'NONE',  ( -0.000000000000000000, -1.000000000000000000, -0.000000000000000000 ) ) ;
#72379 = ORIENTED_EDGE ( 'NONE', *, *, #99833, .F. ) ;
#72380 = AXIS2_PLACEMENT_3D ( 'NONE', #73875, #3842, #113809 ) ;
#72381 = EDGE_CURVE ( 'NONE', #12969, #40542, #8372, .T. ) ;
#72382 = CARTESIAN_POINT ( 'NONE',  ( 5.449999999999934452, 2.500000000000000000, 2.065063509461097624 ) ) ;
#72385 = EDGE_CURVE ( 'NONE', #70518, #67980, #119608, .T. ) ;
#72384 = VECTOR ( 'NONE', #78284, 1000.000000000000000 ) ;
#72383 = CONICAL_SURFACE ( 'NONE', #126658, 0.1000000000000002554, 0.003490658503988666988 ) ;
#72386 = CARTESIAN_POINT ( 'NONE',  ( -12.69999999999999396, 2.500000000000000000, -3.883716857408423984 ) ) ;
#72387 = ORIENTED_EDGE ( 'NONE', *, *, #59381, .F. ) ;
#72388 = ORIENTED_EDGE ( 'NONE', *, *, #6821, .F. ) ;
#72389 = ORIENTED_EDGE ( 'NONE', *, *, #11631, .F. ) ;
#72390 = CARTESIAN_POINT ( 'NONE',  ( -4.550000000000022915, 2.500000000000000000, -2.165063509461101710 ) ) ;
#72391 = CARTESIAN_POINT ( 'NONE',  ( 8.949999999999921130, 12.50000000000000000, 1.753560074763284016 ) ) ;
#72392 = CARTESIAN_POINT ( 'NONE',  ( 186.4010416670080588, -4.367472073101519747, 7.564683531249999149 ) ) ;
#72393 = CARTESIAN_POINT ( 'NONE',  ( -11.64999999999999680, 12.50000000000000000, 7.188010851410848723 ) ) ;
#72394 = EDGE_CURVE ( 'NONE', #3125, #60519, #39803, .T. ) ;
#72395 = DIRECTION ( 'NONE',  ( 0.000000000000000000, 1.000000000000000000, 0.000000000000000000 ) ) ;
#72396 = CARTESIAN_POINT ( 'NONE',  ( 16.68631762705676636, 1.607367762582524451, -5.954228785333302021 ) ) ;
#72397 = DIRECTION ( 'NONE',  ( 0.000000000000000000, 1.000000000000000000, 0.000000000000000000 ) ) ;
#72398 = CARTESIAN_POINT ( 'NONE',  ( 11.89999999999990798, 12.50000000000000000, -4.676537180435977881 ) ) ;
#72399 = VERTEX_POINT ( 'NONE', #69878 ) ;
#72400 = LINE ( 'NONE', #22657, #46388 ) ;
#72401 = DIRECTION ( 'NONE',  ( 0.000000000000000000, -0.000000000000000000, 1.000000000000000000 ) ) ;
#72402 = EDGE_CURVE ( 'NONE', #36233, #99874, #112945, .T. ) ;
#72403 = DIRECTION ( 'NONE',  ( 0.000000000000000000, 0.000000000000000000, -1.000000000000000000 ) ) ;
#72404 = DIRECTION ( 'NONE',  ( 0.000000000000000000, -0.000000000000000000, -1.000000000000000000 ) ) ;
#72405 = ORIENTED_EDGE ( 'NONE', *, *, #42146, .F. ) ;
#72406 = DIRECTION ( 'NONE',  ( -0.000000000000000000, -1.000000000000000000, -0.000000000000000000 ) ) ;
#72407 = AXIS2_PLACEMENT_3D ( 'NONE', #38771, #28935, #29562 ) ;
#72408 = DIRECTION ( 'NONE',  ( -0.000000000000000000, -1.000000000000000000, -0.000000000000000000 ) ) ;
#72410 = ORIENTED_EDGE ( 'NONE', *, *, #64156, .T. ) ;
#72409 = DIRECTION ( 'NONE',  ( 0.000000000000000000, 1.000000000000000000, 0.000000000000000000 ) ) ;
#72411 = VERTEX_POINT ( 'NONE', #108501 ) ;
#72413 = AXIS2_PLACEMENT_3D ( 'NONE', #80979, #81612, #29953 ) ;
#72412 = AXIS2_PLACEMENT_3D ( 'NONE', #49884, #108, #40050 ) ;
#72414 = LINE ( 'NONE', #69827, #65637 ) ;
#72415 = EDGE_CURVE ( 'NONE', #83060, #56205, #35584, .T. ) ;
#72416 = ORIENTED_EDGE ( 'NONE', *, *, #37782, .T. ) ;
#72417 = EDGE_LOOP ( 'NONE', ( #5668, #49167 ) ) ;
#72418 = DIRECTION ( 'NONE',  ( -0.000000000000000000, 1.000000000000000000, -0.000000000000000000 ) ) ;
#72419 = DIRECTION ( 'NONE',  ( -0.000000000000000000, 1.000000000000000000, -0.000000000000000000 ) ) ;
#72420 = CARTESIAN_POINT ( 'NONE',  ( -12.49999999999999289, 2.500000000000000000, 3.737306695894644371 ) ) ;
#72422 = CIRCLE ( 'NONE', #43187, 0.1000000000000000472 ) ;
#72421 = CIRCLE ( 'NONE', #84931, 0.06509327318403745899 ) ;
#72423 = CARTESIAN_POINT ( 'NONE',  ( 13.29999999999990301, 2.500000000000000000, -4.330127018922201643 ) ) ;
#72424 = EDGE_LOOP ( 'NONE', ( #112793, #38666, #61743, #9166 ) ) ;
#72425 = AXIS2_PLACEMENT_3D ( 'NONE', #36627, #76538, #16297 ) ;
#72426 = DIRECTION ( 'NONE',  ( 0.000000000000000000, 1.000000000000000000, 0.000000000000000000 ) ) ;
#72427 = VERTEX_POINT ( 'NONE', #58769 ) ;
#72428 = DIRECTION ( 'NONE',  ( 0.000000000000000000, 0.000000000000000000, -1.000000000000000000 ) ) ;
#72429 = EDGE_CURVE ( 'NONE', #14821, #78690, #56488, .T. ) ;
#72430 = FACE_OUTER_BOUND ( 'NONE', #52337, .T. ) ;
#72431 = ORIENTED_EDGE ( 'NONE', *, *, #104508, .F. ) ;
#72432 = ORIENTED_EDGE ( 'NONE', *, *, #96035, .T. ) ;
#72433 = ORIENTED_EDGE ( 'NONE', *, *, #70847, .F. ) ;
#72434 = VERTEX_POINT ( 'NONE', #49609 ) ;
#72435 = DIRECTION ( 'NONE',  ( 0.000000000000000000, 0.000000000000000000, -1.000000000000000000 ) ) ;
#72436 = CARTESIAN_POINT ( 'NONE',  ( 13.80679872386854790, 1.500000000000063727, 7.946844943073665846 ) ) ;
#72437 = DIRECTION ( 'NONE',  ( -0.000000000000000000, -1.000000000000000000, -0.000000000000000000 ) ) ;
#72438 = FACE_BOUND ( 'NONE', #103867, .T. ) ;
#72439 = ORIENTED_EDGE ( 'NONE', *, *, #116543, .T. ) ;
#72440 = AXIS2_PLACEMENT_3D ( 'NONE', #68601, #67956, #50266 ) ;
#72441 = CARTESIAN_POINT ( 'NONE',  ( 184.5312500006828031, 9.429780353434619030E-16, -7.700000000000000178 ) ) ;
#72442 = DIRECTION ( 'NONE',  ( 0.000000000000000000, 1.000000000000000000, 0.000000000000000000 ) ) ;
#72443 = DIRECTION ( 'NONE',  ( 0.000000000000000000, 0.000000000000000000, 1.000000000000000000 ) ) ;
#72444 = VECTOR ( 'NONE', #281, 1000.000000000000000 ) ;
#72445 = CARTESIAN_POINT ( 'NONE',  ( 179.5000000000000000, 0.000000000000000000, 0.000000000000000000 ) ) ;
#72446 = CONICAL_SURFACE ( 'NONE', #126859, 0.09999999999999982514, 0.003490658503988666988 ) ;
#72447 = CARTESIAN_POINT ( 'NONE',  ( -10.40000000000000213, 12.50000000000000000, 4.265033745738159077 ) ) ;
#72448 = FACE_OUTER_BOUND ( 'NONE', #73128, .T. ) ;
#72449 = AXIS2_PLACEMENT_3D ( 'NONE', #24317, #98680, #9014 ) ;
#72450 = AXIS2_PLACEMENT_3D ( 'NONE', #57808, #98354, #59098 ) ;
#72451 = DIRECTION ( 'NONE',  ( 0.000000000000000000, 0.000000000000000000, -1.000000000000000000 ) ) ;
#72452 = AXIS2_PLACEMENT_3D ( 'NONE', #22880, #62800, #62164 ) ;
#72453 = EDGE_CURVE ( 'NONE', #71159, #16443, #110784, .T. ) ;
#72454 = ORIENTED_EDGE ( 'NONE', *, *, #70117, .T. ) ;
#72455 = ORIENTED_EDGE ( 'NONE', *, *, #61064, .F. ) ;
#72456 = VERTEX_POINT ( 'NONE', #115227 ) ;
#72457 = VERTEX_POINT ( 'NONE', #96251 ) ;
#72458 = VERTEX_POINT ( 'NONE', #95630 ) ;
#72459 = DIRECTION ( 'NONE',  ( 0.000000000000000000, 0.000000000000000000, 1.000000000000000000 ) ) ;
#72460 = CARTESIAN_POINT ( 'NONE',  ( 8.949999999999917577, 2.500000000000000000, -2.411473670974877859 ) ) ;
#72461 = VERTEX_POINT ( 'NONE', #90135 ) ;
#72462 = FACE_BOUND ( 'NONE', #19999, .T. ) ;
#72464 = DIRECTION ( 'NONE',  ( 0.000000000000000000, 0.000000000000000000, 1.000000000000000000 ) ) ;
#72463 = CIRCLE ( 'NONE', #89276, 0.06509327318403745899 ) ;
#72465 = ADVANCED_FACE ( 'NONE', ( #20131 ), #94069, .T. ) ;
#72466 = AXIS2_PLACEMENT_3D ( 'NONE', #32609, #73149, #52223 ) ;
#72467 = ORIENTED_EDGE ( 'NONE', *, *, #22987, .T. ) ;
#72468 = EDGE_CURVE ( 'NONE', #74932, #16115, #100336, .T. ) ;
#72469 = DIRECTION ( 'NONE',  ( 0.000000000000000000, 0.000000000000000000, 1.000000000000000000 ) ) ;
#72470 = ADVANCED_FACE ( 'NONE', ( #106093 ), #69013, .T. ) ;
#72471 = DIRECTION ( 'NONE',  ( 0.000000000000000000, 1.000000000000000000, 0.000000000000000000 ) ) ;
#72472 = ADVANCED_FACE ( 'NONE', ( #25577 ), #85740, .T. ) ;
#72473 = DIRECTION ( 'NONE',  ( 0.000000000000000000, 1.000000000000000000, 0.000000000000000000 ) ) ;
#72474 = ADVANCED_FACE ( 'NONE', ( #5931 ), #73235, .T. ) ;
#72475 = ORIENTED_EDGE ( 'NONE', *, *, #89326, .F. ) ;
#72476 = DIRECTION ( 'NONE',  ( -4.274815082592931898E-19, -0.9999939076577903929, -0.003490651415223739937 ) ) ;
#72477 = ORIENTED_EDGE ( 'NONE', *, *, #119160, .T. ) ;
#72478 = EDGE_LOOP ( 'NONE', ( #114654, #64912, #88464, #94532 ) ) ;
#72479 = EDGE_CURVE ( 'NONE', #92776, #73985, #46049, .T. ) ;
#72480 = ORIENTED_EDGE ( 'NONE', *, *, #126989, .F. ) ;
#72481 = CARTESIAN_POINT ( 'NONE',  ( -11.25000000000000000, 12.50000000000000000, 2.857883832488649301 ) ) ;
#72482 = EDGE_CURVE ( 'NONE', #112003, #92128, #98673, .T. ) ;
#72483 = CARTESIAN_POINT ( 'NONE',  ( 184.5000000000000000, 9.429780353434619030E-16, 7.699999999999999289 ) ) ;
#72484 = DIRECTION ( 'NONE',  ( 0.000000000000000000, 0.000000000000000000, 1.000000000000000000 ) ) ;
#72485 = VERTEX_POINT ( 'NONE', #29313 ) ;
#72486 = EDGE_CURVE ( 'NONE', #896, #120378, #62, .T. ) ;
#72487 = CARTESIAN_POINT ( 'NONE',  ( 0.5999999999999621192, 2.500000000000000000, 0.2464101615137758439 ) ) ;
#72488 = ADVANCED_FACE ( 'NONE', ( #111059 ), #110435, .T. ) ;
#72489 = DIRECTION ( 'NONE',  ( 0.000000000000000000, 0.000000000000000000, 1.000000000000000000 ) ) ;
#72490 = EDGE_CURVE ( 'NONE', #60519, #3125, #16766, .T. ) ;
#72491 = FACE_OUTER_BOUND ( 'NONE', #35641, .T. ) ;
#72492 = CARTESIAN_POINT ( 'NONE',  ( -9.150000000000009237, 12.50000000000000000, -2.099970236277064473 ) ) ;
#72493 = CARTESIAN_POINT ( 'NONE',  ( 186.4895833340161175, -4.445597072760115509, -7.700000000000001954 ) ) ;
#72494 = VERTEX_POINT ( 'NONE', #22726 ) ;
#72495 = PLANE ( 'NONE',  #64150 ) ;
#72496 = EDGE_CURVE ( 'NONE', #33663, #63648, #100607, .T. ) ;
#72497 = EDGE_LOOP ( 'NONE', ( #8574, #59769 ) ) ;
#72498 = DIRECTION ( 'NONE',  ( 0.000000000000000000, 0.000000000000000000, -1.000000000000000000 ) ) ;
#72499 = AXIS2_PLACEMENT_3D ( 'NONE', #22281, #29507, #62203 ) ;
#72500 = EDGE_LOOP ( 'NONE', ( #128625, #118007, #53779, #51954 ) ) ;
#72501 = CIRCLE ( 'NONE', #110055, 0.06509327318403745899 ) ;
#72502 = ORIENTED_EDGE ( 'NONE', *, *, #62288, .F. ) ;
#72503 = PLANE ( 'NONE',  #30459 ) ;
#72504 = DIRECTION ( 'NONE',  ( 0.000000000000000000, 1.000000000000000000, 0.000000000000000000 ) ) ;
#72505 = DIRECTION ( 'NONE',  ( 0.000000000000000000, 1.000000000000000000, 0.000000000000000000 ) ) ;
#72506 = CARTESIAN_POINT ( 'NONE',  ( 12.89999999999990088, 2.500000000000000000, -4.430127018922202176 ) ) ;
#72507 = FACE_OUTER_BOUND ( 'NONE', #71872, .T. ) ;
#72508 = EDGE_LOOP ( 'NONE', ( #91267, #111889, #107261, #44914 ) ) ;
#72511 = ORIENTED_EDGE ( 'NONE', *, *, #24651, .F. ) ;
#72510 = VECTOR ( 'NONE', #54093, 1000.000000000000000 ) ;
#72509 = AXIS2_PLACEMENT_3D ( 'NONE', #64186, #34753, #53728 ) ;
#72512 = CARTESIAN_POINT ( 'NONE',  ( 9.999999999999911182, 2.500000000000000000, 5.022947341949748790 ) ) ;
#72513 = DIRECTION ( 'NONE',  ( 0.000000000000000000, 0.000000000000000000, 1.000000000000000000 ) ) ;
#72514 = DIRECTION ( 'NONE',  ( 0.000000000000000000, 0.000000000000000000, 1.000000000000000000 ) ) ;
#72515 = ORIENTED_EDGE ( 'NONE', *, *, #98731, .T. ) ;
#72516 = ORIENTED_EDGE ( 'NONE', *, *, #103795, .F. ) ;
#72517 = AXIS2_PLACEMENT_3D ( 'NONE', #76019, #104814, #95026 ) ;
#72518 = LINE ( 'NONE', #126110, #16379 ) ;
#72520 = VECTOR ( 'NONE', #10452, 1000.000000000000000 ) ;
#72519 = AXIS2_PLACEMENT_3D ( 'NONE', #20391, #31497, #49226 ) ;
#72521 = ORIENTED_EDGE ( 'NONE', *, *, #83900, .T. ) ;
#72522 = LINE ( 'NONE', #60555, #102976 ) ;
#72523 = DIRECTION ( 'NONE',  ( 0.000000000000000000, 0.000000000000000000, 1.000000000000000000 ) ) ;
#72524 = CONICAL_SURFACE ( 'NONE', #105954, 0.1000000000000000472, 0.003490658503988666988 ) ;
#72525 = LINE ( 'NONE', #3134, #76252 ) ;
#72526 = ORIENTED_EDGE ( 'NONE', *, *, #67428, .T. ) ;
#72527 = PLANE ( 'NONE',  #14696 ) ;
#72528 = CARTESIAN_POINT ( 'NONE',  ( -7.900000000000014566, 12.50000000000000000, -4.330127018922201643 ) ) ;
#72529 = CARTESIAN_POINT ( 'NONE',  ( -5.800000000000018474, 2.500000000000000000, 0.09999999999999772959 ) ) ;
#72530 = DIRECTION ( 'NONE',  ( 0.000000000000000000, 1.000000000000000000, 0.000000000000000000 ) ) ;
#72531 = DIRECTION ( 'NONE',  ( 0.000000000000000000, -0.000000000000000000, 1.000000000000000000 ) ) ;
#72532 = ORIENTED_EDGE ( 'NONE', *, *, #31383, .F. ) ;
#72533 = EDGE_CURVE ( 'NONE', #10550, #40796, #27162, .T. ) ;
#72534 = CARTESIAN_POINT ( 'NONE',  ( 97.50000000000000000, 9.184850993605147944E-16, -7.500000000000000000 ) ) ;
#72536 = EDGE_CURVE ( 'NONE', #90750, #75566, #50254, .T. ) ;
#72535 = CARTESIAN_POINT ( 'NONE',  ( 9.999999999999948486, 12.50000000000000000, 4.330127018922196314 ) ) ;
#72537 = ORIENTED_EDGE ( 'NONE', *, *, #106725, .F. ) ;
#72538 = ORIENTED_EDGE ( 'NONE', *, *, #70404, .T. ) ;
#72539 = CARTESIAN_POINT ( 'NONE',  ( 186.6302083336747160, -4.367472073101514418, -7.564683531250002702 ) ) ;
#72540 = CARTESIAN_POINT ( 'NONE',  ( 13.29999999999990301, 2.500000000000000000, -4.230127018922201998 ) ) ;
#72541 = CIRCLE ( 'NONE', #124754, 0.06509327318403745899 ) ;
#72542 = CARTESIAN_POINT ( 'NONE',  ( 0.1999999999999571565, 12.50000000000000000, 4.048810130592458201 ) ) ;
#72543 = VECTOR ( 'NONE', #66038, 1000.000000000000000 ) ;
#72545 = AXIS2_PLACEMENT_3D ( 'NONE', #59634, #49803, #32 ) ;
#72544 = DIRECTION ( 'NONE',  ( 0.000000000000000000, 0.000000000000000000, 1.000000000000000000 ) ) ;
#72546 = EDGE_CURVE ( 'NONE', #101260, #22692, #123306, .T. ) ;
#72547 = CARTESIAN_POINT ( 'NONE',  ( 2.299999999999949640, 2.500000000000000000, -4.776537180435977525 ) ) ;
#72548 = DIRECTION ( 'NONE',  ( 0.000000000000000000, 0.000000000000000000, -1.000000000000000000 ) ) ;
#72549 = AXIS2_PLACEMENT_3D ( 'NONE', #43466, #50685, #83383 ) ;
#72550 = DIRECTION ( 'NONE',  ( 0.000000000000000000, 0.000000000000000000, 1.000000000000000000 ) ) ;
#72551 = LINE ( 'NONE', #62729, #62343 ) ;
#72552 = AXIS2_PLACEMENT_3D ( 'NONE', #109147, #128170, #120282 ) ;
#72553 = CARTESIAN_POINT ( 'NONE',  ( -6.850000000000013856, 2.500000000000000000, 6.941600689897073018 ) ) ;
#72554 = ORIENTED_EDGE ( 'NONE', *, *, #88419, .F. ) ;
#72555 = EDGE_LOOP ( 'NONE', ( #18898, #79346 ) ) ;
#72556 = AXIS2_PLACEMENT_3D ( 'NONE', #78701, #68855, #59048 ) ;
#72557 = EDGE_LOOP ( 'NONE', ( #22120, #96688, #125584, #9873 ) ) ;
#72558 = VERTEX_POINT ( 'NONE', #121537 ) ;
#72559 = CIRCLE ( 'NONE', #126835, 0.1000000000000000472 ) ;
#72560 = DIRECTION ( 'NONE',  ( -0.000000000000000000, 1.000000000000000000, -0.000000000000000000 ) ) ;
#72561 = CARTESIAN_POINT ( 'NONE',  ( -8.750000000000007105, 2.500000000000000000, 7.188010851410848723 ) ) ;
#72562 = CIRCLE ( 'NONE', #65996, 0.1000000000000002554 ) ;
#72563 = ORIENTED_EDGE ( 'NONE', *, *, #123010, .F. ) ;
#72564 = FACE_BOUND ( 'NONE', #20887, .T. ) ;
#72566 = CIRCLE ( 'NONE', #45376, 0.09999999999999982514 ) ;
#72565 = CIRCLE ( 'NONE', #108047, 0.09999999999999982514 ) ;
#72567 = DIRECTION ( 'NONE',  ( 0.000000000000000000, 0.000000000000000000, -1.000000000000000000 ) ) ;
#72569 = ORIENTED_EDGE ( 'NONE', *, *, #23159, .T. ) ;
#72568 = LINE ( 'NONE', #22186, #24565 ) ;
#72570 = CARTESIAN_POINT ( 'NONE',  ( 4.399999999999939071, 2.500000000000000000, 0.2464101615137736789 ) ) ;
#72571 = DIRECTION ( 'NONE',  ( 0.000000000000000000, 1.000000000000000000, 0.000000000000000000 ) ) ;
#72572 = ORIENTED_EDGE ( 'NONE', *, *, #111932, .T. ) ;
#72573 = VERTEX_POINT ( 'NONE', #23333 ) ;
#72574 = ORIENTED_EDGE ( 'NONE', *, *, #80343, .T. ) ;
#72575 = EDGE_LOOP ( 'NONE', ( #86114, #81168, #109152, #14420 ) ) ;
#72576 = CARTESIAN_POINT ( 'NONE',  ( -6.071532165918824830E-15, 2.500000000000000000, -4.330127018922201643 ) ) ;
#72577 = LINE ( 'NONE', #89632, #13192 ) ;
#72578 = CARTESIAN_POINT ( 'NONE',  ( 21.24754738303297330, 0.7337760880902002292, -4.182111650399407132 ) ) ;
#72579 = DIRECTION ( 'NONE',  ( -4.274815082592931898E-19, -0.9999939076577903929, -0.003490651415223739937 ) ) ;
#72580 = ORIENTED_EDGE ( 'NONE', *, *, #105540, .T. ) ;
#72581 = CARTESIAN_POINT ( 'NONE',  ( 14.14999999999989733, 12.50000000000000000, 1.472243186433545459 ) ) ;
#72583 = ORIENTED_EDGE ( 'NONE', *, *, #37618, .F. ) ;
#72582 = ADVANCED_FACE ( 'NONE', ( #92077 ), #13516, .F. ) ;
#72584 = DIRECTION ( 'NONE',  ( -0.000000000000000000, -1.000000000000000000, -0.000000000000000000 ) ) ;
#72585 = CARTESIAN_POINT ( 'NONE',  ( 7.306656945318285246, -1.500000000000379918, -9.704971168320719599 ) ) ;
#72586 = FACE_OUTER_BOUND ( 'NONE', #22192, .T. ) ;
#72587 = CARTESIAN_POINT ( 'NONE',  ( -0.2000000000000404232, 2.500000000000000000, 4.083716857408421497 ) ) ;
#72588 = EDGE_CURVE ( 'NONE', #91712, #28130, #77346, .T. ) ;
#72589 = ORIENTED_EDGE ( 'NONE', *, *, #49495, .T. ) ;
#72590 = VECTOR ( 'NONE', #513, 1000.000000000000000 ) ;
#72591 = VERTEX_POINT ( 'NONE', #71813 ) ;
#72592 = ORIENTED_EDGE ( 'NONE', *, *, #123583, .T. ) ;
#72593 = CARTESIAN_POINT ( 'NONE',  ( -1.450000000000035039, 2.500000000000000000, -6.741600689897077281 ) ) ;
#72594 = CARTESIAN_POINT ( 'NONE',  ( -10.80000000000000071, 2.500000000000000000, -2.276824562219559311E-15 ) ) ;
#72595 = EDGE_CURVE ( 'NONE', #92706, #46131, #62645, .T. ) ;
#72596 = DIRECTION ( 'NONE',  ( -0.000000000000000000, -1.000000000000000000, -0.000000000000000000 ) ) ;
#72597 = FACE_BOUND ( 'NONE', #27179, .T. ) ;
#72598 = FACE_OUTER_BOUND ( 'NONE', #6546, .T. ) ;
#72599 = PLANE ( 'NONE',  #36139 ) ;
#72601 = AXIS2_PLACEMENT_3D ( 'NONE', #110752, #42029, #11911 ) ;
#72600 = VECTOR ( 'NONE', #44401, 1000.000000000000000 ) ;
#72602 = CARTESIAN_POINT ( 'NONE',  ( 7.299999999999926104, 12.50000000000000000, 4.676537180435972552 ) ) ;
#72603 = CARTESIAN_POINT ( 'NONE',  ( 186.9218750003414016, 0.000000000000000000, 7.564683531250000925 ) ) ;
#72604 = CARTESIAN_POINT ( 'NONE',  ( 0.6499999999999566125, 2.500000000000000000, -6.841600689897077814 ) ) ;
#72605 = CARTESIAN_POINT ( 'NONE',  ( 3.549999999999941203, 2.500000000000000000, 6.148780366869520897 ) ) ;
#72606 = VERTEX_POINT ( 'NONE', #1762 ) ;
#72608 = CIRCLE ( 'NONE', #18204, 0.1000000000000002554 ) ;
#72607 = VECTOR ( 'NONE', #27955, 1000.000000000000000 ) ;
#72609 = VECTOR ( 'NONE', #18524, 1000.000000000000000 ) ;
#72610 = LINE ( 'NONE', #81142, #37104 ) ;
#72611 = ORIENTED_EDGE ( 'NONE', *, *, #28597, .F. ) ;
#72612 = ORIENTED_EDGE ( 'NONE', *, *, #121845, .F. ) ;
#72613 = DIRECTION ( 'NONE',  ( -0.000000000000000000, -1.000000000000000000, -0.000000000000000000 ) ) ;
#72614 = FACE_OUTER_BOUND ( 'NONE', #24807, .T. ) ;
#72615 = FACE_BOUND ( 'NONE', #57596, .T. ) ;
#72616 = DIRECTION ( 'NONE',  ( -4.274815082592931898E-19, -0.9999939076577903929, -0.003490651415223739937 ) ) ;
#72617 = EDGE_CURVE ( 'NONE', #110704, #99929, #52170, .T. ) ;
#72618 = ORIENTED_EDGE ( 'NONE', *, *, #30254, .T. ) ;
#72619 = EDGE_CURVE ( 'NONE', #93363, #125180, #48100, .T. ) ;
#72620 = CARTESIAN_POINT ( 'NONE',  ( -0.8500000000000395017, 12.50000000000000000, 6.495190528383297135 ) ) ;
#72621 = EDGE_CURVE ( 'NONE', #76276, #105557, #98262, .T. ) ;
#72622 = DIRECTION ( 'NONE',  ( 0.000000000000000000, -0.9999939076577903929, 0.003490651415223739937 ) ) ;
#72623 = ADVANCED_FACE ( 'NONE', ( #122205 ), #50881, .T. ) ;
#72624 = AXIS2_PLACEMENT_3D ( 'NONE', #7911, #47863, #98228 ) ;
#72625 = EDGE_CURVE ( 'NONE', #69132, #18092, #41084, .T. ) ;
#72626 = EDGE_LOOP ( 'NONE', ( #100747, #53317, #124374, #31624 ) ) ;
#72627 = DIRECTION ( 'NONE',  ( -0.000000000000000000, 1.000000000000000000, -0.000000000000000000 ) ) ;
#72628 = AXIS2_PLACEMENT_3D ( 'NONE', #79659, #49820, #120474 ) ;
#72629 = CARTESIAN_POINT ( 'NONE',  ( 9.799999999999918998, 12.50000000000000000, -0.3464101615137782364 ) ) ;
#72630 = EDGE_CURVE ( 'NONE', #15958, #116681, #121571, .T. ) ;
#72631 = EDGE_LOOP ( 'NONE', ( #2265, #112330, #76661, #30189 ) ) ;
#72632 = DIRECTION ( 'NONE',  ( -0.000000000000000000, -1.000000000000000000, -0.000000000000000000 ) ) ;
#72633 = EDGE_CURVE ( 'NONE', #81018, #89491, #75598, .T. ) ;
#72634 = DIRECTION ( 'NONE',  ( 0.000000000000000000, 0.000000000000000000, 1.000000000000000000 ) ) ;
#72635 = AXIS2_PLACEMENT_3D ( 'NONE', #65704, #46077, #76179 ) ;
#72636 = CIRCLE ( 'NONE', #30788, 0.06509327318403745899 ) ;
#72637 = ORIENTED_EDGE ( 'NONE', *, *, #94026, .F. ) ;
#72638 = AXIS2_PLACEMENT_3D ( 'NONE', #15022, #125010, #103445 ) ;
#72639 = CARTESIAN_POINT ( 'NONE',  ( 13.54999999999989768, 2.500000000000000000, -2.611473670974877592 ) ) ;
#72640 = EDGE_CURVE ( 'NONE', #47032, #92847, #94470, .T. ) ;
#72641 = DIRECTION ( 'NONE',  ( -0.000000000000000000, 1.000000000000000000, -0.000000000000000000 ) ) ;
#72642 = DIRECTION ( 'NONE',  ( -0.000000000000000000, -1.000000000000000000, -0.000000000000000000 ) ) ;
#72643 = ORIENTED_EDGE ( 'NONE', *, *, #111103, .T. ) ;
#72644 = EDGE_LOOP ( 'NONE', ( #4138, #61998, #13340, #67727 ) ) ;
#72645 = AXIS2_PLACEMENT_3D ( 'NONE', #127553, #39202, #97442 ) ;
#72646 = EDGE_CURVE ( 'NONE', #10174, #119726, #125769, .T. ) ;
#72647 = DIRECTION ( 'NONE',  ( 0.000000000000000000, 1.000000000000000000, 0.000000000000000000 ) ) ;
#72648 = EDGE_CURVE ( 'NONE', #63986, #45554, #94020, .T. ) ;
#72649 = EDGE_LOOP ( 'NONE', ( #17988, #1098, #12733, #128855 ) ) ;
#72650 = CARTESIAN_POINT ( 'NONE',  ( 10.59999999999990905, 2.500000000000000000, -3.983716857408426293 ) ) ;
#72651 = FACE_OUTER_BOUND ( 'NONE', #46615, .T. ) ;
#72652 = VECTOR ( 'NONE', #53490, 1000.000000000000000 ) ;
#72653 = ORIENTED_EDGE ( 'NONE', *, *, #111009, .T. ) ;
#72654 = DIRECTION ( 'NONE',  ( 0.000000000000000000, 1.000000000000000000, 0.000000000000000000 ) ) ;
#72655 = LINE ( 'NONE', #104041, #73376 ) ;
#72656 = DIRECTION ( 'NONE',  ( -1.000000000000000000, -0.000000000000000000, -0.000000000000000000 ) ) ;
#72657 = CARTESIAN_POINT ( 'NONE',  ( 7.049999999999928768, 12.50000000000000000, 6.495190528383297135 ) ) ;
#72658 = DIRECTION ( 'NONE',  ( 0.000000000000000000, 0.000000000000000000, 1.000000000000000000 ) ) ;
#72659 = EDGE_CURVE ( 'NONE', #48660, #5028, #65840, .T. ) ;
#72660 = ORIENTED_EDGE ( 'NONE', *, *, #3032, .T. ) ;
#72661 = ORIENTED_EDGE ( 'NONE', *, *, #105736, .F. ) ;
#72662 = PLANE ( 'NONE',  #105998 ) ;
#72663 = ORIENTED_EDGE ( 'NONE', *, *, #66259, .T. ) ;
#72664 = CARTESIAN_POINT ( 'NONE',  ( -12.29999999999999361, 2.500000000000000000, 4.083716857408420609 ) ) ;
#72666 = ORIENTED_EDGE ( 'NONE', *, *, #10504, .T. ) ;
#72665 = VERTEX_POINT ( 'NONE', #16721 ) ;
#72667 = VERTEX_POINT ( 'NONE', #105781 ) ;
#72668 = AXIS2_PLACEMENT_3D ( 'NONE', #64729, #85010, #124304 ) ;
#72669 = DIRECTION ( 'NONE',  ( 0.000000000000000000, 0.000000000000000000, -1.000000000000000000 ) ) ;
#72670 = PLANE ( 'NONE',  #29729 ) ;
#72671 = DIRECTION ( 'NONE',  ( 0.000000000000000000, 1.000000000000000000, 0.000000000000000000 ) ) ;
#72672 = CARTESIAN_POINT ( 'NONE',  ( -10.40000000000000213, 2.500000000000000000, 0.7928203230275495672 ) ) ;
#72673 = CARTESIAN_POINT ( 'NONE',  ( 184.8229166673494888, -4.445597072760063107, 7.700000000000102318 ) ) ;
#72674 = FACE_OUTER_BOUND ( 'NONE', #59277, .T. ) ;
#72675 = FACE_OUTER_BOUND ( 'NONE', #6302, .T. ) ;
#72676 = CARTESIAN_POINT ( 'NONE',  ( -13.09999999999999076, 12.50000000000000000, 4.048810130592458201 ) ) ;
#72677 = DIRECTION ( 'NONE',  ( 0.000000000000000000, 0.000000000000000000, -1.000000000000000000 ) ) ;
#72679 = ORIENTED_EDGE ( 'NONE', *, *, #41155, .F. ) ;
#72678 = AXIS2_PLACEMENT_3D ( 'NONE', #114344, #24687, #104527 ) ;
#72680 = ADVANCED_FACE ( 'NONE', ( #95317 ), #77744, .T. ) ;
#72681 = AXIS2_PLACEMENT_3D ( 'NONE', #102354, #12655, #112815 ) ;
#72682 = EDGE_CURVE ( 'NONE', #85724, #58412, #65129, .T. ) ;
#72683 = CARTESIAN_POINT ( 'NONE',  ( 15.39999999999989022, 2.500000000000000000, -0.1000000000000023925 ) ) ;
#72684 = ORIENTED_EDGE ( 'NONE', *, *, #86705, .T. ) ;
#72685 = ORIENTED_EDGE ( 'NONE', *, *, #39372, .F. ) ;
#72686 = FACE_OUTER_BOUND ( 'NONE', #100888, .T. ) ;
#72687 = DIRECTION ( 'NONE',  ( 0.000000000000000000, 0.000000000000000000, -1.000000000000000000 ) ) ;
#72688 = DIRECTION ( 'NONE',  ( -4.274815082592931898E-19, -0.9999939076577903929, -0.003490651415223739937 ) ) ;
#72689 = AXIS2_PLACEMENT_3D ( 'NONE', #76227, #97145, #55926 ) ;
#72690 = DIRECTION ( 'NONE',  ( -0.000000000000000000, 1.000000000000000000, -0.000000000000000000 ) ) ;
#72691 = AXIS2_PLACEMENT_3D ( 'NONE', #127089, #58989, #26948 ) ;
#72692 = AXIS2_PLACEMENT_3D ( 'NONE', #39916, #97522, #50363 ) ;
#72693 = CARTESIAN_POINT ( 'NONE',  ( -14.34999999999998543, 12.50000000000000000, 2.511473670974877503 ) ) ;
#72694 = DIRECTION ( 'NONE',  ( 0.000000000000000000, 0.000000000000000000, 1.000000000000000000 ) ) ;
#72695 = DIRECTION ( 'NONE',  ( 0.000000000000000000, -0.000000000000000000, 1.000000000000000000 ) ) ;
#72696 = ORIENTED_EDGE ( 'NONE', *, *, #123890, .F. ) ;
#72697 = ORIENTED_EDGE ( 'NONE', *, *, #124484, .F. ) ;
#72698 = CONICAL_SURFACE ( 'NONE', #83170, 0.09999999999999982514, 0.003490658503988666988 ) ;
#72699 = VERTEX_POINT ( 'NONE', #65183 ) ;
#72700 = EDGE_LOOP ( 'NONE', ( #63074, #4294 ) ) ;
#72701 = AXIS2_PLACEMENT_3D ( 'NONE', #108273, #127916, #27142 ) ;
#72702 = ORIENTED_EDGE ( 'NONE', *, *, #31938, .F. ) ;
#72703 = DIRECTION ( 'NONE',  ( 0.000000000000000000, 0.000000000000000000, -1.000000000000000000 ) ) ;
#72704 = CARTESIAN_POINT ( 'NONE',  ( 7.899999999999921307, 2.500000000000000000, 0.09999999999999761857 ) ) ;
#72705 = CONICAL_SURFACE ( 'NONE', #116607, 0.1000000000000002554, 0.003490658503988666988 ) ;
#72706 = DIRECTION ( 'NONE',  ( -4.274815082592931898E-19, -0.9999939076577903929, -0.003490651415223739937 ) ) ;
#72707 = DIRECTION ( 'NONE',  ( 0.000000000000000000, 0.000000000000000000, 1.000000000000000000 ) ) ;
#72708 = CARTESIAN_POINT ( 'NONE',  ( 3.749999999999976907, 12.50000000000000000, 2.165063509461097713 ) ) ;
#72709 = EDGE_LOOP ( 'NONE', ( #60876, #35928, #75306, #84725 ) ) ;
#72710 = CARTESIAN_POINT ( 'NONE',  ( 7.499999999999925393, 2.500000000000000000, -0.7928203230275542301 ) ) ;
#72711 = DIRECTION ( 'NONE',  ( 0.000000000000000000, -0.000000000000000000, 1.000000000000000000 ) ) ;
#72712 = DIRECTION ( 'NONE',  ( 0.000000000000000000, 1.000000000000000000, 0.000000000000000000 ) ) ;
#72713 = CIRCLE ( 'NONE', #16244, 0.1000000000000000472 ) ;
#72714 = CONICAL_SURFACE ( 'NONE', #112432, 0.1000000000000002554, 0.003490658503988666988 ) ;
#72715 = CARTESIAN_POINT ( 'NONE',  ( 0.1999999999999562961, 12.50000000000000000, 4.676537180435972552 ) ) ;
#72716 = EDGE_CURVE ( 'NONE', #63975, #62965, #48423, .T. ) ;
#72717 = ORIENTED_EDGE ( 'NONE', *, *, #51746, .T. ) ;
#72718 = CIRCLE ( 'NONE', #53934, 0.09999999999999982514 ) ;
#72719 = ORIENTED_EDGE ( 'NONE', *, *, #28759, .T. ) ;
#72720 = ORIENTED_EDGE ( 'NONE', *, *, #58700, .F. ) ;
#72721 = DIRECTION ( 'NONE',  ( 0.000000000000000000, 0.000000000000000000, 1.000000000000000000 ) ) ;
#72722 = AXIS2_PLACEMENT_3D ( 'NONE', #10626, #49963, #29655 ) ;
#72723 = CIRCLE ( 'NONE', #16254, 0.09999999999999982514 ) ;
#72724 = CARTESIAN_POINT ( 'NONE',  ( -4.800000000000028244, 2.500000000000000000, -3.883716857408426648 ) ) ;
#72726 = ADVANCED_FACE ( 'NONE', ( #15442 ), #76322, .F. ) ;
#72725 = FACE_OUTER_BOUND ( 'NONE', #1068, .T. ) ;
#72727 = VECTOR ( 'NONE', #65973, 1000.000000000000000 ) ;
#72729 = EDGE_LOOP ( 'NONE', ( #103227, #78601 ) ) ;
#72728 = ADVANCED_FACE ( 'NONE', ( #85492 ), #33845, .T. ) ;
#72730 = CARTESIAN_POINT ( 'NONE',  ( -7.300000000000016698, 2.500000000000000000, -0.2464101615137783419 ) ) ;
#72732 = CIRCLE ( 'NONE', #14126, 0.06509327318403745899 ) ;
#72731 = DIRECTION ( 'NONE',  ( 0.000000000000000000, 0.000000000000000000, 1.000000000000000000 ) ) ;
#72733 = DIRECTION ( 'NONE',  ( 0.000000000000000000, 0.000000000000000000, 1.000000000000000000 ) ) ;
#72734 = EDGE_CURVE ( 'NONE', #91134, #54383, #2435, .T. ) ;
#72735 = DIRECTION ( 'NONE',  ( 0.000000000000000000, 0.000000000000000000, 1.000000000000000000 ) ) ;
#72737 = AXIS2_PLACEMENT_3D ( 'NONE', #76764, #96381, #26381 ) ;
#72736 = AXIS2_PLACEMENT_3D ( 'NONE', #53845, #123236, #73469 ) ;
#72738 = DIRECTION ( 'NONE',  ( 0.000000000000000000, 0.000000000000000000, 1.000000000000000000 ) ) ;
#72739 = EDGE_LOOP ( 'NONE', ( #104484, #39839 ) ) ;
#72740 =( BOUNDED_CURVE ( )  B_SPLINE_CURVE ( 2, ( #109023, #67826, #79590, #88084, #16770, #88763, #7612 ),
 .UNSPECIFIED., .F., .F. ) 
 B_SPLINE_CURVE_WITH_KNOTS ( ( 3, 2, 2, 3 ),
 ( 0.6428571428571433488, 0.6666666666666670737, 0.6904761904761910207, 0.7142857142857148567 ),
 .UNSPECIFIED. ) 
 CURVE ( )  GEOMETRIC_REPRESENTATION_ITEM ( )  RATIONAL_B_SPLINE_CURVE ( ( 0.9999999999999974465, 0.8660254037844412611, 1.000000000000000000, 0.8660254037844387076, 1.000000000000000000, 0.8660254037844355990, 1.000000000000003109 ) ) 
 REPRESENTATION_ITEM ( '' )  );
#72741 = VERTEX_POINT ( 'NONE', #125417 ) ;
#72742 = EDGE_CURVE ( 'NONE', #41595, #93259, #42166, .T. ) ;
#72743 = CARTESIAN_POINT ( 'NONE',  ( 11.24999999999994493, 12.50000000000000000, -2.230156782645139391 ) ) ;
#72744 = CARTESIAN_POINT ( 'NONE',  ( -6.650000000000015454, 2.500000000000000000, 2.857883832488649301 ) ) ;
#72745 = CARTESIAN_POINT ( 'NONE',  ( -9.150000000000009237, 12.50000000000000000, -1.537336459617587581 ) ) ;
#72746 = CARTESIAN_POINT ( 'NONE',  ( -3.750000000000027978, 12.50000000000000000, 7.253104124594885960 ) ) ;
#72747 = VERTEX_POINT ( 'NONE', #106416 ) ;
#72748 = ORIENTED_EDGE ( 'NONE', *, *, #87845, .T. ) ;
#72749 = DIRECTION ( 'NONE',  ( -0.000000000000000000, 1.000000000000000000, -0.000000000000000000 ) ) ;
#72750 = LINE ( 'NONE', #102833, #55167 ) ;
#72751 = CARTESIAN_POINT ( 'NONE',  ( 6.699999999999930012, 12.50000000000000000, 4.395220292106234439 ) ) ;
#72752 = DIRECTION ( 'NONE',  ( 0.000000000000000000, 1.000000000000000000, 0.000000000000000000 ) ) ;
#72753 = ORIENTED_EDGE ( 'NONE', *, *, #81135, .T. ) ;
#72754 = CARTESIAN_POINT ( 'NONE',  ( 12.69999999999990337, 2.500000000000000000, -4.776537180435978414 ) ) ;
#72755 = DIRECTION ( 'NONE',  ( 0.000000000000000000, 0.000000000000000000, -1.000000000000000000 ) ) ;
#72756 = ORIENTED_EDGE ( 'NONE', *, *, #18173, .F. ) ;
#72757 = CIRCLE ( 'NONE', #12111, 0.1000000000000002554 ) ;
#72758 = DIRECTION ( 'NONE',  ( -0.000000000000000000, 1.000000000000000000, -0.000000000000000000 ) ) ;
#72759 = VERTEX_POINT ( 'NONE', #124120 ) ;
#72760 = DIRECTION ( 'NONE',  ( 0.000000000000000000, 0.000000000000000000, 1.000000000000000000 ) ) ;
#72761 = EDGE_CURVE ( 'NONE', #70524, #39170, #102787, .T. ) ;
#72762 = CONICAL_SURFACE ( 'NONE', #66405, 0.09999999999999982514, 0.003490658503988666988 ) ;
#72763 = EDGE_LOOP ( 'NONE', ( #80316, #88920 ) ) ;
#72764 = DIRECTION ( 'NONE',  ( -0.000000000000000000, -1.000000000000000000, -0.000000000000000000 ) ) ;
#72765 = DIRECTION ( 'NONE',  ( -1.000000000000000000, -0.000000000000000000, -0.000000000000000000 ) ) ;
#72766 = ORIENTED_EDGE ( 'NONE', *, *, #63713, .F. ) ;
#72767 = EDGE_LOOP ( 'NONE', ( #60830, #70067, #79867, #61072 ) ) ;
#72768 = EDGE_CURVE ( 'NONE', #378, #64066, #56809, .T. ) ;
#72769 = CARTESIAN_POINT ( 'NONE',  ( 186.9218750003414016, 0.000000000000000000, 7.564683531250000925 ) ) ;
#72770 = DIRECTION ( 'NONE',  ( 1.000000000000000000, 0.000000000000000000, 0.000000000000000000 ) ) ;
#72772 = EDGE_CURVE ( 'NONE', #99935, #11527, #10838, .T. ) ;
#72771 = AXIS2_PLACEMENT_3D ( 'NONE', #64692, #66619, #73871 ) ;
#72773 = CARTESIAN_POINT ( 'NONE',  ( 187.2552083336747444, 6.551208109652275624, -3.782341765624998686 ) ) ;
#72774 = CARTESIAN_POINT ( 'NONE',  ( 186.1927083336747160, 6.551208109652275624, -3.782341765624998686 ) ) ;
#72775 = VECTOR ( 'NONE', #31385, 1000.000000000000000 ) ;
#72776 = DIRECTION ( 'NONE',  ( 0.000000000000000000, 0.000000000000000000, 1.000000000000000000 ) ) ;
#72777 = DIRECTION ( 'NONE',  ( -4.274815082592931898E-19, -0.9999939076577903929, -0.003490651415223739937 ) ) ;
#72778 = CARTESIAN_POINT ( 'NONE',  ( 3.149999999999944400, 2.500000000000000000, 1.718653347947321386 ) ) ;
#72779 = ADVANCED_FACE ( 'NONE', ( #23999 ), #54765, .T. ) ;
#72780 = EDGE_CURVE ( 'NONE', #97332, #85814, #25936, .T. ) ;
#72781 = DIRECTION ( 'NONE',  ( 0.000000000000000000, 0.000000000000000000, 1.000000000000000000 ) ) ;
#72782 = CARTESIAN_POINT ( 'NONE',  ( 13.74999999999989697, 2.500000000000000000, 2.857883832488649301 ) ) ;
#72783 = EDGE_CURVE ( 'NONE', #22216, #95241, #84191, .T. ) ;
#72784 = ADVANCED_FACE ( 'NONE', ( #24641 ), #64556, .T. ) ;
#72785 = CIRCLE ( 'NONE', #114624, 0.1000000000000000472 ) ;
#72786 = ORIENTED_EDGE ( 'NONE', *, *, #2076, .T. ) ;
#72787 = ORIENTED_EDGE ( 'NONE', *, *, #31848, .T. ) ;
#72788 = DIRECTION ( 'NONE',  ( 0.000000000000000000, 1.000000000000000000, 0.000000000000000000 ) ) ;
#72789 = EDGE_CURVE ( 'NONE', #99291, #52298, #90262, .T. ) ;
#72790 = EDGE_LOOP ( 'NONE', ( #36330, #75628, #62471, #120712 ) ) ;
#72791 = DIRECTION ( 'NONE',  ( -0.000000000000000000, 1.000000000000000000, -0.000000000000000000 ) ) ;
#72792 = CARTESIAN_POINT ( 'NONE',  ( -11.44999999999999751, 12.50000000000000000, -2.511473670974873951 ) ) ;
#72793 = AXIS2_PLACEMENT_3D ( 'NONE', #44698, #115335, #116002 ) ;
#72794 = CARTESIAN_POINT ( 'NONE',  ( 5.649999999999934630, 2.500000000000000000, 6.148780366869520897 ) ) ;
#72796 = ORIENTED_EDGE ( 'NONE', *, *, #24449, .F. ) ;
#72795 = VERTEX_POINT ( 'NONE', #108975 ) ;
#72797 = FACE_BOUND ( 'NONE', #10894, .T. ) ;
#72798 = VERTEX_POINT ( 'NONE', #89366 ) ;
#72799 = CARTESIAN_POINT ( 'NONE',  ( -9.200000000000006395, 2.500000000000000000, 0.09999999999999761857 ) ) ;
#72800 = CARTESIAN_POINT ( 'NONE',  ( 21.23528140090950345, -2.699413673072312392, 2.293764360948889802 ) ) ;
#72801 = EDGE_CURVE ( 'NONE', #118526, #14213, #57325, .T. ) ;
#72802 = CARTESIAN_POINT ( 'NONE',  ( 1.249999999999988454, 2.500000000000000000, -2.165063509461101710 ) ) ;
#72803 = VECTOR ( 'NONE', #77202, 1000.000000000000000 ) ;
#72804 = DIRECTION ( 'NONE',  ( -0.000000000000000000, -1.000000000000000000, -0.000000000000000000 ) ) ;
#72805 = DIRECTION ( 'NONE',  ( 0.000000000000000000, 0.000000000000000000, -1.000000000000000000 ) ) ;
#72806 = FACE_OUTER_BOUND ( 'NONE', #19918, .T. ) ;
#72807 = CARTESIAN_POINT ( 'NONE',  ( 1.849999999999949685, 2.500000000000000000, 1.718653347947321386 ) ) ;
#72808 = DIRECTION ( 'NONE',  ( 0.000000000000000000, 0.000000000000000000, 1.000000000000000000 ) ) ;
#72809 = PLANE ( 'NONE',  #53742 ) ;
#72810 = CARTESIAN_POINT ( 'NONE',  ( 11.44999999999990692, 2.500000000000000000, -6.741600689897078169 ) ) ;
#72811 = AXIS2_PLACEMENT_3D ( 'NONE', #18565, #106300, #127870 ) ;
#72812 = AXIS2_PLACEMENT_3D ( 'NONE', #75234, #74595, #126279 ) ;
#72813 = DIRECTION ( 'NONE',  ( -0.000000000000000000, 1.000000000000000000, -0.000000000000000000 ) ) ;
#72814 = ORIENTED_EDGE ( 'NONE', *, *, #29296, .F. ) ;
#72816 = ORIENTED_EDGE ( 'NONE', *, *, #33937, .F. ) ;
#72815 = AXIS2_PLACEMENT_3D ( 'NONE', #42653, #90416, #52440 ) ;
#72817 = ORIENTED_EDGE ( 'NONE', *, *, #2875, .T. ) ;
#72818 = DIRECTION ( 'NONE',  ( -0.000000000000000000, -1.000000000000000000, -0.000000000000000000 ) ) ;
#72819 = VERTEX_POINT ( 'NONE', #118170 ) ;
#72820 = FACE_OUTER_BOUND ( 'NONE', #122465, .T. ) ;
#72822 = ORIENTED_EDGE ( 'NONE', *, *, #35216, .T. ) ;
#72821 = VERTEX_POINT ( 'NONE', #128674 ) ;
#72823 = VERTEX_POINT ( 'NONE', #126714 ) ;
#72824 = DIRECTION ( 'NONE',  ( 0.000000000000000000, 0.000000000000000000, 1.000000000000000000 ) ) ;
#72825 = CARTESIAN_POINT ( 'NONE',  ( 3.099999999999945466, 12.50000000000000000, -3.918623584224389056 ) ) ;
#72826 = DIRECTION ( 'NONE',  ( 0.000000000000000000, 0.000000000000000000, -1.000000000000000000 ) ) ;
#72827 = DIRECTION ( 'NONE',  ( 0.000000000000000000, 1.000000000000000000, 0.000000000000000000 ) ) ;
#72828 = FACE_OUTER_BOUND ( 'NONE', #52271, .T. ) ;
#72829 = CONICAL_SURFACE ( 'NONE', #68603, 0.09999999999999982514, 0.003490658503988666988 ) ;
#72830 = VERTEX_POINT ( 'NONE', #76963 ) ;
#72831 = DIRECTION ( 'NONE',  ( -0.000000000000000000, -1.000000000000000000, -0.000000000000000000 ) ) ;
#72832 = ORIENTED_EDGE ( 'NONE', *, *, #129092, .F. ) ;
#72834 = AXIS2_PLACEMENT_3D ( 'NONE', #108782, #39443, #115 ) ;
#72833 = CIRCLE ( 'NONE', #7970, 0.1000000000000000472 ) ;
#72835 = ORIENTED_EDGE ( 'NONE', *, *, #55612, .T. ) ;
#72836 = EDGE_CURVE ( 'NONE', #84933, #120640, #48153, .T. ) ;
#72837 = VERTEX_POINT ( 'NONE', #47511 ) ;
#72838 = LINE ( 'NONE', #30353, #65169 ) ;
#72839 = ORIENTED_EDGE ( 'NONE', *, *, #63030, .F. ) ;
#72840 = VERTEX_POINT ( 'NONE', #127994 ) ;
#72841 = ORIENTED_EDGE ( 'NONE', *, *, #65368, .F. ) ;
#72842 = EDGE_CURVE ( 'NONE', #109254, #127530, #17374, .T. ) ;
#72843 = CARTESIAN_POINT ( 'NONE',  ( 10.39999999999990976, 2.500000000000000000, 4.330127018922196314 ) ) ;
#72844 = CARTESIAN_POINT ( 'NONE',  ( 4.399999999999937295, 12.50000000000000000, 4.676537180435972552 ) ) ;
#72845 = CARTESIAN_POINT ( 'NONE',  ( -5.450000000000019718, 2.500000000000000000, 2.065063509461097624 ) ) ;
#72847 = VECTOR ( 'NONE', #72622, 1000.000000000000000 ) ;
#72846 = CARTESIAN_POINT ( 'NONE',  ( -8.749999999999975131, 2.500000000000000000, 2.165063509461097713 ) ) ;
#72848 = CARTESIAN_POINT ( 'NONE',  ( 3.549999999999942091, 12.50000000000000000, 2.511473670974873507 ) ) ;
#72849 = EDGE_LOOP ( 'NONE', ( #121210, #30687 ) ) ;
#72851 = CARTESIAN_POINT ( 'NONE',  ( -2.500000000000031086, 2.500000000000000000, 3.737306695894644371 ) ) ;
#72850 = AXIS2_PLACEMENT_3D ( 'NONE', #23609, #13124, #93009 ) ;
#72853 = ORIENTED_EDGE ( 'NONE', *, *, #9069, .T. ) ;
#72852 = AXIS2_PLACEMENT_3D ( 'NONE', #87956, #117410, #76879 ) ;
#72854 = CARTESIAN_POINT ( 'NONE',  ( 184.9583333333332860, 4.445597072760175905, 7.699999999999896261 ) ) ;
#72855 = AXIS2_PLACEMENT_3D ( 'NONE', #54160, #76378, #24699 ) ;
#72856 = ORIENTED_EDGE ( 'NONE', *, *, #88298, .T. ) ;
#72857 = DIRECTION ( 'NONE',  ( -0.000000000000000000, -1.000000000000000000, -0.000000000000000000 ) ) ;
#72858 = VERTEX_POINT ( 'NONE', #107712 ) ;
#72859 = VECTOR ( 'NONE', #42233, 1000.000000000000000 ) ;
#72860 = CARTESIAN_POINT ( 'NONE',  ( 184.3593750003413732, 0.000000000000000000, 7.564683531250000925 ) ) ;
#72861 = CIRCLE ( 'NONE', #62409, 0.1000000000000000472 ) ;
#72862 = VECTOR ( 'NONE', #64189, 1000.000000000000000 ) ;
#72863 = CARTESIAN_POINT ( 'NONE',  ( -1.650000000000034328, 2.500000000000000000, -2.265063509461101798 ) ) ;
#72864 = ORIENTED_EDGE ( 'NONE', *, *, #125426, .T. ) ;
#72865 = EDGE_LOOP ( 'NONE', ( #41957, #118660, #48325, #58623 ) ) ;
#72866 = CARTESIAN_POINT ( 'NONE',  ( -4.999999999999986677, 2.500000000000000000, 4.430127018922196847 ) ) ;
#72867 = CARTESIAN_POINT ( 'NONE',  ( 11.44999999999990870, 2.500000000000000000, 6.841600689897072485 ) ) ;
#72868 = CARTESIAN_POINT ( 'NONE',  ( 6.449999999999930012, 2.500000000000000000, 6.841600689897072485 ) ) ;
#72869 = LINE ( 'NONE', #80765, #22157 ) ;
#72870 = CIRCLE ( 'NONE', #87517, 0.09999999999999982514 ) ;
#72871 = DIRECTION ( 'NONE',  ( 0.000000000000000000, 0.000000000000000000, 1.000000000000000000 ) ) ;
#72872 = ADVANCED_FACE ( 'NONE', ( #97241 ), #9513, .T. ) ;
#72873 = ORIENTED_EDGE ( 'NONE', *, *, #19730, .F. ) ;
#72874 = CARTESIAN_POINT ( 'NONE',  ( 2.500000000000001776, -2.021986658763282207, 9.892226903609813604 ) ) ;
#72875 = VERTEX_POINT ( 'NONE', #37047 ) ;
#72876 = DIRECTION ( 'NONE',  ( 0.000000000000000000, -0.000000000000000000, 1.000000000000000000 ) ) ;
#72879 = EDGE_CURVE ( 'NONE', #53654, #66522, #71498, .T. ) ;
#72878 = VECTOR ( 'NONE', #50918, 1000.000000000000000 ) ;
#72877 = DIRECTION ( 'NONE',  ( -0.000000000000000000, -1.000000000000000000, -0.000000000000000000 ) ) ;
#72880 = VECTOR ( 'NONE', #39504, 1000.000000000000000 ) ;
#72881 = AXIS2_PLACEMENT_3D ( 'NONE', #44366, #71398, #4413 ) ;
#72882 = EDGE_CURVE ( 'NONE', #126113, #78182, #63090, .T. ) ;
#72883 = ADVANCED_FACE ( 'NONE', ( #118818 ), #69337, .T. ) ;
#72884 = CARTESIAN_POINT ( 'NONE',  ( 185.0468750003414016, -8.734944146203032389, -1.604583208406768146E-15 ) ) ;
#72885 = DIRECTION ( 'NONE',  ( 0.000000000000000000, -0.000000000000000000, 1.000000000000000000 ) ) ;
#72886 = DIRECTION ( 'NONE',  ( -4.274815082592931898E-19, -0.9999939076577903929, -0.003490651415223739937 ) ) ;
#72887 = DIRECTION ( 'NONE',  ( 0.000000000000000000, 0.000000000000000000, -1.000000000000000000 ) ) ;
#72888 = ADVANCED_FACE ( 'NONE', ( #39646 ), #88105, .T. ) ;
#72889 = DIRECTION ( 'NONE',  ( 0.000000000000000000, 0.000000000000000000, 1.000000000000000000 ) ) ;
#72890 = VERTEX_POINT ( 'NONE', #8209 ) ;
#72891 = VECTOR ( 'NONE', #123550, 1000.000000000000000 ) ;
#72892 = DIRECTION ( 'NONE',  ( 0.000000000000000000, 0.000000000000000000, 1.000000000000000000 ) ) ;
#72893 = CARTESIAN_POINT ( 'NONE',  ( -3.350000000000032507, 2.500000000000000000, -6.395190528383301931 ) ) ;
#72894 = FACE_OUTER_BOUND ( 'NONE', #50742, .T. ) ;
#72895 = EDGE_CURVE ( 'NONE', #100735, #106700, #44308, .T. ) ;
#72896 = VERTEX_POINT ( 'NONE', #29169 ) ;
#72897 = EDGE_CURVE ( 'NONE', #37017, #97094, #31805, .T. ) ;
#72898 = CIRCLE ( 'NONE', #118954, 0.06509327318403745899 ) ;
#72899 = CARTESIAN_POINT ( 'NONE',  ( -15.19999999999998330, 12.50000000000000000, 0.3464101615137758494 ) ) ;
#72900 = CIRCLE ( 'NONE', #70837, 0.1000000000000000472 ) ;
#72901 = EDGE_LOOP ( 'NONE', ( #11745, #21854, #90088, #38225 ) ) ;
#72902 = ORIENTED_EDGE ( 'NONE', *, *, #120891, .F. ) ;
#72903 = CARTESIAN_POINT ( 'NONE',  ( -9.350000000000006750, 2.500000000000000000, 1.918653347947321564 ) ) ;
#72904 = VERTEX_POINT ( 'NONE', #49459 ) ;
#72905 = CARTESIAN_POINT ( 'NONE',  ( 16.53754090006383848, -0.4856821978172663479, -6.114873053049103113 ) ) ;
#72906 = CARTESIAN_POINT ( 'NONE',  ( 0.8499999999999536815, 2.500000000000000000, 6.495190528383297135 ) ) ;
#72907 = DIRECTION ( 'NONE',  ( 0.000000000000000000, 0.000000000000000000, -1.000000000000000000 ) ) ;
#72908 = EDGE_LOOP ( 'NONE', ( #35578, #93674 ) ) ;
#72909 = CARTESIAN_POINT ( 'NONE',  ( -9.350000000000006750, 12.50000000000000000, 1.818653347947321475 ) ) ;
#72911 = VECTOR ( 'NONE', #12999, 1000.000000000000000 ) ;
#72910 = CIRCLE ( 'NONE', #118964, 0.06509327318403745899 ) ;
#72912 = DIRECTION ( 'NONE',  ( 0.000000000000000000, 0.000000000000000000, 1.000000000000000000 ) ) ;
#72913 = AXIS2_PLACEMENT_3D ( 'NONE', #125421, #53472, #55395 ) ;
#72914 = ORIENTED_EDGE ( 'NONE', *, *, #20282, .F. ) ;
#72915 = AXIS2_PLACEMENT_3D ( 'NONE', #91528, #20851, #1206 ) ;
#72916 = ORIENTED_EDGE ( 'NONE', *, *, #42899, .F. ) ;
#72917 = ORIENTED_EDGE ( 'NONE', *, *, #76130, .F. ) ;
#72918 = DIRECTION ( 'NONE',  ( 0.000000000000000000, 0.000000000000000000, 1.000000000000000000 ) ) ;
#72919 = DIRECTION ( 'NONE',  ( 0.000000000000000000, -0.000000000000000000, 1.000000000000000000 ) ) ;
#72920 = DIRECTION ( 'NONE',  ( -0.000000000000000000, -1.000000000000000000, -0.000000000000000000 ) ) ;
#72921 = ORIENTED_EDGE ( 'NONE', *, *, #60258, .F. ) ;
#72922 = DIRECTION ( 'NONE',  ( 0.000000000000000000, 1.000000000000000000, 0.000000000000000000 ) ) ;
#72923 = CARTESIAN_POINT ( 'NONE',  ( 6.449999999999931788, 2.500000000000000000, -2.511473670974877948 ) ) ;
#72924 = ORIENTED_EDGE ( 'NONE', *, *, #19368, .T. ) ;
#72925 = DIRECTION ( 'NONE',  ( 0.000000000000000000, 1.000000000000000000, 0.000000000000000000 ) ) ;
#72926 = DIRECTION ( 'NONE',  ( 0.000000000000000000, -0.000000000000000000, 1.000000000000000000 ) ) ;
#72928 = ADVANCED_FACE ( 'NONE', ( #18029 ), #81860, .T. ) ;
#72927 = DIRECTION ( 'NONE',  ( 1.000000000000000000, -0.000000000000000000, -0.000000000000000000 ) ) ;
#72929 = CARTESIAN_POINT ( 'NONE',  ( 3.749999999999942268, 2.500000000000000000, 1.472243186433545459 ) ) ;
#72930 = CIRCLE ( 'NONE', #98056, 5.200000000000000178 ) ;
#72931 = DIRECTION ( 'NONE',  ( 0.000000000000000000, 0.000000000000000000, 1.000000000000000000 ) ) ;
#72932 = EDGE_CURVE ( 'NONE', #58787, #90838, #27860, .T. ) ;
#72933 = CARTESIAN_POINT ( 'NONE',  ( -8.350000000000013856, 12.50000000000000000, -5.737276932171707422 ) ) ;
#72934 = LINE ( 'NONE', #23179, #8565 ) ;
#72935 = ADVANCED_FACE ( 'NONE', ( #119448 ), #29797, .T. ) ;
#72936 = ADVANCED_FACE ( 'NONE', ( #107051 ), #13996, .T. ) ;
#72937 = CIRCLE ( 'NONE', #45753, 0.09999999999999982514 ) ;
#72938 = VECTOR ( 'NONE', #96182, 1000.000000000000000 ) ;
#72939 = ORIENTED_EDGE ( 'NONE', *, *, #6399, .T. ) ;
#72940 = EDGE_LOOP ( 'NONE', ( #105577, #18082, #59233, #3980 ) ) ;
#72942 = ORIENTED_EDGE ( 'NONE', *, *, #101211, .T. ) ;
#72941 = EDGE_CURVE ( 'NONE', #129288, #27568, #50103, .T. ) ;
#72943 = EDGE_LOOP ( 'NONE', ( #30898, #31343 ) ) ;
#72944 = CARTESIAN_POINT ( 'NONE',  ( 0.5999999999999612310, 12.50000000000000000, -0.2813168883297386680 ) ) ;
#72945 = CARTESIAN_POINT ( 'NONE',  ( 9.999999999999952038, 2.500000000000000000, -2.276824562219559311E-15 ) ) ;
#72946 = CARTESIAN_POINT ( 'NONE',  ( 165.4999999999999716, 0.000000000000000000, 2.000000000000000000 ) ) ;
#72947 = VERTEX_POINT ( 'NONE', #120114 ) ;
#72948 = FACE_BOUND ( 'NONE', #118074, .T. ) ;
#72949 = FACE_OUTER_BOUND ( 'NONE', #20726, .T. ) ;
#72950 = CARTESIAN_POINT ( 'NONE',  ( 3.749999999999976907, 12.50000000000000000, 2.099970236277060032 ) ) ;
#72951 = AXIS2_PLACEMENT_3D ( 'NONE', #70297, #29718, #48730 ) ;
#72953 = ADVANCED_FACE ( 'NONE', ( #122684 ), #61191, .T. ) ;
#72952 = AXIS2_PLACEMENT_3D ( 'NONE', #20843, #32627, #9732 ) ;
#72954 = CARTESIAN_POINT ( 'NONE',  ( 1.049999999999952083, 2.500000000000000000, 6.841600689897072485 ) ) ;
#72955 = CIRCLE ( 'NONE', #123125, 0.06509327318403745899 ) ;
#72956 = EDGE_CURVE ( 'NONE', #109646, #98794, #34967, .T. ) ;
#72957 = DIRECTION ( 'NONE',  ( 0.000000000000000000, 1.000000000000000000, 0.000000000000000000 ) ) ;
#72958 = LINE ( 'NONE', #32416, #30469 ) ;
#72959 = DIRECTION ( 'NONE',  ( -0.000000000000000000, 1.000000000000000000, -0.000000000000000000 ) ) ;
#72960 = CARTESIAN_POINT ( 'NONE',  ( -11.04999999999999893, 12.50000000000000000, 1.818653347947321475 ) ) ;
#72961 = CARTESIAN_POINT ( 'NONE',  ( -15.19999999999998153, 2.500000000000000000, -0.2464101615137759549 ) ) ;
#72962 = CARTESIAN_POINT ( 'NONE',  ( 139.9358549477330200, 0.5000000000000000000, -3.576063159858998475 ) ) ;
#72963 = ORIENTED_EDGE ( 'NONE', *, *, #6556, .F. ) ;
#72964 = AXIS2_PLACEMENT_3D ( 'NONE', #64656, #97817, #24095 ) ;
#72965 = EDGE_LOOP ( 'NONE', ( #110266, #8648 ) ) ;
#72966 = EDGE_LOOP ( 'NONE', ( #3208, #49539, #82018, #100304 ) ) ;
#72967 = ORIENTED_EDGE ( 'NONE', *, *, #23869, .T. ) ;
#72968 = ORIENTED_EDGE ( 'NONE', *, *, #29847, .F. ) ;
#72969 = ORIENTED_EDGE ( 'NONE', *, *, #51175, .F. ) ;
#72970 = DIRECTION ( 'NONE',  ( 0.000000000000000000, 1.000000000000000000, 0.000000000000000000 ) ) ;
#72971 = EDGE_LOOP ( 'NONE', ( #64507, #560 ) ) ;
#72972 = VERTEX_POINT ( 'NONE', #121390 ) ;
#72973 = AXIS2_PLACEMENT_3D ( 'NONE', #59575, #49740, #129598 ) ;
#72974 = DIRECTION ( 'NONE',  ( 0.000000000000000000, 0.000000000000000000, -1.000000000000000000 ) ) ;
#72975 = DIRECTION ( 'NONE',  ( -1.000000000000000000, -0.000000000000000000, -0.000000000000000000 ) ) ;
#72976 = CARTESIAN_POINT ( 'NONE',  ( -3.100000000000028511, 2.500000000000000000, 0.2464101615137736789 ) ) ;
#72977 = CIRCLE ( 'NONE', #43752, 0.09999999999999982514 ) ;
#72978 = VERTEX_POINT ( 'NONE', #101763 ) ;
#72979 = DIRECTION ( 'NONE',  ( 0.000000000000000000, 0.000000000000000000, 1.000000000000000000 ) ) ;
#72980 = ORIENTED_EDGE ( 'NONE', *, *, #41005, .F. ) ;
#72981 = ORIENTED_EDGE ( 'NONE', *, *, #55506, .T. ) ;
#72982 = CIRCLE ( 'NONE', #95961, 0.1000000000000002554 ) ;
#72983 = CARTESIAN_POINT ( 'NONE',  ( -7.700000000000014388, 2.500000000000000000, -0.2464101615137782308 ) ) ;
#72984 = CARTESIAN_POINT ( 'NONE',  ( -5.650000000000023448, 12.50000000000000000, -1.818653347947326138 ) ) ;
#72985 = VERTEX_POINT ( 'NONE', #72944 ) ;
#72986 = AXIS2_PLACEMENT_3D ( 'NONE', #36796, #25662, #126459 ) ;
#72987 = UNCERTAINTY_MEASURE_WITH_UNIT (LENGTH_MEASURE( 1.000000000000000082E-05 ), #16004, 'distance_accuracy_value', 'NONE');
#72988 = EDGE_LOOP ( 'NONE', ( #104804, #38381 ) ) ;
#72989 = CARTESIAN_POINT ( 'NONE',  ( 11.89999999999990443, 2.500000000000000000, 0.3464101615137736845 ) ) ;
#72990 = CIRCLE ( 'NONE', #89159, 0.09999999999999982514 ) ;
#72991 = EDGE_CURVE ( 'NONE', #16954, #51911, #87165, .T. ) ;
#72992 = CARTESIAN_POINT ( 'NONE',  ( -4.350000000000023626, 2.500000000000000000, 2.511473670974873507 ) ) ;
#72993 = DIRECTION ( 'NONE',  ( -1.000000000000000000, 0.000000000000000000, -0.000000000000000000 ) ) ;
#72994 = LINE ( 'NONE', #91340, #37769 ) ;
#72995 = DIRECTION ( 'NONE',  ( 0.000000000000000000, -0.9999939076577903929, 0.003490651415223739937 ) ) ;
#72996 = CIRCLE ( 'NONE', #24880, 0.06509327318403745899 ) ;
#72997 = ORIENTED_EDGE ( 'NONE', *, *, #20746, .F. ) ;
#72998 = CARTESIAN_POINT ( 'NONE',  ( 14.18215599311760755, -2.499999999999999112, 6.639800458426547536 ) ) ;
#72999 = ORIENTED_EDGE ( 'NONE', *, *, #61610, .F. ) ;
#73000 = CARTESIAN_POINT ( 'NONE',  ( 1.449999999999952216, 2.500000000000000000, 1.818653347947321475 ) ) ;
#73002 = AXIS2_PLACEMENT_3D ( 'NONE', #13655, #14919, #112528 ) ;
#73001 = AXIS2_PLACEMENT_3D ( 'NONE', #29891, #92028, #91382 ) ;
#73003 = ORIENTED_EDGE ( 'NONE', *, *, #85771, .T. ) ;
#73004 = CARTESIAN_POINT ( 'NONE',  ( 6.449999999999928235, 12.50000000000000000, 2.576566944158910744 ) ) ;
#73005 = CARTESIAN_POINT ( 'NONE',  ( -8.950000000000011724, 2.500000000000000000, -6.248780366869521430 ) ) ;
#73006 = CONICAL_SURFACE ( 'NONE', #106450, 0.1000000000000002554, 0.003490658503988666988 ) ;
#73007 = DIRECTION ( 'NONE',  ( 0.000000000000000000, -0.9999939076577903929, 0.003490651415223739937 ) ) ;
#73008 = CARTESIAN_POINT ( 'NONE',  ( -5.800000000000022027, 2.500000000000000000, -4.430127018922202176 ) ) ;
#73009 = ORIENTED_EDGE ( 'NONE', *, *, #81802, .T. ) ;
#73010 = CARTESIAN_POINT ( 'NONE',  ( 187.0312500006828031, 9.429780353434619030E-16, -7.700000000000000178 ) ) ;
#73012 = CIRCLE ( 'NONE', #47892, 0.06509327318403745899 ) ;
#73011 = AXIS2_PLACEMENT_3D ( 'NONE', #126789, #107787, #17452 ) ;
#73013 = CARTESIAN_POINT ( 'NONE',  ( -14.99999999999998224, 12.50000000000000000, -0.6928203230275519209 ) ) ;
#73014 = ORIENTED_EDGE ( 'NONE', *, *, #69191, .F. ) ;
#73015 = VERTEX_POINT ( 'NONE', #50722 ) ;
#73016 = EDGE_LOOP ( 'NONE', ( #68597, #79584, #66065, #14461 ) ) ;
#73017 = LINE ( 'NONE', #71081, #14377 ) ;
#73018 = CARTESIAN_POINT ( 'NONE',  ( -1.050000000000038236, 12.50000000000000000, -1.818653347947326138 ) ) ;
#73019 = CARTESIAN_POINT ( 'NONE',  ( 185.7343750003414016, 8.734944146203032389, 5.348610694689227483E-16 ) ) ;
#73020 = LINE ( 'NONE', #32484, #13523 ) ;
#73021 = CARTESIAN_POINT ( 'NONE',  ( -11.84999999999999609, 2.500000000000000000, 6.148780366869520897 ) ) ;
#73022 = DIRECTION ( 'NONE',  ( -0.000000000000000000, -1.000000000000000000, -0.000000000000000000 ) ) ;
#73023 = CARTESIAN_POINT ( 'NONE',  ( -2.900000000000029665, 2.500000000000000000, 3.737306695894644371 ) ) ;
#73024 = AXIS2_PLACEMENT_3D ( 'NONE', #45429, #16577, #125267 ) ;
#73025 = DIRECTION ( 'NONE',  ( -0.000000000000000000, -1.000000000000000000, -0.000000000000000000 ) ) ;
#73026 = AXIS2_PLACEMENT_3D ( 'NONE', #81103, #43126, #31360 ) ;
#73027 = ADVANCED_FACE ( 'NONE', ( #20629 ), #72524, .T. ) ;
#73028 = CIRCLE ( 'NONE', #79309, 0.06509327318403745899 ) ;
#73029 = ORIENTED_EDGE ( 'NONE', *, *, #119334, .T. ) ;
#73030 = CARTESIAN_POINT ( 'NONE',  ( -8.950000000000006395, 12.50000000000000000, 6.841600689897072485 ) ) ;
#73031 = EDGE_CURVE ( 'NONE', #118702, #3798, #1610, .T. ) ;
#73032 = FACE_OUTER_BOUND ( 'NONE', #70403, .T. ) ;
#73033 = CARTESIAN_POINT ( 'NONE',  ( 129.5000000000000000, 0.9999999999999985567, -7.634788798650556707 ) ) ;
#73034 = CARTESIAN_POINT ( 'NONE',  ( -6.850000000000013856, 12.50000000000000000, 6.841600689897072485 ) ) ;
#73035 = EDGE_CURVE ( 'NONE', #73360, #125465, #33038, .T. ) ;
#73036 = CIRCLE ( 'NONE', #20807, 0.1000000000000000472 ) ;
#73037 = ORIENTED_EDGE ( 'NONE', *, *, #57838, .T. ) ;
#73038 = AXIS2_PLACEMENT_3D ( 'NONE', #25332, #113077, #123536 ) ;
#73039 = DIRECTION ( 'NONE',  ( 0.000000000000000000, 0.000000000000000000, 1.000000000000000000 ) ) ;
#73040 = AXIS2_PLACEMENT_3D ( 'NONE', #69424, #127707, #87771 ) ;
#73041 = FACE_OUTER_BOUND ( 'NONE', #68570, .T. ) ;
#73043 = ORIENTED_EDGE ( 'NONE', *, *, #17935, .F. ) ;
#73042 = CARTESIAN_POINT ( 'NONE',  ( 5.849999999999934808, 12.50000000000000000, -5.802370205355749988 ) ) ;
#73044 = EDGE_CURVE ( 'NONE', #1197, #82804, #82116, .T. ) ;
#73045 = EDGE_CURVE ( 'NONE', #35250, #103864, #122678, .T. ) ;
#73046 = ADVANCED_FACE ( 'NONE', ( #30462 ), #57941, .T. ) ;
#73047 = ADVANCED_FACE ( 'NONE', ( #32404 ), #62495, .T. ) ;
#73048 = ADVANCED_FACE ( 'NONE', ( #60568 ), #21922, .T. ) ;
#73049 = VECTOR ( 'NONE', #123303, 1000.000000000000000 ) ;
#73050 = VERTEX_POINT ( 'NONE', #112871 ) ;
#73051 = DIRECTION ( 'NONE',  ( -0.000000000000000000, 1.000000000000000000, -0.000000000000000000 ) ) ;
#73052 = CIRCLE ( 'NONE', #62596, 0.06509327318403745899 ) ;
#73053 = VECTOR ( 'NONE', #83993, 1000.000000000000000 ) ;
#73054 = VERTEX_POINT ( 'NONE', #80840 ) ;
#73055 = ORIENTED_EDGE ( 'NONE', *, *, #12475, .T. ) ;
#73056 = CARTESIAN_POINT ( 'NONE',  ( 12.89999999999989733, 2.500000000000000000, 0.09999999999999761857 ) ) ;
#73057 = EDGE_CURVE ( 'NONE', #101366, #113477, #32819, .T. ) ;
#73058 = EDGE_LOOP ( 'NONE', ( #98334, #107121, #85892, #31103 ) ) ;
#73059 = CARTESIAN_POINT ( 'NONE',  ( 18.20334136264111535, 2.532871263994777244, -4.817802756299775169 ) ) ;
#73060 = DIRECTION ( 'NONE',  ( 0.000000000000000000, 0.000000000000000000, 1.000000000000000000 ) ) ;
#73061 = CARTESIAN_POINT ( 'NONE',  ( -14.14999999999998614, 12.50000000000000000, 2.230156782645138946 ) ) ;
#73062 = VERTEX_POINT ( 'NONE', #10158 ) ;
#73063 = DIRECTION ( 'NONE',  ( 0.000000000000000000, 0.000000000000000000, 1.000000000000000000 ) ) ;
#73065 = ORIENTED_EDGE ( 'NONE', *, *, #119327, .T. ) ;
#73064 = CARTESIAN_POINT ( 'NONE',  ( 12.89999999999990266, 2.500000000000000000, -4.922947341949753586 ) ) ;
#73066 = AXIS2_PLACEMENT_3D ( 'NONE', #40137, #38882, #118685 ) ;
#73067 = CARTESIAN_POINT ( 'NONE',  ( 17.50000000000000000, 2.481874158964659571, 3.264437049506136557 ) ) ;
#73068 = DIRECTION ( 'NONE',  ( 0.000000000000000000, 0.000000000000000000, -1.000000000000000000 ) ) ;
#73069 = ORIENTED_EDGE ( 'NONE', *, *, #43528, .T. ) ;
#73070 = ORIENTED_EDGE ( 'NONE', *, *, #109900, .F. ) ;
#73071 = ORIENTED_EDGE ( 'NONE', *, *, #77663, .F. ) ;
#73072 = ORIENTED_EDGE ( 'NONE', *, *, #115489, .F. ) ;
#73073 = DIRECTION ( 'NONE',  ( 0.000000000000000000, 1.000000000000000000, 0.000000000000000000 ) ) ;
#73074 = CARTESIAN_POINT ( 'NONE',  ( 12.07106445339185363, 1.500000000000190070, 8.629160868130334450 ) ) ;
#73075 = DIRECTION ( 'NONE',  ( 0.000000000000000000, -0.000000000000000000, 1.000000000000000000 ) ) ;
#73076 = FACE_BOUND ( 'NONE', #79375, .T. ) ;
#73077 = ORIENTED_EDGE ( 'NONE', *, *, #1295, .F. ) ;
#73078 = CARTESIAN_POINT ( 'NONE',  ( 184.0729166673494603, 4.445597072760120838, -7.699999999999998401 ) ) ;
#73079 = DIRECTION ( 'NONE',  ( 0.000000000000000000, -0.9999939076577903929, 0.003490651415223739937 ) ) ;
#73080 = CARTESIAN_POINT ( 'NONE',  ( -13.09999999999999076, 12.50000000000000000, 3.918623584224383727 ) ) ;
#73081 = PLANE ( 'NONE',  #52702 ) ;
#73082 = LINE ( 'NONE', #92730, #126186 ) ;
#73083 = EDGE_CURVE ( 'NONE', #76681, #101262, #18205, .T. ) ;
#73084 = AXIS2_PLACEMENT_3D ( 'NONE', #48037, #38217, #26460 ) ;
#73085 = DIRECTION ( 'NONE',  ( 1.000000000000000000, 0.000000000000000000, 0.000000000000000000 ) ) ;
#73086 = EDGE_CURVE ( 'NONE', #98404, #79083, #31105, .T. ) ;
#73088 = CARTESIAN_POINT ( 'NONE',  ( 11.24999999999991118, 2.500000000000000000, 5.802370205355744659 ) ) ;
#73087 = B_SPLINE_CURVE_WITH_KNOTS ( 'NONE', 3,
 ( #8374, #107872, #71023, #20637 ),
 .UNSPECIFIED., .F., .F.,
 ( 4, 4 ),
 ( 0.002015733555955077569, 0.002984807578936017093 ),
 .UNSPECIFIED. ) ;
#73089 = EDGE_CURVE ( 'NONE', #51142, #2098, #64184, .T. ) ;
#73091 = CIRCLE ( 'NONE', #116894, 0.09999999999999982514 ) ;
#73090 = VECTOR ( 'NONE', #56740, 1000.000000000000000 ) ;
#73092 = ORIENTED_EDGE ( 'NONE', *, *, #97552, .T. ) ;
#73093 = EDGE_LOOP ( 'NONE', ( #30354, #98716, #90093, #10307 ) ) ;
#73094 = ORIENTED_EDGE ( 'NONE', *, *, #812, .T. ) ;
#73095 = ORIENTED_EDGE ( 'NONE', *, *, #90171, .T. ) ;
#73096 = ORIENTED_EDGE ( 'NONE', *, *, #3289, .T. ) ;
#73097 = DIRECTION ( 'NONE',  ( 0.000000000000000000, 1.846105847067148022E-16, -1.000000000000000000 ) ) ;
#73098 = AXIS2_PLACEMENT_3D ( 'NONE', #46071, #97098, #45430 ) ;
#73099 = LINE ( 'NONE', #72460, #21565 ) ;
#73101 = EDGE_CURVE ( 'NONE', #99888, #36155, #13686, .T. ) ;
#73100 = ORIENTED_EDGE ( 'NONE', *, *, #97600, .F. ) ;
#73102 = FACE_BOUND ( 'NONE', #71538, .T. ) ;
#73103 = FACE_OUTER_BOUND ( 'NONE', #65514, .T. ) ;
#73104 = ADVANCED_FACE ( 'NONE', ( #75502 ), #55242, .T. ) ;
#73105 = CIRCLE ( 'NONE', #110658, 0.1000000000000000472 ) ;
#73106 = EDGE_CURVE ( 'NONE', #34594, #2409, #73566, .T. ) ;
#73107 = EDGE_CURVE ( 'NONE', #29124, #1392, #3554, .T. ) ;
#73108 = EDGE_LOOP ( 'NONE', ( #42553, #6524 ) ) ;
#73109 = DIRECTION ( 'NONE',  ( 0.000000000000000000, 1.000000000000000000, 0.000000000000000000 ) ) ;
#73110 = DIRECTION ( 'NONE',  ( 0.000000000000000000, 0.000000000000000000, 1.000000000000000000 ) ) ;
#73111 = DIRECTION ( 'NONE',  ( -0.000000000000000000, 1.000000000000000000, -0.000000000000000000 ) ) ;
#73112 = ORIENTED_EDGE ( 'NONE', *, *, #6715, .T. ) ;
#73113 = CARTESIAN_POINT ( 'NONE',  ( -9.350000000000006750, 2.500000000000000000, -1.918653347947325782 ) ) ;
#73114 = EDGE_CURVE ( 'NONE', #70171, #110675, #9814, .T. ) ;
#73115 = ORIENTED_EDGE ( 'NONE', *, *, #29472, .F. ) ;
#73116 = ORIENTED_EDGE ( 'NONE', *, *, #21778, .F. ) ;
#73117 = VERTEX_POINT ( 'NONE', #125886 ) ;
#73118 = CARTESIAN_POINT ( 'NONE',  ( 21.23528140090950345, -2.699413673072312392, 2.293764360948889802 ) ) ;
#73119 = CARTESIAN_POINT ( 'NONE',  ( -12.49999999999999289, 12.50000000000000000, -5.022947341949751454 ) ) ;
#73120 = CARTESIAN_POINT ( 'NONE',  ( 9.149999999999920419, 2.500000000000000000, -7.188010851410854052 ) ) ;
#73121 = ORIENTED_EDGE ( 'NONE', *, *, #121573, .F. ) ;
#73122 = DIRECTION ( 'NONE',  ( 0.000000000000000000, -0.9999939076577903929, 0.003490651415223739937 ) ) ;
#73123 = CIRCLE ( 'NONE', #10502, 0.1000000000000002554 ) ;
#73124 = CARTESIAN_POINT ( 'NONE',  ( -10.65000000000000213, 2.500000000000000000, 2.611473670974873151 ) ) ;
#73125 = VECTOR ( 'NONE', #67187, 1000.000000000000000 ) ;
#73126 = CARTESIAN_POINT ( 'NONE',  ( 5.399999999999933742, 2.500000000000000000, -2.385244779468109755E-15 ) ) ;
#73127 = PLANE ( 'NONE',  #60115 ) ;
#73128 = EDGE_LOOP ( 'NONE', ( #97559, #99775, #100428, #116281 ) ) ;
#73129 = CARTESIAN_POINT ( 'NONE',  ( -3.750000000000029310, 2.500000000000000000, -7.288010851410854585 ) ) ;
#73130 = ADVANCED_FACE ( 'NONE', ( #14001 ), #35603, .T. ) ;
#73131 = VERTEX_POINT ( 'NONE', #114157 ) ;
#73132 = CARTESIAN_POINT ( 'NONE',  ( 142.3152275665817115, 2.500000000000000000, 1.374601720185641973 ) ) ;
#73134 = VECTOR ( 'NONE', #70734, 1000.000000000000000 ) ;
#73133 = VECTOR ( 'NONE', #93292, 1000.000000000000000 ) ;
#73135 = EDGE_LOOP ( 'NONE', ( #7841, #12955, #119069, #3187 ) ) ;
#73136 = ORIENTED_EDGE ( 'NONE', *, *, #80025, .F. ) ;
#73137 = CARTESIAN_POINT ( 'NONE',  ( 10.59999999999990905, 12.50000000000000000, -4.741630453620016006 ) ) ;
#73138 = DIRECTION ( 'NONE',  ( -0.000000000000000000, 1.000000000000000000, -0.000000000000000000 ) ) ;
#73139 = CARTESIAN_POINT ( 'NONE',  ( 3.749999999999978684, 2.500000000000000000, -6.495190528383302464 ) ) ;
#73140 = LINE ( 'NONE', #71197, #73828 ) ;
#73141 = CARTESIAN_POINT ( 'NONE',  ( -10.00000000000000355, 2.500000000000000000, 3.737306695894644371 ) ) ;
#73142 = CONICAL_SURFACE ( 'NONE', #16671, 0.1000000000000002554, 0.003490658503988666988 ) ;
#73143 = ORIENTED_EDGE ( 'NONE', *, *, #83244, .F. ) ;
#73144 = ORIENTED_EDGE ( 'NONE', *, *, #19233, .T. ) ;
#73145 = CIRCLE ( 'NONE', #108731, 0.09999999999999982514 ) ;
#73146 = DIRECTION ( 'NONE',  ( 0.000000000000000000, 0.000000000000000000, 1.000000000000000000 ) ) ;
#73147 = CIRCLE ( 'NONE', #56411, 0.06509327318403745899 ) ;
#73148 = EDGE_CURVE ( 'NONE', #103155, #15846, #68386, .T. ) ;
#73149 = DIRECTION ( 'NONE',  ( -0.000000000000000000, 1.000000000000000000, -0.000000000000000000 ) ) ;
#73150 = CARTESIAN_POINT ( 'NONE',  ( -15.39999999999998082, 2.500000000000000000, 0.6928203230275518099 ) ) ;
#73151 = EDGE_LOOP ( 'NONE', ( #105473, #115885, #19433, #77564 ) ) ;
#73152 = VERTEX_POINT ( 'NONE', #65691 ) ;
#73153 = VECTOR ( 'NONE', #108699, 1000.000000000000000 ) ;
#73154 = PLANE ( 'NONE',  #112566 ) ;
#73155 = AXIS2_PLACEMENT_3D ( 'NONE', #86408, #75947, #106694 ) ;
#73156 = EDGE_LOOP ( 'NONE', ( #24375, #30446 ) ) ;
#73157 = DIRECTION ( 'NONE',  ( -0.000000000000000000, -1.000000000000000000, -0.000000000000000000 ) ) ;
#73158 = CARTESIAN_POINT ( 'NONE',  ( 0.5999999999999560130, 12.50000000000000000, -3.983716857408426293 ) ) ;
#73159 = CARTESIAN_POINT ( 'NONE',  ( -5.850000000000022737, 2.500000000000000000, -2.165063509461101710 ) ) ;
#73160 = ORIENTED_EDGE ( 'NONE', *, *, #14807, .T. ) ;
#73161 = CARTESIAN_POINT ( 'NONE',  ( 13.34999999999989662, 12.50000000000000000, -2.165063509461101710 ) ) ;
#73162 = DIRECTION ( 'NONE',  ( 0.000000000000000000, 0.000000000000000000, -1.000000000000000000 ) ) ;
#73163 = DIRECTION ( 'NONE',  ( -0.000000000000000000, -1.000000000000000000, -0.000000000000000000 ) ) ;
#73164 = AXIS2_PLACEMENT_3D ( 'NONE', #64857, #15088, #55050 ) ;
#73165 = CARTESIAN_POINT ( 'NONE',  ( -10.20000000000000639, 2.500000000000000000, -3.883716857408422207 ) ) ;
#73166 = EDGE_CURVE ( 'NONE', #121191, #70149, #105629, .T. ) ;
#73167 = DIRECTION ( 'NONE',  ( 0.000000000000000000, 0.000000000000000000, 1.000000000000000000 ) ) ;
#73168 = EDGE_LOOP ( 'NONE', ( #118302, #106196 ) ) ;
#73169 = CARTESIAN_POINT ( 'NONE',  ( 5.849999999999933920, 2.500000000000000000, 6.495190528383297135 ) ) ;
#73170 = CARTESIAN_POINT ( 'NONE',  ( 24.00496409368203743, -0.9037364215739981388, 4.313973893096084034 ) ) ;
#73171 = ORIENTED_EDGE ( 'NONE', *, *, #38955, .F. ) ;
#73172 = EDGE_LOOP ( 'NONE', ( #112887, #73830 ) ) ;
#73173 = CARTESIAN_POINT ( 'NONE',  ( 186.7135416670080872, 4.367472073101518859, -7.564683531249999149 ) ) ;
#73174 = DIRECTION ( 'NONE',  ( 1.000000000000000000, 0.000000000000000000, 0.000000000000000000 ) ) ;
#73175 = DIRECTION ( 'NONE',  ( -0.000000000000000000, 1.000000000000000000, -0.000000000000000000 ) ) ;
#73176 = CARTESIAN_POINT ( 'NONE',  ( -7.900000000000014566, 12.50000000000000000, 0.6928203230275494784 ) ) ;
#73177 = DIRECTION ( 'NONE',  ( 0.000000000000000000, 1.000000000000000000, 0.000000000000000000 ) ) ;
#73178 = CARTESIAN_POINT ( 'NONE',  ( 10.84999999999991260, 2.500000000000000000, -1.472243186433550122 ) ) ;
#73179 = FACE_OUTER_BOUND ( 'NONE', #94522, .T. ) ;
#73180 = CARTESIAN_POINT ( 'NONE',  ( -8.350000000000012079, 12.50000000000000000, 1.472243186433545459 ) ) ;
#73181 = CARTESIAN_POINT ( 'NONE',  ( -1.650000000000035216, 12.50000000000000000, -5.802370205355749988 ) ) ;
#73182 = AXIS2_PLACEMENT_3D ( 'NONE', #13566, #52866, #103258 ) ;
#73183 = DIRECTION ( 'NONE',  ( 0.000000000000000000, 1.000000000000000000, 0.000000000000000000 ) ) ;
#73184 = VERTEX_POINT ( 'NONE', #24486 ) ;
#73185 = ORIENTED_EDGE ( 'NONE', *, *, #90047, .T. ) ;
#73186 = EDGE_CURVE ( 'NONE', #5233, #26170, #15283, .T. ) ;
#73188 = VECTOR ( 'NONE', #33177, 1000.000000000000000 ) ;
#73187 = AXIS2_PLACEMENT_3D ( 'NONE', #35064, #84128, #74968 ) ;
#73189 = EDGE_LOOP ( 'NONE', ( #127491, #3698 ) ) ;
#73190 = VERTEX_POINT ( 'NONE', #55867 ) ;
#73191 = DIRECTION ( 'NONE',  ( -0.000000000000000000, -1.000000000000000000, -0.000000000000000000 ) ) ;
#73192 = CARTESIAN_POINT ( 'NONE',  ( 3.299999999999942979, 12.50000000000000000, 4.330127018922196314 ) ) ;
#73193 = EDGE_CURVE ( 'NONE', #87106, #72591, #123331, .T. ) ;
#73196 = VERTEX_POINT ( 'NONE', #124620 ) ;
#73195 = VECTOR ( 'NONE', #29449, 1000.000000000000000 ) ;
#73194 = AXIS2_PLACEMENT_3D ( 'NONE', #114081, #24409, #4743 ) ;
#73197 = DIRECTION ( 'NONE',  ( 0.000000000000000000, -0.000000000000000000, 1.000000000000000000 ) ) ;
#73198 = DIRECTION ( 'NONE',  ( -0.000000000000000000, 1.000000000000000000, -0.000000000000000000 ) ) ;
#73200 = ORIENTED_EDGE ( 'NONE', *, *, #55614, .F. ) ;
#73199 = DIRECTION ( 'NONE',  ( 0.000000000000000000, 1.000000000000000000, 0.000000000000000000 ) ) ;
#73201 = EDGE_CURVE ( 'NONE', #60164, #115875, #7741, .T. ) ;
#73202 = EDGE_CURVE ( 'NONE', #48878, #102426, #94499, .T. ) ;
#73203 = ADVANCED_FACE ( 'NONE', ( #23851 ), #80927, .T. ) ;
#73204 = DIRECTION ( 'NONE',  ( -0.000000000000000000, 1.000000000000000000, -0.000000000000000000 ) ) ;
#73205 = ADVANCED_FACE ( 'NONE', ( #53948 ), #20276, .T. ) ;
#73206 = DIRECTION ( 'NONE',  ( 0.000000000000000000, 0.000000000000000000, 1.000000000000000000 ) ) ;
#73207 = ORIENTED_EDGE ( 'NONE', *, *, #9383, .T. ) ;
#73208 = ORIENTED_EDGE ( 'NONE', *, *, #35828, .T. ) ;
#73209 = EDGE_LOOP ( 'NONE', ( #29038, #83908 ) ) ;
#73210 = VERTEX_POINT ( 'NONE', #14639 ) ;
#73211 = CARTESIAN_POINT ( 'NONE',  ( -4.150000000000025224, 12.50000000000000000, 6.495190528383297135 ) ) ;
#73212 = ADVANCED_FACE ( 'NONE', ( #44782 ), #5584, .T. ) ;
#73213 = DIRECTION ( 'NONE',  ( -4.274815082592931898E-19, -0.9999939076577903929, -0.003490651415223739937 ) ) ;
#73214 = DIRECTION ( 'NONE',  ( 0.000000000000000000, 1.000000000000000000, 0.000000000000000000 ) ) ;
#73215 = ADVANCED_FACE ( 'NONE', ( #57815 ), #114359, .T. ) ;
#73216 = DIRECTION ( 'NONE',  ( 0.000000000000000000, 1.000000000000000000, 0.000000000000000000 ) ) ;
#73217 = CIRCLE ( 'NONE', #16749, 0.06509327318403745899 ) ;
#73219 = ORIENTED_EDGE ( 'NONE', *, *, #45290, .T. ) ;
#73218 = EDGE_CURVE ( 'NONE', #40642, #96734, #87891, .T. ) ;
#73220 = CIRCLE ( 'NONE', #8355, 0.1000000000000000472 ) ;
#73221 = DIRECTION ( 'NONE',  ( 0.000000000000000000, -0.000000000000000000, 1.000000000000000000 ) ) ;
#73222 = VERTEX_POINT ( 'NONE', #38172 ) ;
#73223 = CARTESIAN_POINT ( 'NONE',  ( -13.34999999999999076, 12.50000000000000000, 1.537336459617586915 ) ) ;
#73224 = CARTESIAN_POINT ( 'NONE',  ( 8.328334241102787416, -2.499999999999999556, -8.539519493615843615 ) ) ;
#73225 = FACE_OUTER_BOUND ( 'NONE', #29193, .T. ) ;
#73226 = DIRECTION ( 'NONE',  ( 0.000000000000000000, 1.000000000000000000, 0.000000000000000000 ) ) ;
#73227 = AXIS2_PLACEMENT_3D ( 'NONE', #105249, #45062, #73221 ) ;
#73228 = VERTEX_POINT ( 'NONE', #97728 ) ;
#73229 = ORIENTED_EDGE ( 'NONE', *, *, #118265, .T. ) ;
#73230 = VERTEX_POINT ( 'NONE', #17875 ) ;
#73231 = CARTESIAN_POINT ( 'NONE',  ( -10.40000000000000213, 2.500000000000000000, 5.022947341949748790 ) ) ;
#73232 = FACE_OUTER_BOUND ( 'NONE', #48311, .T. ) ;
#73233 = FACE_OUTER_BOUND ( 'NONE', #85737, .T. ) ;
#73234 = FACE_BOUND ( 'NONE', #43987, .T. ) ;
#73235 = CONICAL_SURFACE ( 'NONE', #29328, 0.1000000000000002554, 0.003490658503988666988 ) ;
#73236 = DIRECTION ( 'NONE',  ( -0.000000000000000000, 1.000000000000000000, -0.000000000000000000 ) ) ;
#73237 = CARTESIAN_POINT ( 'NONE',  ( 7.099999999999927702, 2.500000000000000000, 4.922947341949748257 ) ) ;
#73238 = DIRECTION ( 'NONE',  ( -0.000000000000000000, -1.000000000000000000, -0.000000000000000000 ) ) ;
#73239 = VECTOR ( 'NONE', #98147, 1000.000000000000000 ) ;
#73240 = DIRECTION ( 'NONE',  ( -0.000000000000000000, 1.000000000000000000, -0.000000000000000000 ) ) ;
#73241 = DIRECTION ( 'NONE',  ( 1.000000000000000000, 0.000000000000000000, 0.000000000000000000 ) ) ;
#73242 = CARTESIAN_POINT ( 'NONE',  ( -10.60000000000000320, 2.500000000000000000, -4.083716857408422385 ) ) ;
#73243 = ORIENTED_EDGE ( 'NONE', *, *, #85790, .F. ) ;
#73244 = CONICAL_SURFACE ( 'NONE', #123404, 0.09999999999999982514, 0.003490658503988666988 ) ;
#73245 = CARTESIAN_POINT ( 'NONE',  ( -11.44999999999999751, 2.500000000000000000, 2.511473670974873507 ) ) ;
#73246 = AXIS2_PLACEMENT_3D ( 'NONE', #75974, #16381, #23657 ) ;
#73247 = EDGE_LOOP ( 'NONE', ( #67608, #92526 ) ) ;
#73248 = EDGE_LOOP ( 'NONE', ( #71668, #27722 ) ) ;
#73249 = LINE ( 'NONE', #62797, #102943 ) ;
#73250 = EDGE_CURVE ( 'NONE', #26170, #75526, #68293, .T. ) ;
#73251 = FACE_BOUND ( 'NONE', #33083, .T. ) ;
#73252 = DIRECTION ( 'NONE',  ( -0.000000000000000000, 1.000000000000000000, -0.000000000000000000 ) ) ;
#73253 = ADVANCED_FACE ( 'NONE', ( #8054 ), #47352, .T. ) ;
#73254 = EDGE_CURVE ( 'NONE', #93836, #76693, #49538, .T. ) ;
#73255 = ORIENTED_EDGE ( 'NONE', *, *, #36602, .T. ) ;
#73256 = CARTESIAN_POINT ( 'NONE',  ( 43.06166283081541479, 3.066941195862745495, 4.904920240844576007 ) ) ;
#73257 = CARTESIAN_POINT ( 'NONE',  ( -13.94999999999998863, 2.500000000000000000, 2.611473670974877148 ) ) ;
#73258 = ORIENTED_EDGE ( 'NONE', *, *, #57622, .T. ) ;
#73259 = LINE ( 'NONE', #122373, #103361 ) ;
#73260 = CARTESIAN_POINT ( 'NONE',  ( 186.7812500006828031, 0.000000000000000000, 7.700000000000000178 ) ) ;
#73261 = EDGE_CURVE ( 'NONE', #7920, #111617, #45337, .T. ) ;
#73262 = AXIS2_PLACEMENT_3D ( 'NONE', #120167, #1031, #1664 ) ;
#73263 = VERTEX_POINT ( 'NONE', #48002 ) ;
#73264 = CARTESIAN_POINT ( 'NONE',  ( 12.49999999999990052, 12.50000000000000000, 0.6928203230275494784 ) ) ;
#73265 = CIRCLE ( 'NONE', #16804, 0.09999999999999982514 ) ;
#73266 = CARTESIAN_POINT ( 'NONE',  ( 3.949999999999941558, 2.500000000000000000, -1.818653347947326138 ) ) ;
#73267 = EDGE_LOOP ( 'NONE', ( #95694, #65719 ) ) ;
#73268 = CARTESIAN_POINT ( 'NONE',  ( -12.04999999999999716, 2.500000000000000000, -6.595190528383298556 ) ) ;
#73269 = DIRECTION ( 'NONE',  ( 0.000000000000000000, 0.000000000000000000, -1.000000000000000000 ) ) ;
#73270 = DIRECTION ( 'NONE',  ( 0.000000000000000000, 0.000000000000000000, 1.000000000000000000 ) ) ;
#73271 = EDGE_LOOP ( 'NONE', ( #59755, #61207, #77145, #88313 ) ) ;
#73272 = ORIENTED_EDGE ( 'NONE', *, *, #101864, .T. ) ;
#73273 = CARTESIAN_POINT ( 'NONE',  ( 5.849999999999933920, 2.500000000000000000, 5.802370205355744659 ) ) ;
#73274 = EDGE_CURVE ( 'NONE', #11966, #69989, #78792, .T. ) ;
#73275 = ORIENTED_EDGE ( 'NONE', *, *, #47028, .F. ) ;
#73276 = DIRECTION ( 'NONE',  ( 0.000000000000000000, 0.000000000000000000, -1.000000000000000000 ) ) ;
#73277 = DIRECTION ( 'NONE',  ( 0.000000000000000000, 0.000000000000000000, 1.000000000000000000 ) ) ;
#73278 = ORIENTED_EDGE ( 'NONE', *, *, #127278, .T. ) ;
#73279 = DIRECTION ( 'NONE',  ( -0.000000000000000000, 1.000000000000000000, -0.000000000000000000 ) ) ;
#73280 = LINE ( 'NONE', #63473, #79640 ) ;
#73281 = CARTESIAN_POINT ( 'NONE',  ( -3.150000000000029221, 2.500000000000000000, 2.411473670974873862 ) ) ;
#73282 = CARTESIAN_POINT ( 'NONE',  ( 11.84999999999990727, 12.50000000000000000, 6.841600689897072485 ) ) ;
#73283 = DIRECTION ( 'NONE',  ( 0.000000000000000000, 0.000000000000000000, 1.000000000000000000 ) ) ;
#73284 = ORIENTED_EDGE ( 'NONE', *, *, #104525, .F. ) ;
#73285 = ORIENTED_EDGE ( 'NONE', *, *, #98166, .T. ) ;
#73286 = CARTESIAN_POINT ( 'NONE',  ( 4.599999999999936584, 2.500000000000000000, 3.637306695894644726 ) ) ;
#73287 = EDGE_LOOP ( 'NONE', ( #9320, #125333, #109265, #123053 ) ) ;
#73288 = EDGE_CURVE ( 'NONE', #27754, #122264, #8682, .T. ) ;
#73289 = CARTESIAN_POINT ( 'NONE',  ( 103.0080513606563244, 7.694763653578461593, -0.3299518301331845205 ) ) ;
#73291 = ORIENTED_EDGE ( 'NONE', *, *, #35848, .T. ) ;
#73290 = ORIENTED_EDGE ( 'NONE', *, *, #109039, .T. ) ;
#73292 = ORIENTED_EDGE ( 'NONE', *, *, #121472, .T. ) ;
#73293 = CARTESIAN_POINT ( 'NONE',  ( 9.599999999999917932, 12.50000000000000000, -2.276824562219559311E-15 ) ) ;
#73294 = AXIS2_PLACEMENT_3D ( 'NONE', #105383, #123093, #24888 ) ;
#73295 = CARTESIAN_POINT ( 'NONE',  ( 6.849999999999930367, 2.500000000000000000, -6.941600689897078347 ) ) ;
#73296 = VECTOR ( 'NONE', #125472, 1000.000000000000000 ) ;
#73297 = CARTESIAN_POINT ( 'NONE',  ( 4.549999999999939426, 2.500000000000000000, -6.495190528383302464 ) ) ;
#73298 = DIRECTION ( 'NONE',  ( 0.000000000000000000, 0.000000000000000000, 1.000000000000000000 ) ) ;
#73299 = CARTESIAN_POINT ( 'NONE',  ( -1.900000000000034994, 12.50000000000000000, -4.676537180435978769 ) ) ;
#73300 = DIRECTION ( 'NONE',  ( 0.000000000000000000, 0.000000000000000000, 1.000000000000000000 ) ) ;
#73301 = FACE_OUTER_BOUND ( 'NONE', #77830, .T. ) ;
#73302 = DIRECTION ( 'NONE',  ( 0.000000000000000000, 1.000000000000000000, 0.000000000000000000 ) ) ;
#73303 = EDGE_CURVE ( 'NONE', #102426, #28344, #108180, .T. ) ;
#73304 = DIRECTION ( 'NONE',  ( 0.000000000000000000, 0.000000000000000000, -1.000000000000000000 ) ) ;
#73305 = ORIENTED_EDGE ( 'NONE', *, *, #39696, .T. ) ;
#73306 = DIRECTION ( 'NONE',  ( -0.000000000000000000, -1.000000000000000000, -0.000000000000000000 ) ) ;
#73307 = ORIENTED_EDGE ( 'NONE', *, *, #83449, .F. ) ;
#73308 = ADVANCED_FACE ( 'NONE', ( #106896 ), #64280, .T. ) ;
#73309 = ORIENTED_EDGE ( 'NONE', *, *, #103474, .F. ) ;
#73310 = CARTESIAN_POINT ( 'NONE',  ( -7.300000000000014921, 2.500000000000000000, 4.576537180435972019 ) ) ;
#73311 = FACE_OUTER_BOUND ( 'NONE', #25631, .T. ) ;
#73312 = CARTESIAN_POINT ( 'NONE',  ( 15.39999999999989022, 2.500000000000000000, -2.385244779468109755E-15 ) ) ;
#73313 = AXIS2_PLACEMENT_3D ( 'NONE', #109260, #87682, #79183 ) ;
#73314 = PLANE ( 'NONE',  #42012 ) ;
#73315 = CIRCLE ( 'NONE', #115151, 0.1000000000000002554 ) ;
#73317 = LINE ( 'NONE', #124371, #94641 ) ;
#73316 = PRODUCT_DEFINITION_SHAPE ( 'NONE', 'NONE',  #88428 ) ;
#73318 = DIRECTION ( 'NONE',  ( 0.000000000000000000, 1.000000000000000000, 0.000000000000000000 ) ) ;
#73319 = CARTESIAN_POINT ( 'NONE',  ( 6.899999999999928413, 12.50000000000000000, -4.611443907251939756 ) ) ;
#73320 = ORIENTED_EDGE ( 'NONE', *, *, #94585, .F. ) ;
#73321 = LINE ( 'NONE', #118724, #51708 ) ;
#73322 = CIRCLE ( 'NONE', #125552, 0.1000000000000000472 ) ;
#73323 = FACE_OUTER_BOUND ( 'NONE', #79313, .T. ) ;
#73324 = EDGE_LOOP ( 'NONE', ( #80211, #96617, #28182, #71790 ) ) ;
#73325 = EDGE_LOOP ( 'NONE', ( #71989, #15459 ) ) ;
#73326 = EDGE_CURVE ( 'NONE', #105503, #41725, #67612, .T. ) ;
#73327 = AXIS2_PLACEMENT_3D ( 'NONE', #36401, #76314, #6892 ) ;
#73328 = ORIENTED_EDGE ( 'NONE', *, *, #63162, .F. ) ;
#73329 = VERTEX_POINT ( 'NONE', #48636 ) ;
#73330 = DIRECTION ( 'NONE',  ( 0.000000000000000000, 0.000000000000000000, 1.000000000000000000 ) ) ;
#73331 = FACE_OUTER_BOUND ( 'NONE', #60592, .T. ) ;
#73332 = ADVANCED_FACE ( 'NONE', ( #78760 ), #70536, .T. ) ;
#73333 = CARTESIAN_POINT ( 'NONE',  ( 0.4499999999999573785, 2.500000000000000000, -6.395190528383301931 ) ) ;
#73334 = CARTESIAN_POINT ( 'NONE',  ( 5.199999999999933564, 2.500000000000000000, 0.3464101615137735735 ) ) ;
#73335 = DIRECTION ( 'NONE',  ( -0.000000000000000000, 1.000000000000000000, -0.000000000000000000 ) ) ;
#73336 = ORIENTED_EDGE ( 'NONE', *, *, #57573, .F. ) ;
#73337 = DIRECTION ( 'NONE',  ( 0.000000000000000000, 0.000000000000000000, 1.000000000000000000 ) ) ;
#73338 = ADVANCED_FACE ( 'NONE', ( #128516 ), #30854, .T. ) ;
#73339 = ADVANCED_FACE ( 'NONE', ( #96426 ), #87256, .T. ) ;
#73340 = CARTESIAN_POINT ( 'NONE',  ( 0.5999999999999621192, 12.50000000000000000, 0.3464101615137758494 ) ) ;
#73341 = ADVANCED_FACE ( 'NONE', ( #17201 ), #66328, .T. ) ;
#73342 = CARTESIAN_POINT ( 'NONE',  ( 8.749999999999957367, 2.500000000000000000, 2.065063509461097624 ) ) ;
#73343 = ADVANCED_FACE ( 'NONE', ( #117334 ), #127208, .T. ) ;
#73344 = DIRECTION ( 'NONE',  ( 0.000000000000000000, 0.000000000000000000, 1.000000000000000000 ) ) ;
#73345 = EDGE_LOOP ( 'NONE', ( #95413, #113499, #22914, #119998 ) ) ;
#73346 = EDGE_LOOP ( 'NONE', ( #121718, #118542 ) ) ;
#73348 = ORIENTED_EDGE ( 'NONE', *, *, #8063, .F. ) ;
#73347 = EDGE_CURVE ( 'NONE', #106262, #9617, #7834, .T. ) ;
#73349 = VECTOR ( 'NONE', #108728, 1000.000000000000000 ) ;
#73350 = CARTESIAN_POINT ( 'NONE',  ( -3.469446951953614189E-14, 2.500000000000000000, -0.6928203230275519209 ) ) ;
#73351 = CIRCLE ( 'NONE', #75408, 0.06509327318403745899 ) ;
#73352 = CONICAL_SURFACE ( 'NONE', #71211, 0.09999999999999999167, 0.003490658503988666988 ) ;
#73353 = EDGE_CURVE ( 'NONE', #96049, #39206, #2094, .T. ) ;
#73354 = DIRECTION ( 'NONE',  ( -0.000000000000000000, 1.000000000000000000, -0.000000000000000000 ) ) ;
#73355 = CARTESIAN_POINT ( 'NONE',  ( -13.54999999999998828, 2.500000000000000000, 1.918653347947325338 ) ) ;
#73356 = ADVANCED_FACE ( 'NONE', ( #110131 ), #93530, .T. ) ;
#73358 = EDGE_CURVE ( 'NONE', #19796, #87887, #12044, .T. ) ;
#73357 = AXIS2_PLACEMENT_3D ( 'NONE', #87842, #39433, #51813 ) ;
#73360 = VERTEX_POINT ( 'NONE', #91778 ) ;
#73359 = AXIS2_PLACEMENT_3D ( 'NONE', #42909, #12119, #50771 ) ;
#73361 = CARTESIAN_POINT ( 'NONE',  ( 2.299999999999947864, 2.500000000000000000, 3.983716857408420964 ) ) ;
#73362 = DIRECTION ( 'NONE',  ( 0.000000000000000000, 0.000000000000000000, 1.000000000000000000 ) ) ;
#73363 = ADVANCED_FACE ( 'NONE', ( #42043 ), #26630, .T. ) ;
#73364 = DIRECTION ( 'NONE',  ( 0.000000000000000000, 0.000000000000000000, -1.000000000000000000 ) ) ;
#73365 = DIRECTION ( 'NONE',  ( 0.000000000000000000, 0.000000000000000000, -1.000000000000000000 ) ) ;
#73366 = EDGE_CURVE ( 'NONE', #25430, #40175, #49632, .T. ) ;
#73367 = CARTESIAN_POINT ( 'NONE',  ( -2.100000000000033840, 12.50000000000000000, 3.572213422710607489 ) ) ;
#73368 = ORIENTED_EDGE ( 'NONE', *, *, #72801, .T. ) ;
#73369 = ORIENTED_EDGE ( 'NONE', *, *, #1629, .T. ) ;
#73370 = LINE ( 'NONE', #103489, #16684 ) ;
#73371 = LINE ( 'NONE', #44569, #14226 ) ;
#73372 = DIRECTION ( 'NONE',  ( 0.000000000000000000, 1.000000000000000000, 0.000000000000000000 ) ) ;
#73373 = DIRECTION ( 'NONE',  ( 0.000000000000000000, 0.000000000000000000, 1.000000000000000000 ) ) ;
#73374 = DIRECTION ( 'NONE',  ( 0.000000000000000000, 0.000000000000000000, -1.000000000000000000 ) ) ;
#73375 = ORIENTED_EDGE ( 'NONE', *, *, #69373, .T. ) ;
#73376 = VECTOR ( 'NONE', #104662, 1000.000000000000000 ) ;
#73377 = ORIENTED_EDGE ( 'NONE', *, *, #116236, .T. ) ;
#73378 = DIRECTION ( 'NONE',  ( 0.000000000000000000, 1.000000000000000000, 0.000000000000000000 ) ) ;
#73379 = FACE_OUTER_BOUND ( 'NONE', #31311, .T. ) ;
#73380 = FACE_OUTER_BOUND ( 'NONE', #56437, .T. ) ;
#73381 = DIRECTION ( 'NONE',  ( 0.000000000000000000, 0.000000000000000000, -1.000000000000000000 ) ) ;
#73382 = DIRECTION ( 'NONE',  ( 0.000000000000000000, 0.000000000000000000, 1.000000000000000000 ) ) ;
#73383 = EDGE_LOOP ( 'NONE', ( #98091, #50061, #82648, #82624 ) ) ;
#73384 = CONICAL_SURFACE ( 'NONE', #65060, 0.1000000000000002554, 0.003490658503988666988 ) ;
#73385 = DIRECTION ( 'NONE',  ( 0.000000000000000000, 0.000000000000000000, -1.000000000000000000 ) ) ;
#73386 = AXIS2_PLACEMENT_3D ( 'NONE', #106481, #56080, #97945 ) ;
#73387 = DIRECTION ( 'NONE',  ( 0.000000000000000000, 1.000000000000000000, 0.000000000000000000 ) ) ;
#73388 = ORIENTED_EDGE ( 'NONE', *, *, #43845, .T. ) ;
#73389 = DIRECTION ( 'NONE',  ( 0.000000000000000000, 0.000000000000000000, 1.000000000000000000 ) ) ;
#73390 = ORIENTED_EDGE ( 'NONE', *, *, #22047, .F. ) ;
#73391 = AXIS2_PLACEMENT_3D ( 'NONE', #22690, #62608, #112981 ) ;
#73392 = DIRECTION ( 'NONE',  ( 0.000000000000000000, -0.000000000000000000, 1.000000000000000000 ) ) ;
#73393 = CIRCLE ( 'NONE', #23222, 0.1000000000000000056 ) ;
#73394 = EDGE_CURVE ( 'NONE', #8233, #51670, #118562, .T. ) ;
#73395 = ORIENTED_EDGE ( 'NONE', *, *, #102634, .T. ) ;
#73396 = CARTESIAN_POINT ( 'NONE',  ( -2.500000000000030642, 12.50000000000000000, -0.6928203230275541413 ) ) ;
#73397 = CARTESIAN_POINT ( 'NONE',  ( 3.749999999999978684, 2.500000000000000000, -6.595190528383302109 ) ) ;
#73398 = EDGE_CURVE ( 'NONE', #2346, #119558, #114448, .T. ) ;
#73399 = ORIENTED_EDGE ( 'NONE', *, *, #94511, .F. ) ;
#73400 = ORIENTED_EDGE ( 'NONE', *, *, #39373, .T. ) ;
#73401 = CARTESIAN_POINT ( 'NONE',  ( 184.5885416670080872, -6.551208109652273848, -3.782341765625003571 ) ) ;
#73402 = CARTESIAN_POINT ( 'NONE',  ( 108.0000000000000142, 8.500000000000000000, 0.000000000000000000 ) ) ;
#73404 = DIRECTION ( 'NONE',  ( -0.000000000000000000, 1.000000000000000000, -0.000000000000000000 ) ) ;
#73403 = AXIS2_PLACEMENT_3D ( 'NONE', #65303, #115698, #5735 ) ;
#73405 = CARTESIAN_POINT ( 'NONE',  ( 185.4843750003414016, -8.734944146203032389, -1.604583208406767949E-15 ) ) ;
#73406 = AXIS2_PLACEMENT_3D ( 'NONE', #56627, #78891, #9489 ) ;
#73407 = CARTESIAN_POINT ( 'NONE',  ( 8.149999999999920419, 12.50000000000000000, 6.083687093685483660 ) ) ;
#73408 = DIRECTION ( 'NONE',  ( 0.000000000000000000, 0.000000000000000000, 1.000000000000000000 ) ) ;
#73409 = LINE ( 'NONE', #97406, #47415 ) ;
#73410 = CARTESIAN_POINT ( 'NONE',  ( 6.449999999999928235, 12.50000000000000000, 2.511473670974873507 ) ) ;
#73411 = CIRCLE ( 'NONE', #16948, 0.06509327318403745899 ) ;
#73412 = ORIENTED_EDGE ( 'NONE', *, *, #66677, .T. ) ;
#73413 = ORIENTED_EDGE ( 'NONE', *, *, #104431, .F. ) ;
#73414 = CARTESIAN_POINT ( 'NONE',  ( 14.14999999999989733, 12.50000000000000000, 2.857883832488649301 ) ) ;
#73415 = ORIENTED_EDGE ( 'NONE', *, *, #81203, .F. ) ;
#73416 = VECTOR ( 'NONE', #536, 1000.000000000000000 ) ;
#73417 = DIRECTION ( 'NONE',  ( 0.000000000000000000, 0.000000000000000000, -1.000000000000000000 ) ) ;
#73418 = DIRECTION ( 'NONE',  ( 0.000000000000000000, 0.000000000000000000, 1.000000000000000000 ) ) ;
#73419 = FACE_OUTER_BOUND ( 'NONE', #32666, .T. ) ;
#73421 = ORIENTED_EDGE ( 'NONE', *, *, #114728, .F. ) ;
#73420 = EDGE_LOOP ( 'NONE', ( #65203, #61555, #127605, #90009 ) ) ;
#73422 = FACE_BOUND ( 'NONE', #268, .T. ) ;
#73423 = ORIENTED_EDGE ( 'NONE', *, *, #71744, .T. ) ;
#73424 = PLANE ( 'NONE',  #42956 ) ;
#73425 = CARTESIAN_POINT ( 'NONE',  ( -12.89999999999999147, 12.50000000000000000, -0.6928203230275500335 ) ) ;
#73426 = CARTESIAN_POINT ( 'NONE',  ( 14.34999999999989662, 2.500000000000000000, 2.511473670974873507 ) ) ;
#73427 = DIRECTION ( 'NONE',  ( 0.000000000000000000, 0.000000000000000000, 1.000000000000000000 ) ) ;
#73428 = DIRECTION ( 'NONE',  ( 0.000000000000000000, 0.000000000000000000, -1.000000000000000000 ) ) ;
#73429 = DIRECTION ( 'NONE',  ( -0.000000000000000000, 1.000000000000000000, -0.000000000000000000 ) ) ;
#73430 = CARTESIAN_POINT ( 'NONE',  ( 12.04999999999990834, 2.500000000000000000, 6.495190528383297135 ) ) ;
#73431 = DIRECTION ( 'NONE',  ( -0.000000000000000000, -1.000000000000000000, -0.000000000000000000 ) ) ;
#73432 = FACE_OUTER_BOUND ( 'NONE', #97635, .T. ) ;
#73433 = CARTESIAN_POINT ( 'NONE',  ( 9.799999999999917222, 2.500000000000000000, 0.3464101615137735735 ) ) ;
#73434 = CARTESIAN_POINT ( 'NONE',  ( 4.149999999999939959, 2.500000000000000000, -2.165063509461101710 ) ) ;
#73435 = EDGE_CURVE ( 'NONE', #34432, #118817, #72151, .T. ) ;
#73436 = VERTEX_POINT ( 'NONE', #121881 ) ;
#73437 = ORIENTED_EDGE ( 'NONE', *, *, #100137, .F. ) ;
#73438 = ORIENTED_EDGE ( 'NONE', *, *, #111619, .F. ) ;
#73439 = CARTESIAN_POINT ( 'NONE',  ( -2.900000000000030553, 12.50000000000000000, 5.088040615133786027 ) ) ;
#73440 = ORIENTED_EDGE ( 'NONE', *, *, #67132, .F. ) ;
#73441 = AXIS2_PLACEMENT_3D ( 'NONE', #62228, #2628, #83781 ) ;
#73442 = DIRECTION ( 'NONE',  ( 0.000000000000000000, 1.000000000000000000, 0.000000000000000000 ) ) ;
#73443 = CIRCLE ( 'NONE', #94372, 0.06509327318403745899 ) ;
#73444 = AXIS2_PLACEMENT_3D ( 'NONE', #46763, #9415, #86672 ) ;
#73446 = ORIENTED_EDGE ( 'NONE', *, *, #45750, .F. ) ;
#73445 = EDGE_LOOP ( 'NONE', ( #40199, #3550 ) ) ;
#73447 = EDGE_LOOP ( 'NONE', ( #3199, #104000, #13155, #17338, #76229, #117556 ) ) ;
#73448 = CARTESIAN_POINT ( 'NONE',  ( -1.050000000000038680, 12.50000000000000000, 2.511473670974873507 ) ) ;
#73449 = VECTOR ( 'NONE', #50356, 1000.000000000000000 ) ;
#73450 = DIRECTION ( 'NONE',  ( 0.000000000000000000, -0.9999939076577903929, 0.003490651415223739937 ) ) ;
#73451 = CONICAL_SURFACE ( 'NONE', #77654, 0.1000000000000002554, 0.003490658503988666988 ) ;
#73452 = CARTESIAN_POINT ( 'NONE',  ( 187.0000000000000000, 0.000000000000000000, 7.700000000000000178 ) ) ;
#73453 = DIRECTION ( 'NONE',  ( -4.274815082592931898E-19, -0.9999939076577903929, -0.003490651415223739937 ) ) ;
#73455 = EDGE_CURVE ( 'NONE', #81450, #18351, #2744, .T. ) ;
#73454 = CIRCLE ( 'NONE', #31617, 0.1000000000000000472 ) ;
#73456 = FACE_OUTER_BOUND ( 'NONE', #106175, .T. ) ;
#73457 = ADVANCED_FACE ( 'NONE', ( #81324 ), #102252, .T. ) ;
#73458 = EDGE_LOOP ( 'NONE', ( #78338, #108758 ) ) ;
#73459 = DIRECTION ( 'NONE',  ( 0.000000000000000000, 0.000000000000000000, -1.000000000000000000 ) ) ;
#73460 = EDGE_LOOP ( 'NONE', ( #76709, #102085 ) ) ;
#73461 = EDGE_LOOP ( 'NONE', ( #49993, #221 ) ) ;
#73462 = ORIENTED_EDGE ( 'NONE', *, *, #32460, .F. ) ;
#73463 = DIRECTION ( 'NONE',  ( -0.000000000000000000, -1.000000000000000000, -0.000000000000000000 ) ) ;
#73464 = EDGE_LOOP ( 'NONE', ( #102379, #49278, #80557, #113526 ) ) ;
#73465 = ADVANCED_FACE ( 'NONE', ( #40774 ), #9906, .T. ) ;
#73466 = ORIENTED_EDGE ( 'NONE', *, *, #78073, .F. ) ;
#73467 = VERTEX_POINT ( 'NONE', #80027 ) ;
#73468 = CARTESIAN_POINT ( 'NONE',  ( -4.800000000000028244, 12.50000000000000000, -3.983716857408426293 ) ) ;
#73469 = DIRECTION ( 'NONE',  ( 0.000000000000000000, 0.000000000000000000, 1.000000000000000000 ) ) ;
#73470 = CARTESIAN_POINT ( 'NONE',  ( -4.999999999999986677, 2.500000000000000000, 4.230127018922196669 ) ) ;
#73471 = FACE_OUTER_BOUND ( 'NONE', #2944, .T. ) ;
#73472 = DIRECTION ( 'NONE',  ( 0.000000000000000000, 1.000000000000000000, 0.000000000000000000 ) ) ;
#73473 = CARTESIAN_POINT ( 'NONE',  ( 1.249999999999988454, 2.500000000000000000, 2.165063509461097713 ) ) ;
#73474 = DIRECTION ( 'NONE',  ( 0.000000000000000000, -0.000000000000000000, 1.000000000000000000 ) ) ;
#73475 = AXIS2_PLACEMENT_3D ( 'NONE', #102638, #72560, #124873 ) ;
#73476 = CIRCLE ( 'NONE', #69268, 0.06509327318403745899 ) ;
#73477 = ORIENTED_EDGE ( 'NONE', *, *, #126642, .T. ) ;
#73478 = FACE_OUTER_BOUND ( 'NONE', #77443, .T. ) ;
#73479 = ORIENTED_EDGE ( 'NONE', *, *, #103952, .F. ) ;
#73480 = DIRECTION ( 'NONE',  ( 0.000000000000000000, 1.000000000000000000, 0.000000000000000000 ) ) ;
#73481 = EDGE_LOOP ( 'NONE', ( #125748, #121132 ) ) ;
#73482 = EDGE_LOOP ( 'NONE', ( #51889, #4339, #87305, #8164 ) ) ;
#73483 = DIRECTION ( 'NONE',  ( 0.000000000000000000, 1.000000000000000000, 0.000000000000000000 ) ) ;
#73484 = FACE_OUTER_BOUND ( 'NONE', #10739, .T. ) ;
#73485 = CONICAL_SURFACE ( 'NONE', #79759, 0.09999999999999982514, 0.003490658503988666988 ) ;
#73486 = ADVANCED_FACE ( 'NONE', ( #119297 ), #24572, .T. ) ;
#73487 = CONICAL_SURFACE ( 'NONE', #33784, 0.1000000000000002554, 0.003490658503988666988 ) ;
#73488 = DIRECTION ( 'NONE',  ( -0.000000000000000000, 1.000000000000000000, -0.000000000000000000 ) ) ;
#73489 = EDGE_LOOP ( 'NONE', ( #30805, #92581 ) ) ;
#73490 = VERTEX_POINT ( 'NONE', #91137 ) ;
#73491 =( BOUNDED_CURVE ( )  B_SPLINE_CURVE ( 2, ( #76543, #87632, #66705, #58204, #127571, #77811, #117726 ),
 .UNSPECIFIED., .F., .F. ) 
 B_SPLINE_CURVE_WITH_KNOTS ( ( 3, 2, 2, 3 ),
 ( 0.7142857142857148567, 0.7380952380952386926, 0.7619047619047624176, 0.7857142857142862535 ),
 .UNSPECIFIED. ) 
 CURVE ( )  GEOMETRIC_REPRESENTATION_ITEM ( )  RATIONAL_B_SPLINE_CURVE ( ( 0.9999999999999968914, 0.8660254037844418162, 1.000000000000000000, 0.8660254037844387076, 1.000000000000000000, 0.8660254037844355990, 1.000000000000003109 ) ) 
 REPRESENTATION_ITEM ( '' )  );
#73492 = FACE_OUTER_BOUND ( 'NONE', #35815, .T. ) ;
#73493 = DIRECTION ( 'NONE',  ( 0.000000000000000000, 0.000000000000000000, 1.000000000000000000 ) ) ;
#73494 = EDGE_CURVE ( 'NONE', #60152, #65538, #61025, .T. ) ;
#73495 = CARTESIAN_POINT ( 'NONE',  ( -7.700000000000014388, 2.500000000000000000, -0.2464101615137782308 ) ) ;
#73496 = DIRECTION ( 'NONE',  ( 0.000000000000000000, 0.000000000000000000, 1.000000000000000000 ) ) ;
#73497 = EDGE_CURVE ( 'NONE', #49149, #123206, #50553, .T. ) ;
#73498 = CONICAL_SURFACE ( 'NONE', #75637, 0.1000000000000000472, 0.003490658503988666988 ) ;
#73499 = CONICAL_SURFACE ( 'NONE', #69387, 0.1000000000000000472, 0.003490658503988666988 ) ;
#73500 = CARTESIAN_POINT ( 'NONE',  ( -3.150000000000033218, 2.500000000000000000, -6.841600689897078702 ) ) ;
#73501 = EDGE_LOOP ( 'NONE', ( #33065, #83657 ) ) ;
#73502 = VECTOR ( 'NONE', #78369, 1000.000000000000000 ) ;
#73503 = EDGE_CURVE ( 'NONE', #69257, #17553, #60410, .T. ) ;
#73504 = EDGE_CURVE ( 'NONE', #122281, #16616, #1455, .T. ) ;
#73505 = EDGE_CURVE ( 'NONE', #11230, #48106, #124923, .T. ) ;
#73506 = ORIENTED_EDGE ( 'NONE', *, *, #50755, .F. ) ;
#73507 = CARTESIAN_POINT ( 'NONE',  ( -10.20000000000000284, 12.50000000000000000, -0.3464101615137782364 ) ) ;
#73508 = CARTESIAN_POINT ( 'NONE',  ( -8.150000000000012790, 12.50000000000000000, -2.511473670974877948 ) ) ;
#73509 = EDGE_CURVE ( 'NONE', #114154, #39901, #28788, .T. ) ;
#73510 = AXIS2_PLACEMENT_3D ( 'NONE', #17194, #5462, #125880 ) ;
#73511 = AXIS2_PLACEMENT_3D ( 'NONE', #1038, #61259, #19372 ) ;
#73512 = CARTESIAN_POINT ( 'NONE',  ( 185.2552083336747444, 6.551208109652275624, -3.782341765624998686 ) ) ;
#73513 = DIRECTION ( 'NONE',  ( 0.000000000000000000, 0.000000000000000000, -1.000000000000000000 ) ) ;
#73514 = DIRECTION ( 'NONE',  ( -0.000000000000000000, -1.000000000000000000, -0.000000000000000000 ) ) ;
#73515 = CARTESIAN_POINT ( 'NONE',  ( 11.24999999999990585, 2.500000000000000000, -5.702370205355749455 ) ) ;
#73516 = FACE_OUTER_BOUND ( 'NONE', #80069, .T. ) ;
#73517 = ORIENTED_EDGE ( 'NONE', *, *, #28, .T. ) ;
#73518 = EDGE_CURVE ( 'NONE', #108189, #82135, #109439, .T. ) ;
#73519 = CARTESIAN_POINT ( 'NONE',  ( 3.349999999999945466, 12.50000000000000000, -7.188010851410854052 ) ) ;
#73520 = CARTESIAN_POINT ( 'NONE',  ( -13.34999999999999076, 12.50000000000000000, -1.472243186433547901 ) ) ;
#73521 = DIRECTION ( 'NONE',  ( -0.000000000000000000, 1.000000000000000000, -0.000000000000000000 ) ) ;
#73522 = ORIENTED_EDGE ( 'NONE', *, *, #17496, .F. ) ;
#73523 = FACE_OUTER_BOUND ( 'NONE', #92654, .T. ) ;
#73524 = ORIENTED_EDGE ( 'NONE', *, *, #55826, .F. ) ;
#73525 = CARTESIAN_POINT ( 'NONE',  ( 105.5000000000000142, -1.500000000000000222, 1.322875655532295136 ) ) ;
#73526 = CONICAL_SURFACE ( 'NONE', #113244, 0.09999999999999999167, 0.003490658503988666988 ) ;
#73527 = AXIS2_PLACEMENT_3D ( 'NONE', #68505, #50182, #79621 ) ;
#73528 = CIRCLE ( 'NONE', #88091, 0.1000000000000002554 ) ;
#73529 = ORIENTED_EDGE ( 'NONE', *, *, #43979, .T. ) ;
#73530 = PLANE ( 'NONE',  #29156 ) ;
#73531 = CARTESIAN_POINT ( 'NONE',  ( -3.350000000000028511, 12.50000000000000000, 1.537336459617582918 ) ) ;
#73532 = FACE_OUTER_BOUND ( 'NONE', #41942, .T. ) ;
#73533 = ORIENTED_EDGE ( 'NONE', *, *, #6977, .T. ) ;
#73535 = CARTESIAN_POINT ( 'NONE',  ( -7.950000000000009059, 12.50000000000000000, 6.560283801567334372 ) ) ;
#73534 = CONICAL_SURFACE ( 'NONE', #4471, 0.1000000000000000056, 0.003490658503988666988 ) ;
#73536 = AXIS2_PLACEMENT_3D ( 'NONE', #20663, #102443, #31141 ) ;
#73537 = CARTESIAN_POINT ( 'NONE',  ( 3.299999999999942979, 2.500000000000000000, 4.230127018922196669 ) ) ;
#73538 = AXIS2_PLACEMENT_3D ( 'NONE', #83592, #103870, #54120 ) ;
#73539 = CIRCLE ( 'NONE', #17084, 0.06509327318403741736 ) ;
#73540 = ORIENTED_EDGE ( 'NONE', *, *, #8893, .F. ) ;
#73541 = AXIS2_PLACEMENT_3D ( 'NONE', #116230, #115577, #16082 ) ;
#73543 = ORIENTED_EDGE ( 'NONE', *, *, #82549, .T. ) ;
#73542 = EDGE_CURVE ( 'NONE', #53221, #2439, #76807, .T. ) ;
#73544 = EDGE_LOOP ( 'NONE', ( #23477, #61637 ) ) ;
#73545 = DIRECTION ( 'NONE',  ( 0.000000000000000000, 0.000000000000000000, 1.000000000000000000 ) ) ;
#73546 = CARTESIAN_POINT ( 'NONE',  ( -3.749999999999994671, 12.50000000000000000, -6.495190528383302464 ) ) ;
#73547 = CARTESIAN_POINT ( 'NONE',  ( -6.050000000000018474, 12.50000000000000000, 2.511473670974873507 ) ) ;
#73548 = ORIENTED_EDGE ( 'NONE', *, *, #123557, .F. ) ;
#73549 = DIRECTION ( 'NONE',  ( -0.000000000000000000, -1.000000000000000000, -0.000000000000000000 ) ) ;
#73550 = CARTESIAN_POINT ( 'NONE',  ( 184.5000000000000000, 0.000000000000000000, 0.000000000000000000 ) ) ;
#73551 = ORIENTED_EDGE ( 'NONE', *, *, #48720, .T. ) ;
#73552 = ADVANCED_FACE ( 'NONE', ( #93712 ), #85110, .T. ) ;
#73553 = CARTESIAN_POINT ( 'NONE',  ( -7.950000000000012612, 12.50000000000000000, -2.165063509461101710 ) ) ;
#73554 = CARTESIAN_POINT ( 'NONE',  ( -4.999999999999990230, 2.500000000000000000, -4.330127018922201643 ) ) ;
#73555 = CARTESIAN_POINT ( 'NONE',  ( 14.59999999999989484, 12.50000000000000000, -0.6928203230275541413 ) ) ;
#73556 = DIRECTION ( 'NONE',  ( 0.000000000000000000, 0.000000000000000000, 1.000000000000000000 ) ) ;
#73557 = DIRECTION ( 'NONE',  ( -0.000000000000000000, -1.000000000000000000, -0.000000000000000000 ) ) ;
#73558 = CARTESIAN_POINT ( 'NONE',  ( -12.89999999999999147, 12.50000000000000000, -0.6277270498435125745 ) ) ;
#73559 = CARTESIAN_POINT ( 'NONE',  ( -12.04999999999999538, 2.500000000000000000, 6.495190528383297135 ) ) ;
#73560 = CIRCLE ( 'NONE', #59006, 0.06509327318403745899 ) ;
#73561 = CIRCLE ( 'NONE', #117453, 0.06509327318403745899 ) ;
#73562 = ORIENTED_EDGE ( 'NONE', *, *, #90020, .F. ) ;
#73563 = VERTEX_POINT ( 'NONE', #25597 ) ;
#73564 = ORIENTED_EDGE ( 'NONE', *, *, #46179, .F. ) ;
#73565 = VERTEX_POINT ( 'NONE', #75347 ) ;
#73566 = LINE ( 'NONE', #115404, #124837 ) ;
#73567 = DIRECTION ( 'NONE',  ( 0.000000000000000000, 0.000000000000000000, 1.000000000000000000 ) ) ;
#73568 = CARTESIAN_POINT ( 'NONE',  ( -5.200000000000022382, 2.500000000000000000, 0.3464101615137735735 ) ) ;
#73569 = EDGE_LOOP ( 'NONE', ( #92986, #12171 ) ) ;
#73570 = FACE_BOUND ( 'NONE', #26424, .T. ) ;
#73571 = CONICAL_SURFACE ( 'NONE', #27596, 0.09999999999999982514, 0.003490658503988666988 ) ;
#73572 = CARTESIAN_POINT ( 'NONE',  ( 12.49999999999990585, 2.500000000000000000, -5.122947341949753763 ) ) ;
#73573 = DIRECTION ( 'NONE',  ( 0.000000000000000000, -0.000000000000000000, 1.000000000000000000 ) ) ;
#73574 = AXIS2_PLACEMENT_3D ( 'NONE', #120158, #21300, #61242 ) ;
#73576 = CARTESIAN_POINT ( 'NONE',  ( 3.749999999999942268, 2.500000000000000000, 1.372243186433545370 ) ) ;
#73575 = CONICAL_SURFACE ( 'NONE', #109069, 0.1000000000000000472, 0.003490658503988666988 ) ;
#73577 = CIRCLE ( 'NONE', #107017, 0.09999999999999982514 ) ;
#73578 = DIRECTION ( 'NONE',  ( 0.000000000000000000, 0.000000000000000000, 1.000000000000000000 ) ) ;
#73579 = DIRECTION ( 'NONE',  ( -0.000000000000000000, 1.000000000000000000, -0.000000000000000000 ) ) ;
#73580 = CARTESIAN_POINT ( 'NONE',  ( 2.499999999999983569, 2.500000000000000000, -2.276824562219559311E-15 ) ) ;
#73581 = DIRECTION ( 'NONE',  ( -0.000000000000000000, 1.000000000000000000, -0.000000000000000000 ) ) ;
#73582 = DIRECTION ( 'NONE',  ( 0.000000000000000000, 1.000000000000000000, 0.000000000000000000 ) ) ;
#73583 = DIRECTION ( 'NONE',  ( 0.000000000000000000, 0.000000000000000000, 1.000000000000000000 ) ) ;
#73584 = AXIS2_PLACEMENT_3D ( 'NONE', #89956, #101076, #43297 ) ;
#73585 = LINE ( 'NONE', #44139, #110758 ) ;
#73586 = ORIENTED_EDGE ( 'NONE', *, *, #71021, .F. ) ;
#73587 = CONICAL_SURFACE ( 'NONE', #33894, 0.1000000000000002554, 0.003490658503988666988 ) ;
#73588 = EDGE_CURVE ( 'NONE', #63275, #40211, #13201, .T. ) ;
#73589 = ORIENTED_EDGE ( 'NONE', *, *, #119224, .F. ) ;
#73590 = ORIENTED_EDGE ( 'NONE', *, *, #30995, .F. ) ;
#73591 = VERTEX_POINT ( 'NONE', #54421 ) ;
#73593 = VERTEX_POINT ( 'NONE', #105469 ) ;
#73592 = CIRCLE ( 'NONE', #27612, 0.1000000000000002554 ) ;
#73594 = CONICAL_SURFACE ( 'NONE', #8742, 0.1000000000000002554, 0.003490658503988666988 ) ;
#73595 = AXIS2_PLACEMENT_3D ( 'NONE', #96942, #24989, #34837 ) ;
#73596 = EDGE_LOOP ( 'NONE', ( #66814, #49976, #349, #90445 ) ) ;
#73597 = DIRECTION ( 'NONE',  ( 0.000000000000000000, 0.000000000000000000, 1.000000000000000000 ) ) ;
#73598 = VERTEX_POINT ( 'NONE', #4029 ) ;
#73599 = ORIENTED_EDGE ( 'NONE', *, *, #128035, .F. ) ;
#73600 = TOROIDAL_SURFACE ( 'NONE', #23428, 7.541925104783893552, 0.5000000000000000000 ) ;
#73601 = EDGE_CURVE ( 'NONE', #53445, #31778, #3397, .T. ) ;
#73602 = CONICAL_SURFACE ( 'NONE', #100699, 0.09999999999999982514, 0.003490658503988666988 ) ;
#73603 = CARTESIAN_POINT ( 'NONE',  ( 16.56576425164984201, -1.500000000000000000, 6.084390597446049043 ) ) ;
#73604 = CARTESIAN_POINT ( 'NONE',  ( 187.5000000000000000, 0.000000000000000000, 0.000000000000000000 ) ) ;
#73605 = DIRECTION ( 'NONE',  ( 0.000000000000000000, 0.000000000000000000, -1.000000000000000000 ) ) ;
#73606 = EDGE_CURVE ( 'NONE', #123356, #98747, #3642, .T. ) ;
#73607 = EDGE_CURVE ( 'NONE', #67054, #23927, #37107, .T. ) ;
#73608 = ORIENTED_EDGE ( 'NONE', *, *, #9835, .T. ) ;
#73609 = DIRECTION ( 'NONE',  ( 0.000000000000000000, -0.9999939076577903929, 0.003490651415223739937 ) ) ;
#73610 = EDGE_LOOP ( 'NONE', ( #11351, #9201, #56619, #118348 ) ) ;
#73611 = ORIENTED_EDGE ( 'NONE', *, *, #87672, .F. ) ;
#73613 = ORIENTED_EDGE ( 'NONE', *, *, #36547, .T. ) ;
#73612 = DIRECTION ( 'NONE',  ( 0.000000000000000000, -0.000000000000000000, 1.000000000000000000 ) ) ;
#73614 = EDGE_CURVE ( 'NONE', #106514, #79569, #64879, .T. ) ;
#73615 = CARTESIAN_POINT ( 'NONE',  ( 9.599999999999917932, 2.500000000000000000, 0.5928203230275495006 ) ) ;
#73616 = EDGE_CURVE ( 'NONE', #54834, #80090, #14180, .T. ) ;
#73617 = VERTEX_POINT ( 'NONE', #23043 ) ;
#73618 = FACE_OUTER_BOUND ( 'NONE', #66928, .T. ) ;
#73619 = CARTESIAN_POINT ( 'NONE',  ( -8.749999999999975131, 2.500000000000000000, -2.265063509461101798 ) ) ;
#73620 = CARTESIAN_POINT ( 'NONE',  ( 5.849999999999932143, 2.500000000000000000, 1.372243186433545370 ) ) ;
#73622 = DIRECTION ( 'NONE',  ( -0.000000000000000000, -1.000000000000000000, -0.000000000000000000 ) ) ;
#73621 = AXIS2_PLACEMENT_3D ( 'NONE', #50869, #69200, #71142 ) ;
#73623 = AXIS2_PLACEMENT_3D ( 'NONE', #90327, #60887, #674 ) ;
#73624 = CARTESIAN_POINT ( 'NONE',  ( -1.250000000000037970, 2.500000000000000000, 2.857883832488649301 ) ) ;
#73625 = ORIENTED_EDGE ( 'NONE', *, *, #121835, .T. ) ;
#73626 = DIRECTION ( 'NONE',  ( 0.000000000000000000, 1.000000000000000000, 0.000000000000000000 ) ) ;
#73627 = AXIS2_PLACEMENT_3D ( 'NONE', #58738, #18797, #31696 ) ;
#73629 = ORIENTED_EDGE ( 'NONE', *, *, #127884, .F. ) ;
#73628 = CIRCLE ( 'NONE', #8782, 0.1000000000000000472 ) ;
#73630 = CARTESIAN_POINT ( 'NONE',  ( 17.50000000000000000, 2.499999999999999556, -1.666666666666663410 ) ) ;
#73631 = CIRCLE ( 'NONE', #50659, 0.1000000000000002554 ) ;
#73632 = EDGE_LOOP ( 'NONE', ( #123554, #122454 ) ) ;
#73633 = CARTESIAN_POINT ( 'NONE',  ( 2.049999999999950084, 2.500000000000000000, -6.495190528383302464 ) ) ;
#73634 = DIRECTION ( 'NONE',  ( 0.000000000000000000, -0.9999939076577903929, 0.003490651415223739937 ) ) ;
#73635 = CIRCLE ( 'NONE', #54847, 0.06509327318403745899 ) ;
#73636 = CARTESIAN_POINT ( 'NONE',  ( 6.049999999999934097, 2.500000000000000000, 6.048780366869521252 ) ) ;
#73637 = DIRECTION ( 'NONE',  ( -0.000000000000000000, 1.000000000000000000, -0.000000000000000000 ) ) ;
#73638 = EDGE_LOOP ( 'NONE', ( #51650, #20651, #35763, #49407 ) ) ;
#73639 = CIRCLE ( 'NONE', #119612, 0.1000000000000002554 ) ;
#73640 = FACE_OUTER_BOUND ( 'NONE', #124142, .T. ) ;
#73641 = CARTESIAN_POINT ( 'NONE',  ( -4.200000000000025935, 12.50000000000000000, 4.330127018922196314 ) ) ;
#73642 = ORIENTED_EDGE ( 'NONE', *, *, #112374, .F. ) ;
#73643 = EDGE_LOOP ( 'NONE', ( #117359, #114388, #33668, #28202 ) ) ;
#73644 = ORIENTED_EDGE ( 'NONE', *, *, #70522, .T. ) ;
#73645 = DIRECTION ( 'NONE',  ( 0.000000000000000000, 0.000000000000000000, 1.000000000000000000 ) ) ;
#73646 = DIRECTION ( 'NONE',  ( 0.000000000000000000, -0.000000000000000000, 1.000000000000000000 ) ) ;
#73647 = CARTESIAN_POINT ( 'NONE',  ( 184.9427083336747160, -6.551208109652278289, 3.782341765624995134 ) ) ;
#73648 = DIRECTION ( 'NONE',  ( 0.000000000000000000, 0.000000000000000000, -1.000000000000000000 ) ) ;
#73649 = ADVANCED_FACE ( 'NONE', ( #24331 ), #24969, .T. ) ;
#73650 = CARTESIAN_POINT ( 'NONE',  ( 17.27571223834410219, 2.230085210383166316, -5.047251339834024186 ) ) ;
#73651 = DIRECTION ( 'NONE',  ( -4.274815082592931898E-19, -0.9999939076577903929, -0.003490651415223739937 ) ) ;
#73652 = EDGE_CURVE ( 'NONE', #41483, #54886, #5318, .T. ) ;
#73653 = EDGE_CURVE ( 'NONE', #33436, #73847, #37197, .T. ) ;
#73654 = ADVANCED_FACE ( 'NONE', ( #5954 ), #16228, .T. ) ;
#73655 = AXIS2_PLACEMENT_3D ( 'NONE', #76265, #116167, #26516 ) ;
#73656 = ORIENTED_EDGE ( 'NONE', *, *, #70036, .T. ) ;
#73657 = CARTESIAN_POINT ( 'NONE',  ( 11.84999999999990727, 2.500000000000000000, -2.511473670974877948 ) ) ;
#73658 = AXIS2_PLACEMENT_3D ( 'NONE', #1043, #92006, #381 ) ;
#73659 = ORIENTED_EDGE ( 'NONE', *, *, #51179, .T. ) ;
#73660 = EDGE_CURVE ( 'NONE', #39039, #37067, #70633, .T. ) ;
#73661 = DIRECTION ( 'NONE',  ( 0.000000000000000000, -0.9999939076577903929, 0.003490651415223739937 ) ) ;
#73662 = LINE ( 'NONE', #94588, #60097 ) ;
#73663 = DIRECTION ( 'NONE',  ( -0.000000000000000000, -1.000000000000000000, -0.000000000000000000 ) ) ;
#73664 = CARTESIAN_POINT ( 'NONE',  ( -6.450000000000014388, 12.50000000000000000, 1.818653347947321475 ) ) ;
#73665 = CIRCLE ( 'NONE', #27695, 0.06509327318403745899 ) ;
#73666 = ORIENTED_EDGE ( 'NONE', *, *, #15762, .T. ) ;
#73667 = ADVANCED_FACE ( 'NONE', ( #63618 ), #74844, .T. ) ;
#73668 = CIRCLE ( 'NONE', #50691, 0.06509327318403745899 ) ;
#73669 = EDGE_CURVE ( 'NONE', #81872, #44930, #24669, .T. ) ;
#73670 = AXIS2_PLACEMENT_3D ( 'NONE', #73507, #2843, #34907 ) ;
#73671 = DIRECTION ( 'NONE',  ( 1.000000000000000000, 0.000000000000000000, -7.228014483236698281E-17 ) ) ;
#73673 = ORIENTED_EDGE ( 'NONE', *, *, #97039, .F. ) ;
#73672 = CARTESIAN_POINT ( 'NONE',  ( 8.349999999999919709, 2.500000000000000000, 7.288010851410849256 ) ) ;
#73674 = VECTOR ( 'NONE', #107348, 1000.000000000000000 ) ;
#73675 = VERTEX_POINT ( 'NONE', #18363 ) ;
#73676 = LINE ( 'NONE', #63224, #126190 ) ;
#73677 = ORIENTED_EDGE ( 'NONE', *, *, #128557, .F. ) ;
#73678 = AXIS2_PLACEMENT_3D ( 'NONE', #124352, #94883, #5197 ) ;
#73680 = ORIENTED_EDGE ( 'NONE', *, *, #40155, .F. ) ;
#73679 = AXIS2_PLACEMENT_3D ( 'NONE', #98909, #9247, #49196 ) ;
#73681 = AXIS2_PLACEMENT_3D ( 'NONE', #19018, #119813, #98878 ) ;
#73682 = DIRECTION ( 'NONE',  ( 0.000000000000000000, 0.000000000000000000, -1.000000000000000000 ) ) ;
#73684 = EDGE_LOOP ( 'NONE', ( #125133, #124885, #83029, #104654 ) ) ;
#73683 = CIRCLE ( 'NONE', #59141, 0.1000000000000002554 ) ;
#73685 = CARTESIAN_POINT ( 'NONE',  ( 16.68526679984143613, 0.4774970013437123129, -5.954360761636884547 ) ) ;
#73686 = DIRECTION ( 'NONE',  ( -0.000000000000000000, -1.000000000000000000, -0.000000000000000000 ) ) ;
#73687 = DIRECTION ( 'NONE',  ( -4.274815082592931898E-19, -0.9999939076577903929, -0.003490651415223739937 ) ) ;
#73688 = ORIENTED_EDGE ( 'NONE', *, *, #11201, .T. ) ;
#73689 = CIRCLE ( 'NONE', #17240, 0.06509327318403745899 ) ;
#73690 = DIRECTION ( 'NONE',  ( 0.000000000000000000, -0.9999939076577903929, 0.003490651415223739937 ) ) ;
#73692 = VERTEX_POINT ( 'NONE', #36742 ) ;
#73691 = DIRECTION ( 'NONE',  ( 0.000000000000000000, 0.000000000000000000, 1.000000000000000000 ) ) ;
#73693 = DIRECTION ( 'NONE',  ( 0.000000000000000000, 0.000000000000000000, -1.000000000000000000 ) ) ;
#73694 = CARTESIAN_POINT ( 'NONE',  ( -9.600000000000006750, 2.500000000000000000, -0.6928203230275542523 ) ) ;
#73695 = VERTEX_POINT ( 'NONE', #125726 ) ;
#73696 = ORIENTED_EDGE ( 'NONE', *, *, #23388, .T. ) ;
#73697 = EDGE_LOOP ( 'NONE', ( #33008, #37326, #75098, #43239, #105796, #12350, #81051, #92821 ) ) ;
#73698 = VERTEX_POINT ( 'NONE', #7241 ) ;
#73699 = FACE_OUTER_BOUND ( 'NONE', #79819, .T. ) ;
#73700 = FACE_OUTER_BOUND ( 'NONE', #101831, .T. ) ;
#73701 = DIRECTION ( 'NONE',  ( 0.000000000000000000, -0.000000000000000000, 1.000000000000000000 ) ) ;
#73702 = AXIS2_PLACEMENT_3D ( 'NONE', #78674, #49221, #26991 ) ;
#73703 = FACE_BOUND ( 'NONE', #19617, .T. ) ;
#73704 = ORIENTED_EDGE ( 'NONE', *, *, #53564, .T. ) ;
#73705 = CARTESIAN_POINT ( 'NONE',  ( 187.2760416670080588, 6.551208109652274736, 3.782341765625001351 ) ) ;
#73706 = DIRECTION ( 'NONE',  ( 0.000000000000000000, 1.000000000000000000, 0.000000000000000000 ) ) ;
#73707 = DIRECTION ( 'NONE',  ( -4.274815082592931898E-19, -0.9999939076577903929, -0.003490651415223739937 ) ) ;
#73708 = EDGE_CURVE ( 'NONE', #41461, #120619, #96922, .T. ) ;
#73709 = AXIS2_PLACEMENT_3D ( 'NONE', #29783, #118803, #48790 ) ;
#73710 = VECTOR ( 'NONE', #75218, 1000.000000000000000 ) ;
#73712 = AXIS2_PLACEMENT_3D ( 'NONE', #110353, #76552, #80260 ) ;
#73711 = CARTESIAN_POINT ( 'NONE',  ( 5.649999999999934630, 2.500000000000000000, 6.941600689897073018 ) ) ;
#73713 = CARTESIAN_POINT ( 'NONE',  ( -14.39999999999998614, 12.50000000000000000, 0.3464101615137758494 ) ) ;
#73714 = CARTESIAN_POINT ( 'NONE',  ( -1.850000000000033396, 2.500000000000000000, -6.248780366869526759 ) ) ;
#73716 = DIRECTION ( 'NONE',  ( 0.000000000000000000, -0.9999939076577903929, 0.003490651415223739937 ) ) ;
#73715 = AXIS2_PLACEMENT_3D ( 'NONE', #122946, #82387, #91547 ) ;
#73717 = CIRCLE ( 'NONE', #102974, 0.06509327318403745899 ) ;
#73718 = ORIENTED_EDGE ( 'NONE', *, *, #26059, .F. ) ;
#73719 = ORIENTED_EDGE ( 'NONE', *, *, #23081, .T. ) ;
#73720 = ORIENTED_EDGE ( 'NONE', *, *, #100405, .F. ) ;
#73721 = ORIENTED_EDGE ( 'NONE', *, *, #24579, .F. ) ;
#73723 = ORIENTED_EDGE ( 'NONE', *, *, #95489, .F. ) ;
#73722 = AXIS2_PLACEMENT_3D ( 'NONE', #61720, #49974, #30330 ) ;
#73724 = DIRECTION ( 'NONE',  ( 0.000000000000000000, 0.000000000000000000, 1.000000000000000000 ) ) ;
#73725 = AXIS2_PLACEMENT_3D ( 'NONE', #92805, #10989, #43079 ) ;
#73726 = CIRCLE ( 'NONE', #40609, 0.06509327318403745899 ) ;
#73727 = DIRECTION ( 'NONE',  ( 0.000000000000000000, 1.000000000000000000, 0.000000000000000000 ) ) ;
#73728 = ORIENTED_EDGE ( 'NONE', *, *, #113745, .F. ) ;
#73729 = FACE_BOUND ( 'NONE', #127246, .T. ) ;
#73730 = CARTESIAN_POINT ( 'NONE',  ( 3.149999999999946176, 2.500000000000000000, -2.611473670974877592 ) ) ;
#73731 = EDGE_LOOP ( 'NONE', ( #97228, #70192, #58000, #99390 ) ) ;
#73732 = CARTESIAN_POINT ( 'NONE',  ( 0.3999999999999563904, 2.500000000000000000, 3.637306695894644726 ) ) ;
#73733 = DIRECTION ( 'NONE',  ( 0.000000000000000000, 1.000000000000000000, 0.000000000000000000 ) ) ;
#73734 = CARTESIAN_POINT ( 'NONE',  ( -11.84999999999999787, 2.500000000000000000, -1.918653347947322008 ) ) ;
#73735 = ORIENTED_EDGE ( 'NONE', *, *, #29737, .F. ) ;
#73736 = DIRECTION ( 'NONE',  ( 0.000000000000000000, 0.000000000000000000, 1.000000000000000000 ) ) ;
#73737 = VECTOR ( 'NONE', #25888, 1000.000000000000000 ) ;
#73738 = EDGE_LOOP ( 'NONE', ( #88547, #47245 ) ) ;
#73739 = ORIENTED_EDGE ( 'NONE', *, *, #35024, .F. ) ;
#73740 = VERTEX_POINT ( 'NONE', #96269 ) ;
#73741 = DIRECTION ( 'NONE',  ( 0.000000000000000000, -0.9999939076577903929, 0.003490651415223739937 ) ) ;
#73742 = CARTESIAN_POINT ( 'NONE',  ( -10.20000000000000284, 2.500000000000000000, -0.3464101615137782364 ) ) ;
#73743 = DIRECTION ( 'NONE',  ( -0.000000000000000000, 1.000000000000000000, -0.000000000000000000 ) ) ;
#73744 = VERTEX_POINT ( 'NONE', #58315 ) ;
#73745 = CARTESIAN_POINT ( 'NONE',  ( -8.350000000000012079, 2.500000000000000000, 1.472243186433545459 ) ) ;
#73746 = VECTOR ( 'NONE', #82048, 1000.000000000000000 ) ;
#73747 = EDGE_CURVE ( 'NONE', #15359, #33584, #18404, .T. ) ;
#73749 = LINE ( 'NONE', #124806, #7175 ) ;
#73748 = AXIS2_PLACEMENT_3D ( 'NONE', #81947, #63616, #11919 ) ;
#73750 = FACE_OUTER_BOUND ( 'NONE', #18466, .T. ) ;
#73751 = CARTESIAN_POINT ( 'NONE',  ( 186.1562500006828031, 8.891194145520236347, 5.444286225454521982E-16 ) ) ;
#73752 = VERTEX_POINT ( 'NONE', #47197 ) ;
#73753 = EDGE_CURVE ( 'NONE', #94819, #119696, #117840, .T. ) ;
#73754 = DIRECTION ( 'NONE',  ( 0.000000000000000000, 1.000000000000000000, 0.000000000000000000 ) ) ;
#73755 = CONICAL_SURFACE ( 'NONE', #92542, 0.1000000000000000472, 0.003490658503988666988 ) ;
#73756 = ADVANCED_FACE ( 'NONE', ( #6578 ), #7928, .T. ) ;
#73757 = EDGE_LOOP ( 'NONE', ( #80863, #99612 ) ) ;
#73758 = CARTESIAN_POINT ( 'NONE',  ( 194.5000000000000000, 0.000000000000000000, 0.000000000000000000 ) ) ;
#73759 = CIRCLE ( 'NONE', #17305, 0.06509327318403745899 ) ;
#73760 = VECTOR ( 'NONE', #66189, 1000.000000000000000 ) ;
#73761 = ORIENTED_EDGE ( 'NONE', *, *, #1792, .F. ) ;
#73762 = CONICAL_SURFACE ( 'NONE', #42493, 0.1000000000000002554, 0.003490658503988666988 ) ;
#73763 = ORIENTED_EDGE ( 'NONE', *, *, #28279, .F. ) ;
#73764 = DIRECTION ( 'NONE',  ( 0.000000000000000000, 0.000000000000000000, 1.000000000000000000 ) ) ;
#73765 = DIRECTION ( 'NONE',  ( -0.000000000000000000, -1.000000000000000000, -0.000000000000000000 ) ) ;
#73766 = EDGE_CURVE ( 'NONE', #105454, #37559, #38684, .T. ) ;
#73767 = EDGE_CURVE ( 'NONE', #8482, #71296, #97570, .T. ) ;
#73768 = CARTESIAN_POINT ( 'NONE',  ( 0.3999999999999568345, 12.50000000000000000, -5.022947341949754119 ) ) ;
#73769 = EDGE_CURVE ( 'NONE', #49114, #12584, #101940, .T. ) ;
#73770 = CARTESIAN_POINT ( 'NONE',  ( 7.049999999999928768, 2.500000000000000000, -2.165063509461101710 ) ) ;
#73771 = EDGE_CURVE ( 'NONE', #2492, #110412, #68106, .T. ) ;
#73772 = DIRECTION ( 'NONE',  ( -0.000000000000000000, -1.000000000000000000, -0.000000000000000000 ) ) ;
#73773 = AXIS2_PLACEMENT_3D ( 'NONE', #26074, #117000, #5125 ) ;
#73774 = VERTEX_POINT ( 'NONE', #47847 ) ;
#73775 = EDGE_LOOP ( 'NONE', ( #47289, #129278 ) ) ;
#73776 = DIRECTION ( 'NONE',  ( 0.000000000000000000, 0.000000000000000000, -1.000000000000000000 ) ) ;
#73778 = CIRCLE ( 'NONE', #71738, 0.06509327318403745899 ) ;
#73777 = DIRECTION ( 'NONE',  ( 0.000000000000000000, -1.000000000000000000, 0.000000000000000000 ) ) ;
#73779 = CONICAL_SURFACE ( 'NONE', #86287, 0.1000000000000002554, 0.003490658503988666988 ) ;
#73780 = DIRECTION ( 'NONE',  ( 0.000000000000000000, 0.000000000000000000, 1.000000000000000000 ) ) ;
#73781 = ORIENTED_EDGE ( 'NONE', *, *, #11695, .F. ) ;
#73782 = EDGE_LOOP ( 'NONE', ( #127578, #66392 ) ) ;
#73783 = EDGE_CURVE ( 'NONE', #44204, #125682, #102035, .T. ) ;
#73784 = DIRECTION ( 'NONE',  ( -0.000000000000000000, 1.000000000000000000, -0.000000000000000000 ) ) ;
#73785 = VECTOR ( 'NONE', #120901, 1000.000000000000000 ) ;
#73786 = ORIENTED_EDGE ( 'NONE', *, *, #19400, .T. ) ;
#73787 = CARTESIAN_POINT ( 'NONE',  ( -3.100000000000028955, 2.500000000000000000, 3.983716857408420964 ) ) ;
#73788 = LINE ( 'NONE', #103907, #40673 ) ;
#73789 = VERTEX_POINT ( 'NONE', #28847 ) ;
#73790 = AXIS2_PLACEMENT_3D ( 'NONE', #77135, #36587, #39172 ) ;
#73791 = CARTESIAN_POINT ( 'NONE',  ( -6.650000000000018119, 2.500000000000000000, -6.495190528383302464 ) ) ;
#73792 = DIRECTION ( 'NONE',  ( 0.000000000000000000, -0.000000000000000000, 1.000000000000000000 ) ) ;
#73793 = PLANE ( 'NONE',  #126221 ) ;
#73794 = CARTESIAN_POINT ( 'NONE',  ( 14.34999999999989662, 12.50000000000000000, 1.883746621131358934 ) ) ;
#73795 = ORIENTED_EDGE ( 'NONE', *, *, #55250, .T. ) ;
#73796 = CARTESIAN_POINT ( 'NONE',  ( -5.400000000000019895, 2.500000000000000000, -0.7928203230275542301 ) ) ;
#73797 = CARTESIAN_POINT ( 'NONE',  ( 35.04009662963670735, -1.562391656607243329, 4.793251516052316141 ) ) ;
#73798 = ORIENTED_EDGE ( 'NONE', *, *, #78583, .F. ) ;
#73799 = ORIENTED_EDGE ( 'NONE', *, *, #123589, .T. ) ;
#73800 = CONICAL_SURFACE ( 'NONE', #31969, 0.1000000000000002554, 0.003490658503988666988 ) ;
#73802 = ADVANCED_FACE ( 'NONE', ( #48478 ), #41405, .T. ) ;
#73801 = AXIS2_PLACEMENT_3D ( 'NONE', #115173, #25518, #83804 ) ;
#73803 = CARTESIAN_POINT ( 'NONE',  ( 183.9427083336747160, -6.551208109652278289, 3.782341765624995134 ) ) ;
#73804 = DIRECTION ( 'NONE',  ( -0.000000000000000000, 1.000000000000000000, -0.000000000000000000 ) ) ;
#73805 = DIRECTION ( 'NONE',  ( -0.000000000000000000, 1.000000000000000000, -0.000000000000000000 ) ) ;
#73806 = DIRECTION ( 'NONE',  ( 0.000000000000000000, 0.000000000000000000, -1.000000000000000000 ) ) ;
#73807 = CARTESIAN_POINT ( 'NONE',  ( 9.599999999999917932, 2.500000000000000000, -0.5928203230275541635 ) ) ;
#73808 = AXIS2_PLACEMENT_3D ( 'NONE', #6856, #87367, #108304 ) ;
#73809 = DIRECTION ( 'NONE',  ( -0.000000000000000000, 1.000000000000000000, -0.000000000000000000 ) ) ;
#73810 = DIRECTION ( 'NONE',  ( -0.000000000000000000, 1.000000000000000000, -0.000000000000000000 ) ) ;
#73811 = AXIS2_PLACEMENT_3D ( 'NONE', #71982, #11756, #119777 ) ;
#73812 = DIRECTION ( 'NONE',  ( 0.000000000000000000, 1.000000000000000000, 0.000000000000000000 ) ) ;
#73813 = FACE_OUTER_BOUND ( 'NONE', #91140, .T. ) ;
#73815 = CIRCLE ( 'NONE', #115560, 0.06509327318403745899 ) ;
#73814 = DIRECTION ( 'NONE',  ( 0.000000000000000000, 0.000000000000000000, 1.000000000000000000 ) ) ;
#73817 = EDGE_CURVE ( 'NONE', #96053, #60531, #30939, .T. ) ;
#73816 = CONICAL_SURFACE ( 'NONE', #46628, 0.1000000000000000472, 0.003490658503988666988 ) ;
#73818 = ADVANCED_FACE ( 'NONE', ( #98857 ), #12129, .T. ) ;
#73819 = EDGE_CURVE ( 'NONE', #43127, #27663, #78604, .T. ) ;
#73820 = DIRECTION ( 'NONE',  ( 0.000000000000000000, 0.000000000000000000, -1.000000000000000000 ) ) ;
#73821 = ORIENTED_EDGE ( 'NONE', *, *, #116654, .F. ) ;
#73822 = VECTOR ( 'NONE', #20401, 1000.000000000000000 ) ;
#73823 = VERTEX_POINT ( 'NONE', #117181 ) ;
#73824 = CONICAL_SURFACE ( 'NONE', #61315, 0.1000000000000000472, 0.003490658503988666988 ) ;
#73825 = EDGE_CURVE ( 'NONE', #37559, #116756, #114534, .T. ) ;
#73826 = CONICAL_SURFACE ( 'NONE', #69622, 0.1000000000000002554, 0.003490658503988666988 ) ;
#73827 = EDGE_LOOP ( 'NONE', ( #55650, #47510, #90060, #2559 ) ) ;
#73828 = VECTOR ( 'NONE', #102586, 1000.000000000000000 ) ;
#73829 = ADVANCED_FACE ( 'NONE', ( #75998 ), #115925, .T. ) ;
#73830 = ORIENTED_EDGE ( 'NONE', *, *, #5937, .F. ) ;
#73831 = EDGE_CURVE ( 'NONE', #79117, #18510, #120810, .T. ) ;
#73832 = CARTESIAN_POINT ( 'NONE',  ( 13.09999999999989839, 2.500000000000000000, 0.3464101615137735735 ) ) ;
#73833 = PLANE ( 'NONE',  #72964 ) ;
#73834 = CONICAL_SURFACE ( 'NONE', #117727, 0.09999999999999982514, 0.003490658503988666988 ) ;
#73835 = EDGE_CURVE ( 'NONE', #5090, #38024, #66423, .T. ) ;
#73836 = ORIENTED_EDGE ( 'NONE', *, *, #14908, .F. ) ;
#73837 = ADVANCED_FACE ( 'NONE', ( #11113 ), #89418, .T. ) ;
#73838 = CARTESIAN_POINT ( 'NONE',  ( 1.449999999999951328, 12.50000000000000000, -1.818653347947326138 ) ) ;
#73839 = EDGE_CURVE ( 'NONE', #50581, #128585, #20952, .T. ) ;
#73840 = FACE_OUTER_BOUND ( 'NONE', #106382, .T. ) ;
#73842 = VERTEX_POINT ( 'NONE', #59616 ) ;
#73841 = DIRECTION ( 'NONE',  ( -0.000000000000000000, -1.000000000000000000, -0.000000000000000000 ) ) ;
#73843 = FACE_OUTER_BOUND ( 'NONE', #118726, .T. ) ;
#73844 = EDGE_CURVE ( 'NONE', #77757, #128842, #76897, .T. ) ;
#73845 = CARTESIAN_POINT ( 'NONE',  ( 13.34999999999989662, 12.50000000000000000, -2.922977105672691422 ) ) ;
#73846 = ORIENTED_EDGE ( 'NONE', *, *, #86803, .F. ) ;
#73847 = VERTEX_POINT ( 'NONE', #101449 ) ;
#73848 = ORIENTED_EDGE ( 'NONE', *, *, #14574, .T. ) ;
#73849 = ORIENTED_EDGE ( 'NONE', *, *, #66943, .F. ) ;
#73850 = CARTESIAN_POINT ( 'NONE',  ( 4.149999999999941735, 2.500000000000000000, -1.572243186433550211 ) ) ;
#73851 = DIRECTION ( 'NONE',  ( -0.000000000000000000, -1.000000000000000000, -0.000000000000000000 ) ) ;
#73852 = CARTESIAN_POINT ( 'NONE',  ( 12.69999999999989981, 12.50000000000000000, -0.3464101615137783474 ) ) ;
#73853 = CARTESIAN_POINT ( 'NONE',  ( 11.04999999999990834, 12.50000000000000000, 1.818653347947321475 ) ) ;
#73854 = CIRCLE ( 'NONE', #59211, 0.06509327318403743123 ) ;
#73855 = VERTEX_POINT ( 'NONE', #9841 ) ;
#73856 = CARTESIAN_POINT ( 'NONE',  ( -7.500000000000013323, 2.500000000000000000, 4.922947341949748257 ) ) ;
#73857 = ORIENTED_EDGE ( 'NONE', *, *, #73186, .F. ) ;
#73858 = CARTESIAN_POINT ( 'NONE',  ( -3.950000000000024603, 2.500000000000000000, -2.511473670974877948 ) ) ;
#73859 = CARTESIAN_POINT ( 'NONE',  ( 10.04522989421447043, -2.499999999999999556, -8.164691043409833426 ) ) ;
#73860 = DIRECTION ( 'NONE',  ( -4.274815082592931898E-19, -0.9999939076577903929, -0.003490651415223739937 ) ) ;
#73861 = LINE ( 'NONE', #43783, #119544 ) ;
#73862 = EDGE_CURVE ( 'NONE', #15192, #10596, #45609, .T. ) ;
#73863 = AXIS2_PLACEMENT_3D ( 'NONE', #24145, #83712, #33339 ) ;
#73864 = AXIS2_PLACEMENT_3D ( 'NONE', #86178, #44340, #114367 ) ;
#73865 = CIRCLE ( 'NONE', #67588, 0.06509327318403745899 ) ;
#73866 = ORIENTED_EDGE ( 'NONE', *, *, #12141, .T. ) ;
#73867 = AXIS2_PLACEMENT_3D ( 'NONE', #99293, #64823, #128104 ) ;
#73868 = VERTEX_POINT ( 'NONE', #1940 ) ;
#73869 = VERTEX_POINT ( 'NONE', #81165 ) ;
#73870 = DIRECTION ( 'NONE',  ( 0.000000000000000000, -0.9999939076577903929, 0.003490651415223739937 ) ) ;
#73871 = DIRECTION ( 'NONE',  ( 0.000000000000000000, -0.000000000000000000, 1.000000000000000000 ) ) ;
#73872 = DIRECTION ( 'NONE',  ( 0.000000000000000000, 0.000000000000000000, 1.000000000000000000 ) ) ;
#73873 = FACE_BOUND ( 'NONE', #54097, .T. ) ;
#73874 = AXIS2_PLACEMENT_3D ( 'NONE', #88382, #27530, #106742 ) ;
#73875 = CARTESIAN_POINT ( 'NONE',  ( -0.8500000000000386136, 2.500000000000000000, 7.188010851410848723 ) ) ;
#73876 = DIRECTION ( 'NONE',  ( 0.000000000000000000, -0.000000000000000000, 1.000000000000000000 ) ) ;
#73877 = LINE ( 'NONE', #113811, #70852 ) ;
#73878 = ADVANCED_FACE ( 'NONE', ( #11769 ), #72698, .T. ) ;
#73879 = VECTOR ( 'NONE', #10146, 1000.000000000000000 ) ;
#73880 = AXIS2_PLACEMENT_3D ( 'NONE', #14060, #114222, #85403 ) ;
#73881 = AXIS2_PLACEMENT_3D ( 'NONE', #21454, #101317, #51576 ) ;
#73882 = DIRECTION ( 'NONE',  ( -0.000000000000000000, -1.000000000000000000, -0.000000000000000000 ) ) ;
#73883 = DIRECTION ( 'NONE',  ( 0.000000000000000000, 1.000000000000000000, 0.000000000000000000 ) ) ;
#73884 = AXIS2_PLACEMENT_3D ( 'NONE', #87412, #99839, #7562 ) ;
#73885 = DIRECTION ( 'NONE',  ( -0.000000000000000000, 1.000000000000000000, -0.000000000000000000 ) ) ;
#73886 = VERTEX_POINT ( 'NONE', #120443 ) ;
#73887 = DIRECTION ( 'NONE',  ( 0.000000000000000000, -0.9999939076577903929, 0.003490651415223739937 ) ) ;
#73888 = ORIENTED_EDGE ( 'NONE', *, *, #80038, .T. ) ;
#73889 = ORIENTED_EDGE ( 'NONE', *, *, #64167, .T. ) ;
#73890 = ORIENTED_EDGE ( 'NONE', *, *, #119168, .F. ) ;
#73891 = ORIENTED_EDGE ( 'NONE', *, *, #54505, .T. ) ;
#73892 = EDGE_CURVE ( 'NONE', #74692, #115125, #93624, .T. ) ;
#73893 = DIRECTION ( 'NONE',  ( 0.000000000000000000, 1.000000000000000000, 0.000000000000000000 ) ) ;
#73894 = FACE_BOUND ( 'NONE', #98339, .T. ) ;
#73895 = DIRECTION ( 'NONE',  ( 0.000000000000000000, 0.000000000000000000, 1.000000000000000000 ) ) ;
#73897 = VERTEX_POINT ( 'NONE', #89690 ) ;
#73896 = AXIS2_PLACEMENT_3D ( 'NONE', #67992, #69274, #107924 ) ;
#73899 = AXIS2_PLACEMENT_3D ( 'NONE', #80447, #41186, #121005 ) ;
#73898 = DIRECTION ( 'NONE',  ( 0.000000000000000000, 0.000000000000000000, 1.000000000000000000 ) ) ;
#73900 = DIRECTION ( 'NONE',  ( 0.000000000000000000, 1.000000000000000000, 0.000000000000000000 ) ) ;
#73901 = ORIENTED_EDGE ( 'NONE', *, *, #118102, .F. ) ;
#73902 = DIRECTION ( 'NONE',  ( -0.000000000000000000, 1.000000000000000000, -0.000000000000000000 ) ) ;
#73903 = DIRECTION ( 'NONE',  ( -0.000000000000000000, -1.000000000000000000, -0.000000000000000000 ) ) ;
#73904 = CIRCLE ( 'NONE', #38323, 0.06509327318403745899 ) ;
#73905 = AXIS2_PLACEMENT_3D ( 'NONE', #100845, #44352, #104565 ) ;
#73906 = CIRCLE ( 'NONE', #67639, 0.06509327318403745899 ) ;
#73907 = AXIS2_PLACEMENT_3D ( 'NONE', #35163, #105819, #75071 ) ;
#73908 = AXIS2_PLACEMENT_3D ( 'NONE', #51309, #81405, #121312 ) ;
#73909 = EDGE_LOOP ( 'NONE', ( #88504, #16051, #116994, #79423 ) ) ;
#73910 = DIRECTION ( 'NONE',  ( 0.000000000000000000, 0.000000000000000000, -1.000000000000000000 ) ) ;
#73911 = DIRECTION ( 'NONE',  ( 0.000000000000000000, -0.000000000000000000, 1.000000000000000000 ) ) ;
#73912 = AXIS2_PLACEMENT_3D ( 'NONE', #45840, #85747, #36677 ) ;
#73914 = VERTEX_POINT ( 'NONE', #109327 ) ;
#73913 = AXIS2_PLACEMENT_3D ( 'NONE', #79432, #110800, #58509 ) ;
#73916 = ADVANCED_FACE ( 'NONE', ( #79239 ), #21597, .T. ) ;
#73915 = CIRCLE ( 'NONE', #2916, 0.1000000000000002554 ) ;
#73917 = DIRECTION ( 'NONE',  ( 0.000000000000000000, 0.000000000000000000, 1.000000000000000000 ) ) ;
#73918 = CARTESIAN_POINT ( 'NONE',  ( 5.649999999999934630, 2.500000000000000000, 6.841600689897072485 ) ) ;
#73919 = DIRECTION ( 'NONE',  ( -0.000000000000000000, -1.000000000000000000, -0.000000000000000000 ) ) ;
#73921 = ORIENTED_EDGE ( 'NONE', *, *, #102912, .F. ) ;
#73920 = AXIS2_PLACEMENT_3D ( 'NONE', #123081, #94906, #103443 ) ;
#73922 = ORIENTED_EDGE ( 'NONE', *, *, #73358, .T. ) ;
#73923 = CARTESIAN_POINT ( 'NONE',  ( 4.149999999999939959, 12.50000000000000000, -6.560283801567339701 ) ) ;
#73924 = EDGE_CURVE ( 'NONE', #11458, #87465, #32999, .T. ) ;
#73925 = ORIENTED_EDGE ( 'NONE', *, *, #77661, .T. ) ;
#73926 = DIRECTION ( 'NONE',  ( 0.000000000000000000, 0.000000000000000000, 1.000000000000000000 ) ) ;
#73927 = CARTESIAN_POINT ( 'NONE',  ( 8.349999999999923261, 2.500000000000000000, 1.472243186433545459 ) ) ;
#73928 = ORIENTED_EDGE ( 'NONE', *, *, #21191, .T. ) ;
#73929 = DIRECTION ( 'NONE',  ( -0.000000000000000000, -1.000000000000000000, -0.000000000000000000 ) ) ;
#73930 = DIRECTION ( 'NONE',  ( 0.000000000000000000, 1.000000000000000000, 0.000000000000000000 ) ) ;
#73931 = DIRECTION ( 'NONE',  ( 0.000000000000000000, 1.000000000000000000, 0.000000000000000000 ) ) ;
#73932 = ADVANCED_FACE ( 'NONE', ( #51075 ), #31047, .T. ) ;
#73933 = EDGE_CURVE ( 'NONE', #110796, #60290, #81788, .T. ) ;
#73934 = DIRECTION ( 'NONE',  ( 0.000000000000000000, 0.000000000000000000, 1.000000000000000000 ) ) ;
#73935 = EDGE_CURVE ( 'NONE', #107586, #91772, #22263, .T. ) ;
#73936 = EDGE_CURVE ( 'NONE', #91958, #56615, #119793, .T. ) ;
#73937 = ADVANCED_FACE ( 'NONE', ( #109982 ), #89051, .T. ) ;
#73938 = DIRECTION ( 'NONE',  ( 0.000000000000000000, 1.000000000000000000, 0.000000000000000000 ) ) ;
#73939 = CIRCLE ( 'NONE', #113753, 0.06509327318403745899 ) ;
#73940 = EDGE_LOOP ( 'NONE', ( #61563, #70087, #8260, #96022 ) ) ;
#73941 = VERTEX_POINT ( 'NONE', #119149 ) ;
#73942 = DIRECTION ( 'NONE',  ( 0.000000000000000000, 1.000000000000000000, 0.000000000000000000 ) ) ;
#73943 = DIRECTION ( 'NONE',  ( -4.274815082592931898E-19, -0.9999939076577903929, -0.003490651415223739937 ) ) ;
#73945 = ORIENTED_EDGE ( 'NONE', *, *, #44379, .F. ) ;
#73944 = ORIENTED_EDGE ( 'NONE', *, *, #113078, .T. ) ;
#73946 = EDGE_LOOP ( 'NONE', ( #5350, #22789 ) ) ;
#73947 = EDGE_CURVE ( 'NONE', #101350, #90163, #54008, .T. ) ;
#73948 = DIRECTION ( 'NONE',  ( 0.000000000000000000, 0.000000000000000000, -1.000000000000000000 ) ) ;
#73950 = EDGE_CURVE ( 'NONE', #48914, #57519, #79058, .T. ) ;
#73949 = CONICAL_SURFACE ( 'NONE', #94877, 0.1000000000000000472, 0.003490658503988666988 ) ;
#73951 = CARTESIAN_POINT ( 'NONE',  ( -0.4000000000000331624, 12.50000000000000000, -0.7579135962115893799 ) ) ;
#73952 = VECTOR ( 'NONE', #2359, 1000.000000000000000 ) ;
#73953 = EDGE_CURVE ( 'NONE', #96127, #70629, #68666, .T. ) ;
#73954 = DIRECTION ( 'NONE',  ( 0.000000000000000000, 0.000000000000000000, 1.000000000000000000 ) ) ;
#73955 = DIRECTION ( 'NONE',  ( 0.000000000000000000, 0.000000000000000000, 1.000000000000000000 ) ) ;
#73956 = CARTESIAN_POINT ( 'NONE',  ( 184.9895833340161175, -4.445597072760163471, -7.699999999999919353 ) ) ;
#73957 = CARTESIAN_POINT ( 'NONE',  ( 11.84999999999990372, 2.500000000000000000, -6.248780366869526759 ) ) ;
#73958 = FACE_OUTER_BOUND ( 'NONE', #16520, .T. ) ;
#73959 = CARTESIAN_POINT ( 'NONE',  ( -10.60000000000000320, 2.500000000000000000, -3.983716857408421852 ) ) ;
#73960 = AXIS2_PLACEMENT_3D ( 'NONE', #15354, #115490, #104404 ) ;
#73961 = FACE_OUTER_BOUND ( 'NONE', #74719, .T. ) ;
#73962 = VECTOR ( 'NONE', #4213, 1000.000000000000000 ) ;
#73963 = ORIENTED_EDGE ( 'NONE', *, *, #84611, .F. ) ;
#73964 = CONICAL_SURFACE ( 'NONE', #109565, 0.1000000000000002554, 0.003490658503988666988 ) ;
#73965 = FACE_OUTER_BOUND ( 'NONE', #51441, .T. ) ;
#73966 = ORIENTED_EDGE ( 'NONE', *, *, #123275, .T. ) ;
#73967 = VERTEX_POINT ( 'NONE', #22898 ) ;
#73968 = FACE_OUTER_BOUND ( 'NONE', #65386, .T. ) ;
#73970 = AXIS2_PLACEMENT_3D ( 'NONE', #8866, #29821, #59299 ) ;
#73969 = DIRECTION ( 'NONE',  ( -0.000000000000000000, -1.000000000000000000, -0.000000000000000000 ) ) ;
#73971 = DIRECTION ( 'NONE',  ( -0.000000000000000000, 1.000000000000000000, -0.000000000000000000 ) ) ;
#73972 = PLANE ( 'NONE',  #8538 ) ;
#73973 = CARTESIAN_POINT ( 'NONE',  ( -4.600000000000024514, 12.50000000000000000, 5.088040615133786027 ) ) ;
#73974 = AXIS2_PLACEMENT_3D ( 'NONE', #88511, #128471, #129122 ) ;
#73975 = DIRECTION ( 'NONE',  ( -0.000000000000000000, -1.000000000000000000, -0.000000000000000000 ) ) ;
#73976 = VECTOR ( 'NONE', #61762, 1000.000000000000000 ) ;
#73977 = CIRCLE ( 'NONE', #27911, 0.09999999999999982514 ) ;
#73978 = FACE_OUTER_BOUND ( 'NONE', #63389, .T. ) ;
#73979 = ORIENTED_EDGE ( 'NONE', *, *, #108801, .T. ) ;
#73980 = DIRECTION ( 'NONE',  ( -0.000000000000000000, -1.000000000000000000, -0.000000000000000000 ) ) ;
#73981 = AXIS2_PLACEMENT_3D ( 'NONE', #35605, #76814, #4825 ) ;
#73982 = AXIS2_PLACEMENT_3D ( 'NONE', #6095, #85941, #125871 ) ;
#73983 = CARTESIAN_POINT ( 'NONE',  ( 2.099999999999950351, 2.500000000000000000, -0.1000000000000022815 ) ) ;
#73984 = ORIENTED_EDGE ( 'NONE', *, *, #58306, .T. ) ;
#73985 = VERTEX_POINT ( 'NONE', #94849 ) ;
#73986 = ORIENTED_EDGE ( 'NONE', *, *, #113727, .T. ) ;
#73987 = EDGE_CURVE ( 'NONE', #72830, #17629, #70727, .T. ) ;
#73988 = ORIENTED_EDGE ( 'NONE', *, *, #40594, .F. ) ;
#73989 = LINE ( 'NONE', #113922, #98506 ) ;
#73990 = CARTESIAN_POINT ( 'NONE',  ( -11.89999999999999503, 12.50000000000000000, 4.611443907251934426 ) ) ;
#73991 = EDGE_CURVE ( 'NONE', #44948, #75085, #81201, .T. ) ;
#73992 = DIRECTION ( 'NONE',  ( -1.000000000000000000, -0.000000000000000000, -0.000000000000000000 ) ) ;
#73993 = CARTESIAN_POINT ( 'NONE',  ( 11.64999999999990443, 12.50000000000000000, -5.802370205355749988 ) ) ;
#73994 = EDGE_CURVE ( 'NONE', #117544, #33453, #120890, .T. ) ;
#73995 = CARTESIAN_POINT ( 'NONE',  ( 87.50000000000001421, 3.974992050023849810, 6.359987280038159163 ) ) ;
#73996 = ORIENTED_EDGE ( 'NONE', *, *, #42640, .T. ) ;
#73998 = CIRCLE ( 'NONE', #19619, 0.06509327318403745899 ) ;
#73997 = CARTESIAN_POINT ( 'NONE',  ( -11.89999999999999680, 2.500000000000000000, -3.983716857408423628 ) ) ;
#73999 = CIRCLE ( 'NONE', #48881, 0.06509327318403745899 ) ;
#74000 = LINE ( 'NONE', #15040, #13895 ) ;
#74001 = EDGE_CURVE ( 'NONE', #86001, #27095, #3825, .T. ) ;
#74002 = CARTESIAN_POINT ( 'NONE',  ( -5.400000000000020783, 2.500000000000000000, 0.7928203230275495672 ) ) ;
#74003 = EDGE_LOOP ( 'NONE', ( #75767, #1532 ) ) ;
#74004 = CIRCLE ( 'NONE', #92794, 0.09999999999999982514 ) ;
#74005 = AXIS2_PLACEMENT_3D ( 'NONE', #3636, #124706, #23261 ) ;
#74006 = VECTOR ( 'NONE', #61359, 1000.000000000000000 ) ;
#74007 = ORIENTED_EDGE ( 'NONE', *, *, #112691, .T. ) ;
#74008 = AXIS2_PLACEMENT_3D ( 'NONE', #82816, #13404, #61232 ) ;
#74009 = VERTEX_POINT ( 'NONE', #45113 ) ;
#74010 = DIRECTION ( 'NONE',  ( -0.000000000000000000, -1.000000000000000000, -0.000000000000000000 ) ) ;
#74011 = LINE ( 'NONE', #13133, #42592 ) ;
#74012 = CARTESIAN_POINT ( 'NONE',  ( -6.450000000000017941, 2.500000000000000000, -6.841600689897077814 ) ) ;
#74013 = AXIS2_PLACEMENT_3D ( 'NONE', #111173, #32012, #42476 ) ;
#74014 = CIRCLE ( 'NONE', #53086, 0.1000000000000002554 ) ;
#74015 = VECTOR ( 'NONE', #70835, 1000.000000000000000 ) ;
#74016 = AXIS2_PLACEMENT_3D ( 'NONE', #40520, #11015, #31338 ) ;
#74017 = ORIENTED_EDGE ( 'NONE', *, *, #119037, .T. ) ;
#74018 = DIRECTION ( 'NONE',  ( -0.000000000000000000, -1.000000000000000000, -0.000000000000000000 ) ) ;
#74019 = DIRECTION ( 'NONE',  ( -0.000000000000000000, -1.000000000000000000, -0.000000000000000000 ) ) ;
#74020 = CARTESIAN_POINT ( 'NONE',  ( -14.99999999999998224, 12.50000000000000000, -0.6928203230275519209 ) ) ;
#74021 = EDGE_CURVE ( 'NONE', #54678, #116826, #4496, .T. ) ;
#74022 = CARTESIAN_POINT ( 'NONE',  ( 7.299999999999926104, 2.500000000000000000, -3.883716857408426648 ) ) ;
#74023 = CARTESIAN_POINT ( 'NONE',  ( 9.149999999999916866, 12.50000000000000000, 7.253104124594885960 ) ) ;
#74024 = CIRCLE ( 'NONE', #107474, 0.06509327318403741736 ) ;
#74025 = VERTEX_POINT ( 'NONE', #52342 ) ;
#74026 = ORIENTED_EDGE ( 'NONE', *, *, #8457, .T. ) ;
#74027 = CARTESIAN_POINT ( 'NONE',  ( -6.450000000000019718, 2.500000000000000000, -1.918653347947326004 ) ) ;
#74028 = DIRECTION ( 'NONE',  ( 0.000000000000000000, 1.000000000000000000, 0.000000000000000000 ) ) ;
#74029 = DIRECTION ( 'NONE',  ( 0.000000000000000000, 0.000000000000000000, -1.000000000000000000 ) ) ;
#74030 = VECTOR ( 'NONE', #67854, 1000.000000000000000 ) ;
#74031 = DIRECTION ( 'NONE',  ( -0.000000000000000000, -1.000000000000000000, -0.000000000000000000 ) ) ;
#74032 = FACE_OUTER_BOUND ( 'NONE', #91957, .T. ) ;
#74033 = EDGE_LOOP ( 'NONE', ( #42623, #39106, #64458, #73589 ) ) ;
#74034 = EDGE_CURVE ( 'NONE', #116188, #59835, #122823, .T. ) ;
#74035 = ORIENTED_EDGE ( 'NONE', *, *, #25800, .F. ) ;
#74036 = CARTESIAN_POINT ( 'NONE',  ( -11.84999999999999787, 2.500000000000000000, -1.718653347947321830 ) ) ;
#74037 = CARTESIAN_POINT ( 'NONE',  ( 11.84999999999990727, 12.50000000000000000, 6.148780366869520009 ) ) ;
#74038 = DIRECTION ( 'NONE',  ( 0.000000000000000000, -0.000000000000000000, 1.000000000000000000 ) ) ;
#74039 = CARTESIAN_POINT ( 'NONE',  ( 3.099999999999945022, 2.500000000000000000, -4.776537180435978414 ) ) ;
#74040 = ORIENTED_EDGE ( 'NONE', *, *, #81372, .F. ) ;
#74041 = CIRCLE ( 'NONE', #94976, 0.09999999999999999167 ) ;
#74042 = CIRCLE ( 'NONE', #94879, 0.06509327318403745899 ) ;
#74043 = DIRECTION ( 'NONE',  ( 0.000000000000000000, 0.000000000000000000, -1.000000000000000000 ) ) ;
#74044 = DIRECTION ( 'NONE',  ( 0.000000000000000000, 1.846105847067148022E-16, -1.000000000000000000 ) ) ;
#74045 = VERTEX_POINT ( 'NONE', #93562 ) ;
#74046 = DIRECTION ( 'NONE',  ( -0.000000000000000000, -1.000000000000000000, -0.000000000000000000 ) ) ;
#74047 = EDGE_CURVE ( 'NONE', #10609, #70290, #47751, .T. ) ;
#74048 = ORIENTED_EDGE ( 'NONE', *, *, #128158, .F. ) ;
#74049 = CARTESIAN_POINT ( 'NONE',  ( 12.89999999999990088, 2.500000000000000000, -4.330127018922201643 ) ) ;
#74050 = CIRCLE ( 'NONE', #42784, 0.06509327318403741736 ) ;
#74051 = ORIENTED_EDGE ( 'NONE', *, *, #107820, .F. ) ;
#74052 = CARTESIAN_POINT ( 'NONE',  ( -0.8500000000000382805, 2.500000000000000000, -7.188010851410854052 ) ) ;
#74053 = DIRECTION ( 'NONE',  ( 0.000000000000000000, 0.000000000000000000, 1.000000000000000000 ) ) ;
#74054 = ORIENTED_EDGE ( 'NONE', *, *, #13238, .F. ) ;
#74055 = VERTEX_POINT ( 'NONE', #24175 ) ;
#74056 = CARTESIAN_POINT ( 'NONE',  ( 187.1302083336747444, -4.367472073101514418, -7.564683531250002702 ) ) ;
#74057 = CARTESIAN_POINT ( 'NONE',  ( 4.799999999999937650, 2.500000000000000000, -3.883716857408426648 ) ) ;
#74058 = CARTESIAN_POINT ( 'NONE',  ( 186.1302083336747444, -4.367472073101514418, -7.564683531250002702 ) ) ;
#74059 = DIRECTION ( 'NONE',  ( 0.000000000000000000, 0.000000000000000000, -1.000000000000000000 ) ) ;
#74060 = AXIS2_PLACEMENT_3D ( 'NONE', #114595, #94978, #106080 ) ;
#74061 = AXIS2_PLACEMENT_3D ( 'NONE', #99645, #108797, #8023 ) ;
#74062 = CARTESIAN_POINT ( 'NONE',  ( 9.599999999999917932, 2.500000000000000000, -0.1000000000000022815 ) ) ;
#74063 = CARTESIAN_POINT ( 'NONE',  ( 1.649999999999951505, 2.500000000000000000, -1.572243186433550211 ) ) ;
#74064 = DIRECTION ( 'NONE',  ( 0.000000000000000000, 0.000000000000000000, 1.000000000000000000 ) ) ;
#74065 = AXIS2_PLACEMENT_3D ( 'NONE', #115250, #25600, #105471 ) ;
#74066 = CARTESIAN_POINT ( 'NONE',  ( -5.600000000000020073, 2.500000000000000000, 0.3464101615137736845 ) ) ;
#74067 = VECTOR ( 'NONE', #36394, 1000.000000000000000 ) ;
#74068 = ORIENTED_EDGE ( 'NONE', *, *, #102902, .F. ) ;
#74070 = VERTEX_POINT ( 'NONE', #83741 ) ;
#74069 = ADVANCED_FACE ( 'NONE', ( #53636 ), #5865, .T. ) ;
#74071 = DIRECTION ( 'NONE',  ( 0.000000000000000000, 0.000000000000000000, -1.000000000000000000 ) ) ;
#74072 = DIRECTION ( 'NONE',  ( -0.000000000000000000, 1.000000000000000000, -0.000000000000000000 ) ) ;
#74073 = CARTESIAN_POINT ( 'NONE',  ( 7.099999999999926814, 12.50000000000000000, -0.06509327318403970719 ) ) ;
#74074 = CARTESIAN_POINT ( 'NONE',  ( 7.099999999999927702, 2.500000000000000000, -3.737306695894649700 ) ) ;
#74076 = ORIENTED_EDGE ( 'NONE', *, *, #29472, .T. ) ;
#74075 = ORIENTED_EDGE ( 'NONE', *, *, #60271, .T. ) ;
#74077 = FACE_BOUND ( 'NONE', #36130, .T. ) ;
#74078 = ORIENTED_EDGE ( 'NONE', *, *, #47335, .T. ) ;
#74079 = DIRECTION ( 'NONE',  ( -0.000000000000000000, 1.000000000000000000, -0.000000000000000000 ) ) ;
#74080 = DIRECTION ( 'NONE',  ( 0.000000000000000000, 0.000000000000000000, 1.000000000000000000 ) ) ;
#74081 = ORIENTED_EDGE ( 'NONE', *, *, #65085, .F. ) ;
#74083 = EDGE_CURVE ( 'NONE', #114265, #1501, #64457, .T. ) ;
#74082 = DIRECTION ( 'NONE',  ( -0.000000000000000000, -1.000000000000000000, -0.000000000000000000 ) ) ;
#74084 = DIRECTION ( 'NONE',  ( 0.000000000000000000, -0.9999939076577903929, 0.003490651415223739937 ) ) ;
#74085 = CARTESIAN_POINT ( 'NONE',  ( 1.249999999999986899, 12.50000000000000000, 6.495190528383297135 ) ) ;
#74087 = DIRECTION ( 'NONE',  ( 0.000000000000000000, 0.000000000000000000, 1.000000000000000000 ) ) ;
#74086 = CONICAL_SURFACE ( 'NONE', #57359, 0.1000000000000002554, 0.003490658503988666988 ) ;
#74088 = CIRCLE ( 'NONE', #17638, 0.1000000000000002554 ) ;
#74089 = DIRECTION ( 'NONE',  ( 0.000000000000000000, 0.000000000000000000, -1.000000000000000000 ) ) ;
#74090 = LINE ( 'NONE', #125126, #45331 ) ;
#74091 = CIRCLE ( 'NONE', #48967, 0.09999999999999982514 ) ;
#74092 = EDGE_CURVE ( 'NONE', #86121, #44827, #85394, .T. ) ;
#74093 = CIRCLE ( 'NONE', #34404, 0.09999999999999982514 ) ;
#74094 = EDGE_CURVE ( 'NONE', #29442, #44638, #92256, .T. ) ;
#74095 = CARTESIAN_POINT ( 'NONE',  ( 185.9010416670080303, -4.367472073101520635, 7.564683531249999149 ) ) ;
#74096 = DIRECTION ( 'NONE',  ( -4.274815082592931898E-19, -0.9999939076577903929, -0.003490651415223739937 ) ) ;
#74097 = EDGE_CURVE ( 'NONE', #33468, #78082, #72785, .T. ) ;
#74098 = ADVANCED_FACE ( 'NONE', ( #3250 ), #74934, .T. ) ;
#74099 = CARTESIAN_POINT ( 'NONE',  ( -3.100000000000028955, 2.500000000000000000, 3.983716857408420964 ) ) ;
#74100 = EDGE_LOOP ( 'NONE', ( #80798, #32423 ) ) ;
#74101 = VERTEX_POINT ( 'NONE', #23521 ) ;
#74102 = ORIENTED_EDGE ( 'NONE', *, *, #57071, .T. ) ;
#74104 = DIRECTION ( 'NONE',  ( 0.000000000000000000, 0.000000000000000000, 1.000000000000000000 ) ) ;
#74103 = CONICAL_SURFACE ( 'NONE', #13446, 0.09999999999999999167, 0.003490658503988666988 ) ;
#74105 = EDGE_LOOP ( 'NONE', ( #74547, #6736, #28455, #97750 ) ) ;
#74106 = ADVANCED_FACE ( 'NONE', ( #124310 ), #91653, .T. ) ;
#74109 = ORIENTED_EDGE ( 'NONE', *, *, #6716, .T. ) ;
#74108 = ORIENTED_EDGE ( 'NONE', *, *, #4546, .F. ) ;
#74107 = ADVANCED_FACE ( 'NONE', ( #37853 ), #125099, .T. ) ;
#74110 = ORIENTED_EDGE ( 'NONE', *, *, #88354, .T. ) ;
#74111 = EDGE_CURVE ( 'NONE', #58932, #868, #108376, .T. ) ;
#74112 = DIRECTION ( 'NONE',  ( 0.000000000000000000, -0.9999939076577903929, 0.003490651415223739937 ) ) ;
#74113 = ADVANCED_FACE ( 'NONE', ( #35923 ), #45694, .T. ) ;
#74114 = CIRCLE ( 'NONE', #118004, 0.06509327318403745899 ) ;
#74115 = AXIS2_PLACEMENT_3D ( 'NONE', #86282, #24808, #5153 ) ;
#74116 = EDGE_CURVE ( 'NONE', #82725, #93012, #62428, .T. ) ;
#74117 = CARTESIAN_POINT ( 'NONE',  ( -8.950000000000008171, 2.500000000000000000, 1.818653347947321475 ) ) ;
#74118 = PRESENTATION_STYLE_ASSIGNMENT (( #104208 ) ) ;
#74119 = CARTESIAN_POINT ( 'NONE',  ( 11.44999999999990514, 12.50000000000000000, 2.446380397790835826 ) ) ;
#74120 = DIRECTION ( 'NONE',  ( 0.000000000000000000, 0.000000000000000000, 1.000000000000000000 ) ) ;
#74121 = CONICAL_SURFACE ( 'NONE', #21895, 0.09999999999999982514, 0.003490658503988666988 ) ;
#74122 = DIRECTION ( 'NONE',  ( -1.000000000000000000, -0.000000000000000000, -0.000000000000000000 ) ) ;
#74123 = ORIENTED_EDGE ( 'NONE', *, *, #60190, .F. ) ;
#74124 = EDGE_CURVE ( 'NONE', #71126, #117070, #118749, .T. ) ;
#74125 = DIRECTION ( 'NONE',  ( 0.000000000000000000, 1.000000000000000000, 0.000000000000000000 ) ) ;
#74126 = EDGE_LOOP ( 'NONE', ( #19123, #48299, #87638, #95952 ) ) ;
#74127 = ORIENTED_EDGE ( 'NONE', *, *, #124345, .F. ) ;
#74128 = ORIENTED_EDGE ( 'NONE', *, *, #21327, .F. ) ;
#74129 = CARTESIAN_POINT ( 'NONE',  ( -7.050000000000013145, 12.50000000000000000, 2.165063509461097713 ) ) ;
#74130 = ORIENTED_EDGE ( 'NONE', *, *, #69967, .T. ) ;
#74131 = ORIENTED_EDGE ( 'NONE', *, *, #16426, .F. ) ;
#74132 = EDGE_LOOP ( 'NONE', ( #27392, #7650 ) ) ;
#74133 = AXIS2_PLACEMENT_3D ( 'NONE', #48884, #60639, #28586 ) ;
#74134 = DIRECTION ( 'NONE',  ( 0.000000000000000000, 0.000000000000000000, 1.000000000000000000 ) ) ;
#74135 = DIRECTION ( 'NONE',  ( 0.000000000000000000, 0.000000000000000000, 1.000000000000000000 ) ) ;
#74136 = DIRECTION ( 'NONE',  ( 0.000000000000000000, 1.000000000000000000, 0.000000000000000000 ) ) ;
#74137 = DIRECTION ( 'NONE',  ( 0.000000000000000000, -0.9999939076577903929, 0.003490651415223739937 ) ) ;
#74138 = CARTESIAN_POINT ( 'NONE',  ( -3.750000000000031086, 2.500000000000000000, -5.802370205355749988 ) ) ;
#74139 = CARTESIAN_POINT ( 'NONE',  ( -5.600000000000020073, 2.500000000000000000, 4.776537180435972196 ) ) ;
#74140 = DIRECTION ( 'NONE',  ( -0.000000000000000000, -1.000000000000000000, -0.000000000000000000 ) ) ;
#74141 = CONICAL_SURFACE ( 'NONE', #105532, 0.09999999999999982514, 0.003490658503988666988 ) ;
#74142 = ORIENTED_EDGE ( 'NONE', *, *, #61719, .F. ) ;
#74143 = DIRECTION ( 'NONE',  ( 0.000000000000000000, 0.000000000000000000, 1.000000000000000000 ) ) ;
#74144 = VERTEX_POINT ( 'NONE', #65376 ) ;
#74145 = CARTESIAN_POINT ( 'NONE',  ( -6.505213034913026604E-15, 2.500000000000000000, 4.330127018922196314 ) ) ;
#74146 = VERTEX_POINT ( 'NONE', #16259 ) ;
#74147 = EDGE_LOOP ( 'NONE', ( #117244, #74479 ) ) ;
#74148 = CARTESIAN_POINT ( 'NONE',  ( -3.750000000000027978, 2.500000000000000000, 7.288010851410849256 ) ) ;
#74149 = CARTESIAN_POINT ( 'NONE',  ( 184.6927083336747160, 6.551208109652275624, -3.782341765624998686 ) ) ;
#74150 = CIRCLE ( 'NONE', #70039, 0.06509327318403745899 ) ;
#74151 = EDGE_CURVE ( 'NONE', #116013, #56139, #62327, .T. ) ;
#74152 = CARTESIAN_POINT ( 'NONE',  ( 11.24999999999991118, 12.50000000000000000, -2.922977105672691422 ) ) ;
#74154 = ADVANCED_FACE ( 'NONE', ( #16888 ), #56043, .T. ) ;
#74153 = CONICAL_SURFACE ( 'NONE', #126664, 0.1000000000000002554, 0.003490658503988666988 ) ;
#74155 = ORIENTED_EDGE ( 'NONE', *, *, #48853, .T. ) ;
#74156 = CARTESIAN_POINT ( 'NONE',  ( -3.749999999999994671, 2.500000000000000000, -6.495190528383302464 ) ) ;
#74157 = ORIENTED_EDGE ( 'NONE', *, *, #66047, .F. ) ;
#74158 = DIRECTION ( 'NONE',  ( -4.274815082592931898E-19, -0.9999939076577903929, -0.003490651415223739937 ) ) ;
#74159 = DIRECTION ( 'NONE',  ( -1.000000000000000000, -0.000000000000000000, -0.000000000000000000 ) ) ;
#74160 = DIRECTION ( 'NONE',  ( 0.000000000000000000, 0.000000000000000000, 1.000000000000000000 ) ) ;
#74161 = CARTESIAN_POINT ( 'NONE',  ( 7.699999999999925571, 12.50000000000000000, 3.983716857408420076 ) ) ;
#74162 = ADVANCED_FACE ( 'NONE', ( #67954 ), #97416, .T. ) ;
#74163 = CARTESIAN_POINT ( 'NONE',  ( 7.299999999999924327, 12.50000000000000000, 0.3464101615137735735 ) ) ;
#74164 = ORIENTED_EDGE ( 'NONE', *, *, #4353, .T. ) ;
#74165 = AXIS2_PLACEMENT_3D ( 'NONE', #82441, #100749, #50378 ) ;
#74166 = CIRCLE ( 'NONE', #26041, 0.06509327318403745899 ) ;
#74167 = AXIS2_PLACEMENT_3D ( 'NONE', #78607, #38014, #57664 ) ;
#74168 = ORIENTED_EDGE ( 'NONE', *, *, #61118, .T. ) ;
#74169 = CIRCLE ( 'NONE', #124344, 0.1000000000000000472 ) ;
#74170 = FACE_OUTER_BOUND ( 'NONE', #26701, .T. ) ;
#74171 = DIRECTION ( 'NONE',  ( 1.000000000000000000, 0.000000000000000000, 0.000000000000000000 ) ) ;
#74172 = CARTESIAN_POINT ( 'NONE',  ( 185.0885416670080872, -6.551208109652273848, -3.782341765625003571 ) ) ;
#74173 = LINE ( 'NONE', #45368, #9341 ) ;
#74174 = DIRECTION ( 'NONE',  ( 0.000000000000000000, 0.000000000000000000, 1.000000000000000000 ) ) ;
#74175 = DIRECTION ( 'NONE',  ( 0.000000000000000000, 0.000000000000000000, 1.000000000000000000 ) ) ;
#74176 = LINE ( 'NONE', #46013, #108162 ) ;
#74177 = EDGE_LOOP ( 'NONE', ( #65241, #104930 ) ) ;
#74178 = DIRECTION ( 'NONE',  ( 0.000000000000000000, 0.000000000000000000, 1.000000000000000000 ) ) ;
#74180 = DIRECTION ( 'NONE',  ( 0.000000000000000000, 0.000000000000000000, -1.000000000000000000 ) ) ;
#74179 = AXIS2_PLACEMENT_3D ( 'NONE', #57567, #26168, #97478 ) ;
#74181 = CARTESIAN_POINT ( 'NONE',  ( -12.49999999999999289, 2.500000000000000000, -0.7928203230275501223 ) ) ;
#74182 = CIRCLE ( 'NONE', #30282, 0.06509327318403745899 ) ;
#74183 = VERTEX_POINT ( 'NONE', #107240 ) ;
#74184 = CIRCLE ( 'NONE', #28215, 0.1000000000000002554 ) ;
#74185 = DIRECTION ( 'NONE',  ( 0.000000000000000000, 0.000000000000000000, 1.000000000000000000 ) ) ;
#74186 = EDGE_CURVE ( 'NONE', #72457, #128585, #39363, .T. ) ;
#74187 = AXIS2_PLACEMENT_3D ( 'NONE', #77651, #118231, #61754 ) ;
#74188 = AXIS2_PLACEMENT_3D ( 'NONE', #51718, #5808, #116413 ) ;
#74189 = ORIENTED_EDGE ( 'NONE', *, *, #45876, .T. ) ;
#74190 = VECTOR ( 'NONE', #112778, 1000.000000000000000 ) ;
#74191 = CARTESIAN_POINT ( 'NONE',  ( -8.100000000000013856, 2.500000000000000000, -0.2464101615137782308 ) ) ;
#74192 = AXIS2_PLACEMENT_3D ( 'NONE', #46971, #107811, #67200 ) ;
#74193 = ORIENTED_EDGE ( 'NONE', *, *, #25003, .F. ) ;
#74194 = DIRECTION ( 'NONE',  ( -0.000000000000000000, -1.000000000000000000, -0.000000000000000000 ) ) ;
#74195 = PLANE ( 'NONE',  #90566 ) ;
#74196 = CARTESIAN_POINT ( 'NONE',  ( 1.649999999999951505, 2.500000000000000000, 1.472243186433545459 ) ) ;
#74197 = EDGE_LOOP ( 'NONE', ( #35382, #20532 ) ) ;
#74198 = AXIS2_PLACEMENT_3D ( 'NONE', #105852, #34560, #24076 ) ;
#74199 = AXIS2_PLACEMENT_3D ( 'NONE', #66340, #57825, #85343 ) ;
#74200 = DIRECTION ( 'NONE',  ( -0.000000000000000000, 1.000000000000000000, -0.000000000000000000 ) ) ;
#74201 = DIRECTION ( 'NONE',  ( 0.000000000000000000, 0.000000000000000000, 1.000000000000000000 ) ) ;
#74202 = AXIS2_PLACEMENT_3D ( 'NONE', #15197, #45990, #114076 ) ;
#74203 = ADVANCED_FACE ( 'NONE', ( #126242 ), #116405, .T. ) ;
#74204 = EDGE_CURVE ( 'NONE', #112423, #87133, #128184, .T. ) ;
#74205 = VERTEX_POINT ( 'NONE', #78453 ) ;
#74206 = DIRECTION ( 'NONE',  ( 0.000000000000000000, 1.000000000000000000, 0.000000000000000000 ) ) ;
#74207 = ORIENTED_EDGE ( 'NONE', *, *, #41151, .F. ) ;
#74208 = EDGE_LOOP ( 'NONE', ( #24946, #68171, #10916, #37396 ) ) ;
#74209 = FACE_OUTER_BOUND ( 'NONE', #20991, .T. ) ;
#74210 = CARTESIAN_POINT ( 'NONE',  ( 9.349999999999919709, 2.500000000000000000, -6.941600689897078347 ) ) ;
#74211 = FACE_OUTER_BOUND ( 'NONE', #121692, .T. ) ;
#74212 = EDGE_CURVE ( 'NONE', #86058, #84876, #43557, .T. ) ;
#74213 = VERTEX_POINT ( 'NONE', #36595 ) ;
#74214 = LINE ( 'NONE', #93852, #124149 ) ;
#74215 = CARTESIAN_POINT ( 'NONE',  ( -4.150000000000025224, 2.500000000000000000, -1.472243186433550122 ) ) ;
#74216 = AXIS2_PLACEMENT_3D ( 'NONE', #11922, #124467, #51866 ) ;
#74217 = EDGE_LOOP ( 'NONE', ( #107600, #56425 ) ) ;
#74218 = LINE ( 'NONE', #114140, #119791 ) ;
#74219 = DIRECTION ( 'NONE',  ( 0.000000000000000000, -0.9999939076577903929, 0.003490651415223739937 ) ) ;
#74220 = CARTESIAN_POINT ( 'NONE',  ( 14.99999999999992895, 2.500000000000000000, -2.276824562219559311E-15 ) ) ;
#74221 = CARTESIAN_POINT ( 'NONE',  ( 4.349999999999938360, 2.500000000000000000, 1.818653347947321475 ) ) ;
#74222 = CARTESIAN_POINT ( 'NONE',  ( -12.49999999999995914, 2.500000000000000000, -4.330127018922198978 ) ) ;
#74223 = LINE ( 'NONE', #125254, #72369 ) ;
#74224 = DIRECTION ( 'NONE',  ( -0.000000000000000000, -1.000000000000000000, -0.000000000000000000 ) ) ;
#74225 = AXIS2_PLACEMENT_3D ( 'NONE', #29810, #127369, #69731 ) ;
#74226 = AXIS2_PLACEMENT_3D ( 'NONE', #39148, #128817, #107853 ) ;
#74227 = ORIENTED_EDGE ( 'NONE', *, *, #99876, .T. ) ;
#74228 = ORIENTED_EDGE ( 'NONE', *, *, #18874, .T. ) ;
#74229 = EDGE_LOOP ( 'NONE', ( #57021, #59987 ) ) ;
#74230 = VERTEX_POINT ( 'NONE', #105316 ) ;
#74231 = DIRECTION ( 'NONE',  ( -0.000000000000000000, -1.000000000000000000, -0.000000000000000000 ) ) ;
#74232 = DIRECTION ( 'NONE',  ( 0.000000000000000000, 1.000000000000000000, 0.000000000000000000 ) ) ;
#74233 = DIRECTION ( 'NONE',  ( -4.274815082592931898E-19, -0.9999939076577903929, -0.003490651415223739937 ) ) ;
#74234 = VERTEX_POINT ( 'NONE', #15623 ) ;
#74235 = FACE_BOUND ( 'NONE', #114935, .T. ) ;
#74236 = CARTESIAN_POINT ( 'NONE',  ( -13.09999999999999254, 2.500000000000000000, -0.3464101615137741286 ) ) ;
#74237 = CARTESIAN_POINT ( 'NONE',  ( -1.650000000000034772, 2.500000000000000000, 5.802370205355744659 ) ) ;
#74238 = AXIS2_PLACEMENT_3D ( 'NONE', #30261, #11226, #19098 ) ;
#74240 = EDGE_CURVE ( 'NONE', #118322, #53342, #76987, .T. ) ;
#74239 = FACE_OUTER_BOUND ( 'NONE', #107908, .T. ) ;
#74241 = CARTESIAN_POINT ( 'NONE',  ( -7.900000000000014566, 2.500000000000000000, -5.022947341949754119 ) ) ;
#74242 = AXIS2_PLACEMENT_3D ( 'NONE', #82459, #110605, #20942 ) ;
#74243 = DIRECTION ( 'NONE',  ( -0.000000000000000000, -1.000000000000000000, -0.000000000000000000 ) ) ;
#74244 = CARTESIAN_POINT ( 'NONE',  ( 12.49999999999990585, 2.500000000000000000, 3.637306695894644726 ) ) ;
#74245 = DIRECTION ( 'NONE',  ( 0.000000000000000000, 1.000000000000000000, 0.000000000000000000 ) ) ;
#74246 = CARTESIAN_POINT ( 'NONE',  ( 3.149999999999946176, 12.50000000000000000, -6.213873640053564351 ) ) ;
#74247 = EDGE_CURVE ( 'NONE', #118333, #7975, #85483, .T. ) ;
#74248 = DIRECTION ( 'NONE',  ( 0.000000000000000000, 1.000000000000000000, 0.000000000000000000 ) ) ;
#74249 = ADVANCED_FACE ( 'NONE', ( #46375 ), #26752, .T. ) ;
#74250 = DIRECTION ( 'NONE',  ( 0.000000000000000000, 0.000000000000000000, 1.000000000000000000 ) ) ;
#74251 = CONICAL_SURFACE ( 'NONE', #40919, 0.1000000000000002554, 0.003490658503988666988 ) ;
#74252 = ORIENTED_EDGE ( 'NONE', *, *, #99174, .F. ) ;
#74253 = EDGE_LOOP ( 'NONE', ( #67974, #104779 ) ) ;
#74254 = AXIS2_PLACEMENT_3D ( 'NONE', #89375, #119456, #29807 ) ;
#74255 = VERTEX_POINT ( 'NONE', #47046 ) ;
#74256 = ORIENTED_EDGE ( 'NONE', *, *, #25155, .F. ) ;
#74257 = ADVANCED_FACE ( 'NONE', ( #86955 ), #110526, .T. ) ;
#74258 = VERTEX_POINT ( 'NONE', #60731 ) ;
#74260 = ADVANCED_FACE ( 'NONE', ( #30636 ), #81287, .T. ) ;
#74259 = PLANE ( 'NONE',  #48519 ) ;
#74262 = VERTEX_POINT ( 'NONE', #31281 ) ;
#74261 = ADVANCED_FACE ( 'NONE', ( #100010 ), #24849, .T. ) ;
#74263 = ORIENTED_EDGE ( 'NONE', *, *, #107699, .T. ) ;
#74264 = EDGE_CURVE ( 'NONE', #108726, #69317, #16401, .T. ) ;
#74265 = FACE_OUTER_BOUND ( 'NONE', #40158, .T. ) ;
#74266 = FACE_OUTER_BOUND ( 'NONE', #71675, .T. ) ;
#74267 = LINE ( 'NONE', #35008, #124127 ) ;
#74268 = LINE ( 'NONE', #12264, #12060 ) ;
#74269 = EDGE_CURVE ( 'NONE', #65715, #116743, #51562, .T. ) ;
#74270 = AXIS2_PLACEMENT_3D ( 'NONE', #16300, #124989, #85058 ) ;
#74271 = ORIENTED_EDGE ( 'NONE', *, *, #77407, .T. ) ;
#74272 = DIRECTION ( 'NONE',  ( 0.000000000000000000, -0.000000000000000000, 1.000000000000000000 ) ) ;
#74273 = ADVANCED_FACE ( 'NONE', ( #120295 ), #114727, .T. ) ;
#74274 = VERTEX_POINT ( 'NONE', #91468 ) ;
#74276 = ORIENTED_EDGE ( 'NONE', *, *, #76607, .T. ) ;
#74275 = CONICAL_SURFACE ( 'NONE', #84727, 0.1000000000000002554, 0.003490658503988666988 ) ;
#74278 = EDGE_LOOP ( 'NONE', ( #22860, #58193, #122706, #21209 ) ) ;
#74277 = DIRECTION ( 'NONE',  ( -0.000000000000000000, -1.000000000000000000, -0.000000000000000000 ) ) ;
#74279 = AXIS2_PLACEMENT_3D ( 'NONE', #55321, #25857, #96501 ) ;
#74280 = CIRCLE ( 'NONE', #34586, 0.06509327318403745899 ) ;
#74281 = FACE_OUTER_BOUND ( 'NONE', #58590, .T. ) ;
#74282 = ORIENTED_EDGE ( 'NONE', *, *, #63013, .F. ) ;
#74283 = VERTEX_POINT ( 'NONE', #108533 ) ;
#74284 = DIRECTION ( 'NONE',  ( 0.000000000000000000, -0.9999939076577903929, 0.003490651415223739937 ) ) ;
#74285 = CONICAL_SURFACE ( 'NONE', #122405, 0.1000000000000002554, 0.003490658503988666988 ) ;
#74286 = CONICAL_SURFACE ( 'NONE', #55499, 0.1000000000000000056, 0.003490658503988666988 ) ;
#74287 = AXIS2_PLACEMENT_3D ( 'NONE', #117247, #1207, #7960 ) ;
#74288 = CARTESIAN_POINT ( 'NONE',  ( -6.650000000000018119, 2.500000000000000000, -6.395190528383301931 ) ) ;
#74289 = CARTESIAN_POINT ( 'NONE',  ( 11.24999999999994316, 2.500000000000000000, 2.265063509461097357 ) ) ;
#74290 = FACE_OUTER_BOUND ( 'NONE', #50434, .T. ) ;
#74291 = CIRCLE ( 'NONE', #91009, 0.06509327318403745899 ) ;
#74292 = CARTESIAN_POINT ( 'NONE',  ( 11.84999999999990727, 12.50000000000000000, 6.148780366869520009 ) ) ;
#74293 = ORIENTED_EDGE ( 'NONE', *, *, #99656, .F. ) ;
#74294 = DIRECTION ( 'NONE',  ( 0.000000000000000000, 0.000000000000000000, 1.000000000000000000 ) ) ;
#74295 = AXIS2_PLACEMENT_3D ( 'NONE', #94577, #23929, #42945 ) ;
#74296 = AXIS2_PLACEMENT_3D ( 'NONE', #83890, #61703, #62342 ) ;
#74297 = ORIENTED_EDGE ( 'NONE', *, *, #12576, .F. ) ;
#74298 = CARTESIAN_POINT ( 'NONE',  ( 87.50000000000002842, 7.032605354647521345, -2.693424153406288379 ) ) ;
#74299 = EDGE_LOOP ( 'NONE', ( #41390, #61757 ) ) ;
#74300 = FACE_OUTER_BOUND ( 'NONE', #2100, .T. ) ;
#74301 = DIRECTION ( 'NONE',  ( 0.000000000000000000, 0.000000000000000000, 1.000000000000000000 ) ) ;
#74302 = VECTOR ( 'NONE', #38095, 1000.000000000000000 ) ;
#74303 = DIRECTION ( 'NONE',  ( 0.000000000000000000, 1.000000000000000000, 0.000000000000000000 ) ) ;
#74304 = FACE_OUTER_BOUND ( 'NONE', #110839, .T. ) ;
#74305 = ORIENTED_EDGE ( 'NONE', *, *, #16438, .T. ) ;
#74306 = DIRECTION ( 'NONE',  ( 0.000000000000000000, 1.000000000000000000, 0.000000000000000000 ) ) ;
#74307 = ADVANCED_FACE ( 'NONE', ( #90826 ), #41107, .T. ) ;
#74308 = DIRECTION ( 'NONE',  ( -0.000000000000000000, 1.000000000000000000, -0.000000000000000000 ) ) ;
#74309 = ADVANCED_FACE ( 'NONE', ( #80378 ), #111084, .T. ) ;
#74310 = ORIENTED_EDGE ( 'NONE', *, *, #84906, .F. ) ;
#74311 = ORIENTED_EDGE ( 'NONE', *, *, #122403, .F. ) ;
#74312 = VERTEX_POINT ( 'NONE', #61377 ) ;
#74313 = CARTESIAN_POINT ( 'NONE',  ( -1.050000000000038680, 2.500000000000000000, 2.511473670974873507 ) ) ;
#74314 = FACE_OUTER_BOUND ( 'NONE', #125698, .T. ) ;
#74315 = CARTESIAN_POINT ( 'NONE',  ( 185.3593750003413732, 0.000000000000000000, 7.564683531250000925 ) ) ;
#74316 = AXIS2_PLACEMENT_3D ( 'NONE', #58316, #89691, #10476 ) ;
#74317 = FACE_OUTER_BOUND ( 'NONE', #69885, .T. ) ;
#74318 = CARTESIAN_POINT ( 'NONE',  ( 17.49862860983167323, 2.500000000000000000, -4.081131818001370704 ) ) ;
#74319 = DIRECTION ( 'NONE',  ( 0.000000000000000000, -0.9999939076577903929, 0.003490651415223739937 ) ) ;
#74320 = VERTEX_POINT ( 'NONE', #20156 ) ;
#74321 = AXIS2_PLACEMENT_3D ( 'NONE', #41710, #33181, #43014 ) ;
#74322 = DIRECTION ( 'NONE',  ( -0.000000000000000000, 1.000000000000000000, -0.000000000000000000 ) ) ;
#74323 = EDGE_LOOP ( 'NONE', ( #12032, #112967 ) ) ;
#74324 = DIRECTION ( 'NONE',  ( 0.000000000000000000, -0.000000000000000000, 1.000000000000000000 ) ) ;
#74325 = CARTESIAN_POINT ( 'NONE',  ( -8.300000000000011369, 2.500000000000000000, -0.1000000000000022815 ) ) ;
#74326 = LINE ( 'NONE', #3014, #89808 ) ;
#74327 = ORIENTED_EDGE ( 'NONE', *, *, #103913, .F. ) ;
#74328 = CIRCLE ( 'NONE', #47246, 0.06509327318403745899 ) ;
#74329 = VECTOR ( 'NONE', #70525, 1000.000000000000000 ) ;
#74330 = DIRECTION ( 'NONE',  ( -0.000000000000000000, 1.000000000000000000, -0.000000000000000000 ) ) ;
#74331 = LINE ( 'NONE', #103791, #92282 ) ;
#74332 = ORIENTED_EDGE ( 'NONE', *, *, #88023, .T. ) ;
#74333 = FACE_OUTER_BOUND ( 'NONE', #90030, .T. ) ;
#74334 = ADVANCED_FACE ( 'NONE', ( #48990 ), #93812, .T. ) ;
#74335 = CIRCLE ( 'NONE', #11643, 0.06509327318403745899 ) ;
#74336 = VECTOR ( 'NONE', #38860, 1000.000000000000000 ) ;
#74337 = VERTEX_POINT ( 'NONE', #9689 ) ;
#74338 = VERTEX_POINT ( 'NONE', #101303 ) ;
#74339 = LINE ( 'NONE', #53422, #123980 ) ;
#74340 = EDGE_LOOP ( 'NONE', ( #10285, #67930, #43939, #25351 ) ) ;
#74341 = CARTESIAN_POINT ( 'NONE',  ( 17.17161331427240256, 0.4678040054248072122, -5.513957101008877260 ) ) ;
#74342 = CARTESIAN_POINT ( 'NONE',  ( 10.19999999999991580, 2.500000000000000000, -0.2464101615137783419 ) ) ;
#74343 = DIRECTION ( 'NONE',  ( -0.000000000000000000, -1.000000000000000000, -0.000000000000000000 ) ) ;
#74344 = EDGE_CURVE ( 'NONE', #31556, #47635, #106325, .T. ) ;
#74345 = ORIENTED_EDGE ( 'NONE', *, *, #69687, .F. ) ;
#74346 = DIRECTION ( 'NONE',  ( 0.000000000000000000, 0.000000000000000000, 1.000000000000000000 ) ) ;
#74348 = ORIENTED_EDGE ( 'NONE', *, *, #1078, .F. ) ;
#74347 = FACE_OUTER_BOUND ( 'NONE', #103300, .T. ) ;
#74349 = EDGE_CURVE ( 'NONE', #77555, #47068, #75024, .T. ) ;
#74350 = CARTESIAN_POINT ( 'NONE',  ( 9.599999999999917932, 2.500000000000000000, -0.7928203230275542301 ) ) ;
#74351 = CARTESIAN_POINT ( 'NONE',  ( -10.65000000000000213, 2.500000000000000000, 6.148780366869520009 ) ) ;
#74352 = EDGE_CURVE ( 'NONE', #17807, #29513, #18589, .T. ) ;
#74353 = CIRCLE ( 'NONE', #91076, 0.1000000000000000472 ) ;
#74354 = VERTEX_POINT ( 'NONE', #128850 ) ;
#74355 = AXIS2_PLACEMENT_3D ( 'NONE', #28372, #87901, #95811 ) ;
#74356 = ORIENTED_EDGE ( 'NONE', *, *, #79204, .T. ) ;
#74357 = ADVANCED_FACE ( 'NONE', ( #39179 ), #37379, .T. ) ;
#74358 = VECTOR ( 'NONE', #31655, 1000.000000000000000 ) ;
#74359 = EDGE_LOOP ( 'NONE', ( #61564, #67470, #51082, #71129 ) ) ;
#74360 = CARTESIAN_POINT ( 'NONE',  ( -5.850000000000022737, 2.500000000000000000, -6.395190528383301931 ) ) ;
#74361 = DIRECTION ( 'NONE',  ( 0.000000000000000000, -0.9999939076577903929, 0.003490651415223739937 ) ) ;
#74362 = DIRECTION ( 'NONE',  ( 0.000000000000000000, 0.000000000000000000, 1.000000000000000000 ) ) ;
#74363 = EDGE_CURVE ( 'NONE', #88700, #1645, #69236, .T. ) ;
#74364 = FACE_BOUND ( 'NONE', #36712, .T. ) ;
#74365 = VERTEX_POINT ( 'NONE', #89535 ) ;
#74366 = CARTESIAN_POINT ( 'NONE',  ( 186.4843750003414016, -8.734944146203032389, -1.604583208406768146E-15 ) ) ;
#74367 = CARTESIAN_POINT ( 'NONE',  ( 14.39999999999989555, 2.500000000000000000, 0.3464101615137736845 ) ) ;
#74368 = DIRECTION ( 'NONE',  ( 0.000000000000000000, 1.000000000000000000, 0.000000000000000000 ) ) ;
#74369 = CARTESIAN_POINT ( 'NONE',  ( 8.299999999999922551, 12.50000000000000000, 4.330127018922196314 ) ) ;
#74370 = LINE ( 'NONE', #4309, #33923 ) ;
#74371 = AXIS2_PLACEMENT_3D ( 'NONE', #118112, #96521, #67055 ) ;
#74372 = CARTESIAN_POINT ( 'NONE',  ( -11.05000000000000249, 12.50000000000000000, -1.818653347947322141 ) ) ;
#74373 = FACE_OUTER_BOUND ( 'NONE', #68026, .T. ) ;
#74374 = CIRCLE ( 'NONE', #107823, 0.06509327318403745899 ) ;
#74375 = CONICAL_SURFACE ( 'NONE', #5414, 0.1000000000000002554, 0.003490658503988666988 ) ;
#74376 = DIRECTION ( 'NONE',  ( -0.000000000000000000, -0.000000000000000000, -1.000000000000000000 ) ) ;
#74377 = AXIS2_PLACEMENT_3D ( 'NONE', #122573, #34850, #85211 ) ;
#74378 = VERTEX_POINT ( 'NONE', #129494 ) ;
#74379 = VERTEX_POINT ( 'NONE', #39815 ) ;
#74380 = EDGE_LOOP ( 'NONE', ( #79563, #128676, #47985, #59923 ) ) ;
#74381 = ORIENTED_EDGE ( 'NONE', *, *, #95970, .F. ) ;
#74382 = AXIS2_PLACEMENT_3D ( 'NONE', #54349, #93638, #35368 ) ;
#74383 = ORIENTED_EDGE ( 'NONE', *, *, #85649, .T. ) ;
#74384 = DIRECTION ( 'NONE',  ( 0.000000000000000000, 0.000000000000000000, 1.000000000000000000 ) ) ;
#74385 = DIRECTION ( 'NONE',  ( -0.000000000000000000, 1.000000000000000000, -0.000000000000000000 ) ) ;
#74386 = ORIENTED_EDGE ( 'NONE', *, *, #32744, .F. ) ;
#74387 = FACE_BOUND ( 'NONE', #32969, .T. ) ;
#74388 = PLANE ( 'NONE',  #83384 ) ;
#74389 = EDGE_CURVE ( 'NONE', #79739, #11888, #29988, .T. ) ;
#74390 = CARTESIAN_POINT ( 'NONE',  ( -3.300000000000027800, 2.500000000000000000, -4.330127018922201643 ) ) ;
#74391 = EDGE_LOOP ( 'NONE', ( #48820, #103940, #88837, #88880 ) ) ;
#74392 = DIRECTION ( 'NONE',  ( 0.000000000000000000, 0.000000000000000000, -1.000000000000000000 ) ) ;
#74393 = DIRECTION ( 'NONE',  ( 0.000000000000000000, 0.000000000000000000, 1.000000000000000000 ) ) ;
#74394 = EDGE_CURVE ( 'NONE', #38823, #129286, #123055, .T. ) ;
#74395 = CARTESIAN_POINT ( 'NONE',  ( -6.650000000000015454, 12.50000000000000000, 2.792790559304612064 ) ) ;
#74397 = ORIENTED_EDGE ( 'NONE', *, *, #69783, .F. ) ;
#74396 = AXIS2_PLACEMENT_3D ( 'NONE', #64735, #105958, #66661 ) ;
#74398 = CARTESIAN_POINT ( 'NONE',  ( 2.699999999999947331, 2.500000000000000000, -4.676537180435978769 ) ) ;
#74399 = EDGE_CURVE ( 'NONE', #77648, #109309, #66605, .T. ) ;
#74400 = VERTEX_POINT ( 'NONE', #25791 ) ;
#74401 = ORIENTED_EDGE ( 'NONE', *, *, #97756, .T. ) ;
#74402 = ORIENTED_EDGE ( 'NONE', *, *, #116074, .T. ) ;
#74403 = EDGE_CURVE ( 'NONE', #9181, #111170, #10187, .T. ) ;
#74404 = CARTESIAN_POINT ( 'NONE',  ( -5.650000000000019895, 2.500000000000000000, 6.841600689897072485 ) ) ;
#74405 = CARTESIAN_POINT ( 'NONE',  ( -7.700000000000016165, 2.500000000000000000, -3.983716857408426293 ) ) ;
#74406 = AXIS2_PLACEMENT_3D ( 'NONE', #52346, #12414, #72003 ) ;
#74407 = DIRECTION ( 'NONE',  ( 0.000000000000000000, 0.000000000000000000, -1.000000000000000000 ) ) ;
#74409 = ORIENTED_EDGE ( 'NONE', *, *, #121385, .F. ) ;
#74408 = EDGE_CURVE ( 'NONE', #97087, #112557, #83354, .T. ) ;
#74410 = FACE_OUTER_BOUND ( 'NONE', #91981, .T. ) ;
#74411 = AXIS2_PLACEMENT_3D ( 'NONE', #62323, #91126, #2731 ) ;
#74412 = EDGE_CURVE ( 'NONE', #31054, #37520, #26902, .T. ) ;
#74413 = AXIS2_PLACEMENT_3D ( 'NONE', #50713, #2240, #31722 ) ;
#74414 = CARTESIAN_POINT ( 'NONE',  ( 127.5000000000000000, 0.000000000000000000, 7.700000000000000178 ) ) ;
#74415 = AXIS2_PLACEMENT_3D ( 'NONE', #60856, #60236, #50387 ) ;
#74417 = EDGE_CURVE ( 'NONE', #61868, #105096, #54591, .T. ) ;
#74416 = CARTESIAN_POINT ( 'NONE',  ( -7.950000000000012612, 12.50000000000000000, -2.165063509461101710 ) ) ;
#74418 = CARTESIAN_POINT ( 'NONE',  ( 186.8645833340161175, -6.668395609140180369, 3.849999999999994760 ) ) ;
#74420 = EDGE_LOOP ( 'NONE', ( #25213, #203, #33361, #32402 ) ) ;
#74419 = DIRECTION ( 'NONE',  ( 0.000000000000000000, 0.000000000000000000, -1.000000000000000000 ) ) ;
#74421 = CARTESIAN_POINT ( 'NONE',  ( -13.09999999999999076, 12.50000000000000000, 4.741630453620009789 ) ) ;
#74422 = ORIENTED_EDGE ( 'NONE', *, *, #89075, .T. ) ;
#74423 = DIRECTION ( 'NONE',  ( 0.000000000000000000, 1.000000000000000000, 0.000000000000000000 ) ) ;
#74424 = ADVANCED_FACE ( 'NONE', ( #72491 ), #125201, .T. ) ;
#74425 = CIRCLE ( 'NONE', #9667, 0.06509327318403745899 ) ;
#74426 = EDGE_CURVE ( 'NONE', #49764, #82278, #52051, .T. ) ;
#74427 = VERTEX_POINT ( 'NONE', #52194 ) ;
#74429 = CIRCLE ( 'NONE', #43060, 0.06509327318403745899 ) ;
#74428 = AXIS2_PLACEMENT_3D ( 'NONE', #46401, #95520, #56222 ) ;
#74430 = ORIENTED_EDGE ( 'NONE', *, *, #25474, .F. ) ;
#74431 = DIRECTION ( 'NONE',  ( 0.000000000000000000, 0.000000000000000000, 1.000000000000000000 ) ) ;
#74432 = CARTESIAN_POINT ( 'NONE',  ( -1.850000000000033396, 2.500000000000000000, -1.818653347947325916 ) ) ;
#74433 = CARTESIAN_POINT ( 'NONE',  ( 8.749999999999918288, 12.50000000000000000, -1.472243186433550122 ) ) ;
#74434 = DIRECTION ( 'NONE',  ( 0.000000000000000000, 0.000000000000000000, -1.000000000000000000 ) ) ;
#74435 = CARTESIAN_POINT ( 'NONE',  ( 3.949999999999942446, 12.50000000000000000, -2.511473670974877948 ) ) ;
#74436 = ORIENTED_EDGE ( 'NONE', *, *, #9685, .F. ) ;
#74437 = ORIENTED_EDGE ( 'NONE', *, *, #98624, .F. ) ;
#74438 = PLANE ( 'NONE',  #64316 ) ;
#74439 = CONICAL_SURFACE ( 'NONE', #63972, 0.1000000000000002554, 0.003490658503988666988 ) ;
#74440 = DIRECTION ( 'NONE',  ( -0.000000000000000000, 1.000000000000000000, -0.000000000000000000 ) ) ;
#74441 = CARTESIAN_POINT ( 'NONE',  ( -4.350000000000023626, 2.500000000000000000, -1.818653347947325916 ) ) ;
#74442 = ORIENTED_EDGE ( 'NONE', *, *, #3336, .F. ) ;
#74443 = VERTEX_POINT ( 'NONE', #104979 ) ;
#74444 = LINE ( 'NONE', #84245, #97972 ) ;
#74445 = ORIENTED_EDGE ( 'NONE', *, *, #104266, .T. ) ;
#74446 = DIRECTION ( 'NONE',  ( -0.000000000000000000, 1.000000000000000000, -0.000000000000000000 ) ) ;
#74447 = DIRECTION ( 'NONE',  ( 0.000000000000000000, 0.000000000000000000, 1.000000000000000000 ) ) ;
#74448 = VERTEX_POINT ( 'NONE', #124647 ) ;
#74449 = DIRECTION ( 'NONE',  ( 0.000000000000000000, 1.000000000000000000, 0.000000000000000000 ) ) ;
#74450 = FACE_OUTER_BOUND ( 'NONE', #124501, .T. ) ;
#74451 = PLANE ( 'NONE',  #107444 ) ;
#74452 = CARTESIAN_POINT ( 'NONE',  ( 5.849999999999933920, 2.500000000000000000, -2.065063509461102065 ) ) ;
#74453 = ORIENTED_EDGE ( 'NONE', *, *, #104692, .F. ) ;
#74454 = FACE_OUTER_BOUND ( 'NONE', #102672, .T. ) ;
#74455 = CIRCLE ( 'NONE', #55663, 0.1000000000000002554 ) ;
#74456 = ADVANCED_FACE ( 'NONE', ( #46087 ), #102219, .T. ) ;
#74457 = AXIS2_PLACEMENT_3D ( 'NONE', #116648, #88470, #40038 ) ;
#74458 = CARTESIAN_POINT ( 'NONE',  ( 87.50000000000001421, -3.974992050023847145, 6.359987280038161828 ) ) ;
#74459 = VERTEX_POINT ( 'NONE', #45450 ) ;
#74460 = ORIENTED_EDGE ( 'NONE', *, *, #28598, .F. ) ;
#74461 = CARTESIAN_POINT ( 'NONE',  ( 184.8802083336747444, 4.367472073101515306, 7.564683531250000925 ) ) ;
#74462 = DIRECTION ( 'NONE',  ( -0.000000000000000000, 1.000000000000000000, -0.000000000000000000 ) ) ;
#74463 = LINE ( 'NONE', #122927, #104308 ) ;
#74464 = FACE_OUTER_BOUND ( 'NONE', #4225, .T. ) ;
#74467 = AXIS2_PLACEMENT_3D ( 'NONE', #94011, #25254, #72451 ) ;
#74466 = CARTESIAN_POINT ( 'NONE',  ( -1.850000000000033396, 2.500000000000000000, -6.048780366869526581 ) ) ;
#74465 = VECTOR ( 'NONE', #65781, 1000.000000000000000 ) ;
#74468 = EDGE_CURVE ( 'NONE', #77466, #87148, #62523, .T. ) ;
#74469 = CARTESIAN_POINT ( 'NONE',  ( 11.04999999999991012, 12.50000000000000000, -1.818653347947326138 ) ) ;
#74470 = CARTESIAN_POINT ( 'NONE',  ( 9.799999999999917222, 2.500000000000000000, 0.4464101615137735513 ) ) ;
#74471 = CARTESIAN_POINT ( 'NONE',  ( 13.54999999999989946, 2.500000000000000000, 2.511473670974873507 ) ) ;
#74472 = DIRECTION ( 'NONE',  ( 0.000000000000000000, 1.000000000000000000, 0.000000000000000000 ) ) ;
#74473 = CARTESIAN_POINT ( 'NONE',  ( 0.000000000000000000, 0.000000000000000000, -5.000000000000004441 ) ) ;
#74475 = CONICAL_SURFACE ( 'NONE', #24393, 0.1000000000000000472, 0.003490658503988666988 ) ;
#74474 = AXIS2_PLACEMENT_3D ( 'NONE', #127134, #78013, #27606 ) ;
#74476 = VERTEX_POINT ( 'NONE', #76190 ) ;
#74477 = ORIENTED_EDGE ( 'NONE', *, *, #104508, .T. ) ;
#74478 = VECTOR ( 'NONE', #110023, 1000.000000000000000 ) ;
#74479 = ORIENTED_EDGE ( 'NONE', *, *, #37984, .F. ) ;
#74480 = ORIENTED_EDGE ( 'NONE', *, *, #47656, .T. ) ;
#74481 = LINE ( 'NONE', #99601, #81290 ) ;
#74482 = DIRECTION ( 'NONE',  ( -0.000000000000000000, 1.000000000000000000, -0.000000000000000000 ) ) ;
#74483 = CARTESIAN_POINT ( 'NONE',  ( 8.349999999999919709, 2.500000000000000000, -2.957883832488653830 ) ) ;
#74484 = ORIENTED_EDGE ( 'NONE', *, *, #76192, .F. ) ;
#74485 = CARTESIAN_POINT ( 'NONE',  ( 20.59313469514024320, -2.666874593322334785, -2.243770147468747034 ) ) ;
#74486 = PLANE ( 'NONE',  #34502 ) ;
#74488 = VERTEX_POINT ( 'NONE', #92105 ) ;
#74487 = DIRECTION ( 'NONE',  ( -0.000000000000000000, 1.000000000000000000, -0.000000000000000000 ) ) ;
#74489 = DIRECTION ( 'NONE',  ( 0.000000000000000000, 1.000000000000000000, 0.000000000000000000 ) ) ;
#74490 = AXIS2_PLACEMENT_3D ( 'NONE', #119630, #48326, #48992 ) ;
#74491 = DIRECTION ( 'NONE',  ( 0.000000000000000000, 0.000000000000000000, 1.000000000000000000 ) ) ;
#74492 = ORIENTED_EDGE ( 'NONE', *, *, #90635, .F. ) ;
#74493 = CIRCLE ( 'NONE', #114208, 0.09999999999999982514 ) ;
#74494 = ORIENTED_EDGE ( 'NONE', *, *, #114636, .T. ) ;
#74495 = ORIENTED_EDGE ( 'NONE', *, *, #49900, .T. ) ;
#74496 = ORIENTED_EDGE ( 'NONE', *, *, #42842, .T. ) ;
#74497 = CARTESIAN_POINT ( 'NONE',  ( 129.5000000000000000, 0.000000000000000000, 0.000000000000000000 ) ) ;
#74498 = AXIS2_PLACEMENT_3D ( 'NONE', #77147, #88220, #6432 ) ;
#74499 = DIRECTION ( 'NONE',  ( 0.000000000000000000, 1.000000000000000000, 0.000000000000000000 ) ) ;
#74500 = DIRECTION ( 'NONE',  ( 0.000000000000000000, 0.000000000000000000, 1.000000000000000000 ) ) ;
#74501 = AXIS2_PLACEMENT_3D ( 'NONE', #99017, #29627, #68903 ) ;
#74502 = CARTESIAN_POINT ( 'NONE',  ( -7.950000000000012612, 2.500000000000000000, -2.165063509461101710 ) ) ;
#74503 = EDGE_CURVE ( 'NONE', #47024, #103084, #77080, .T. ) ;
#74504 = VERTEX_POINT ( 'NONE', #66357 ) ;
#74505 = LINE ( 'NONE', #73856, #23052 ) ;
#74506 = EDGE_LOOP ( 'NONE', ( #101342, #69019, #26092, #70635 ) ) ;
#74507 = CARTESIAN_POINT ( 'NONE',  ( 13.09999999999990195, 12.50000000000000000, -3.983716857408426293 ) ) ;
#74509 = EDGE_CURVE ( 'NONE', #121191, #4941, #79155, .T. ) ;
#74508 = CARTESIAN_POINT ( 'NONE',  ( 4.848431875658358869, -2.500000000000000000, -8.943854603575022821 ) ) ;
#74510 = ADVANCED_FACE ( 'NONE', ( #112410 ), #31915, .T. ) ;
#74511 = DIRECTION ( 'NONE',  ( 1.000000000000000000, 0.000000000000000000, 0.000000000000000000 ) ) ;
#74512 = CARTESIAN_POINT ( 'NONE',  ( -11.64999999999999680, 2.500000000000000000, -6.395190528383298378 ) ) ;
#74513 = ADVANCED_FACE ( 'NONE', ( #44805 ), #129337, .T. ) ;
#74514 = VECTOR ( 'NONE', #46044, 1000.000000000000000 ) ;
#74515 = ORIENTED_EDGE ( 'NONE', *, *, #61960, .T. ) ;
#74517 = AXIS2_PLACEMENT_3D ( 'NONE', #90321, #9204, #19677 ) ;
#74516 = CIRCLE ( 'NONE', #20138, 0.06509327318403745899 ) ;
#74518 = ORIENTED_EDGE ( 'NONE', *, *, #48102, .F. ) ;
#74519 = EDGE_CURVE ( 'NONE', #121477, #59645, #56135, .T. ) ;
#74521 = VERTEX_POINT ( 'NONE', #25141 ) ;
#74520 = EDGE_CURVE ( 'NONE', #17094, #83056, #33281, .T. ) ;
#74522 = DIRECTION ( 'NONE',  ( 0.000000000000000000, 1.000000000000000000, 0.000000000000000000 ) ) ;
#74523 = DIRECTION ( 'NONE',  ( 0.000000000000000000, 0.000000000000000000, -1.000000000000000000 ) ) ;
#74524 = DIRECTION ( 'NONE',  ( -4.274815082592931898E-19, -0.9999939076577903929, -0.003490651415223739937 ) ) ;
#74525 = EDGE_CURVE ( 'NONE', #84079, #36965, #99704, .T. ) ;
#74526 = FACE_BOUND ( 'NONE', #11866, .T. ) ;
#74527 = DIRECTION ( 'NONE',  ( 0.000000000000000000, 0.000000000000000000, 1.000000000000000000 ) ) ;
#74528 = DIRECTION ( 'NONE',  ( 0.000000000000000000, 1.000000000000000000, 0.000000000000000000 ) ) ;
#74529 = FACE_OUTER_BOUND ( 'NONE', #108059, .T. ) ;
#74530 = CARTESIAN_POINT ( 'NONE',  ( 187.1302083336747444, -4.367472073101514418, -7.564683531250002702 ) ) ;
#74531 = FACE_OUTER_BOUND ( 'NONE', #115041, .T. ) ;
#74532 = PLANE ( 'NONE',  #970 ) ;
#74533 = ORIENTED_EDGE ( 'NONE', *, *, #65088, .F. ) ;
#74534 = CARTESIAN_POINT ( 'NONE',  ( -8.749999999999976907, 2.500000000000000000, -6.395190528383296602 ) ) ;
#74535 = EDGE_LOOP ( 'NONE', ( #40219, #121672, #66225, #92448 ) ) ;
#74536 = ORIENTED_EDGE ( 'NONE', *, *, #114133, .T. ) ;
#74537 = ORIENTED_EDGE ( 'NONE', *, *, #61570, .T. ) ;
#74538 = ORIENTED_EDGE ( 'NONE', *, *, #42776, .F. ) ;
#74539 = CARTESIAN_POINT ( 'NONE',  ( 12.29999999999990656, 12.50000000000000000, 3.983716857408420964 ) ) ;
#74540 = FACE_BOUND ( 'NONE', #80643, .T. ) ;
#74541 = FACE_OUTER_BOUND ( 'NONE', #73596, .T. ) ;
#74542 = CIRCLE ( 'NONE', #76596, 0.09999999999999999167 ) ;
#74543 = AXIS2_PLACEMENT_3D ( 'NONE', #47769, #46457, #17642 ) ;
#74544 = ORIENTED_EDGE ( 'NONE', *, *, #69026, .T. ) ;
#74545 = CARTESIAN_POINT ( 'NONE',  ( 14.34999999999989306, 2.500000000000000000, -1.818653347947326138 ) ) ;
#74546 = DIRECTION ( 'NONE',  ( 0.000000000000000000, -0.000000000000000000, 1.000000000000000000 ) ) ;
#74547 = ORIENTED_EDGE ( 'NONE', *, *, #91670, .F. ) ;
#74548 = DIRECTION ( 'NONE',  ( -0.000000000000000000, 1.000000000000000000, -0.000000000000000000 ) ) ;
#74549 = DIRECTION ( 'NONE',  ( 0.000000000000000000, -0.000000000000000000, 1.000000000000000000 ) ) ;
#74550 = CIRCLE ( 'NONE', #120528, 0.06509327318403745899 ) ;
#74551 = ADVANCED_FACE ( 'NONE', ( #68286 ), #59801, .T. ) ;
#74552 = ORIENTED_EDGE ( 'NONE', *, *, #15215, .F. ) ;
#74553 = EDGE_CURVE ( 'NONE', #47322, #10760, #104081, .T. ) ;
#74554 = CARTESIAN_POINT ( 'NONE',  ( -5.850000000000019185, 12.50000000000000000, 6.560283801567334372 ) ) ;
#74555 = CARTESIAN_POINT ( 'NONE',  ( -7.050000000000013145, 12.50000000000000000, 6.430097255199259010 ) ) ;
#74556 = EDGE_CURVE ( 'NONE', #72795, #46368, #47374, .T. ) ;
#74558 = AXIS2_PLACEMENT_3D ( 'NONE', #29461, #69365, #37354 ) ;
#74557 = AXIS2_PLACEMENT_3D ( 'NONE', #87177, #89767, #61615 ) ;
#74559 = ORIENTED_EDGE ( 'NONE', *, *, #56081, .T. ) ;
#74560 = CIRCLE ( 'NONE', #116312, 0.06509327318403745899 ) ;
#74561 = CARTESIAN_POINT ( 'NONE',  ( 145.7653593504141725, 2.500000000000000000, -1.098523788719517169 ) ) ;
#74562 = CARTESIAN_POINT ( 'NONE',  ( 13.09999999999990195, 2.500000000000000000, 3.983716857408420076 ) ) ;
#74564 = ADVANCED_FACE ( 'NONE', ( #38876 ), #9987, .T. ) ;
#74563 = LINE ( 'NONE', #114481, #118309 ) ;
#74565 = EDGE_CURVE ( 'NONE', #21407, #71164, #97813, .T. ) ;
#74566 = ORIENTED_EDGE ( 'NONE', *, *, #78991, .T. ) ;
#74567 = ORIENTED_EDGE ( 'NONE', *, *, #85001, .T. ) ;
#74568 = FACE_OUTER_BOUND ( 'NONE', #103779, .T. ) ;
#74569 = VERTEX_POINT ( 'NONE', #77469 ) ;
#74570 = CARTESIAN_POINT ( 'NONE',  ( -2.500000000000031086, 12.50000000000000000, 3.637306695894644726 ) ) ;
#74571 = CARTESIAN_POINT ( 'NONE',  ( -8.300000000000011369, 2.500000000000000000, -4.330127018922201643 ) ) ;
#74572 = ADVANCED_FACE ( 'NONE', ( #87281 ), #27006, .T. ) ;
#74573 = ADVANCED_FACE ( 'NONE', ( #29664 ), #59136, .T. ) ;
#74574 = ORIENTED_EDGE ( 'NONE', *, *, #5676, .F. ) ;
#74575 = DIRECTION ( 'NONE',  ( 0.000000000000000000, 0.000000000000000000, 1.000000000000000000 ) ) ;
#74576 = DIRECTION ( 'NONE',  ( 0.000000000000000000, 0.000000000000000000, -1.000000000000000000 ) ) ;
#74577 = DIRECTION ( 'NONE',  ( 0.000000000000000000, 1.000000000000000000, 0.000000000000000000 ) ) ;
#74578 = CARTESIAN_POINT ( 'NONE',  ( 0.3999999999999568345, 12.50000000000000000, -5.022947341949754119 ) ) ;
#74579 = AXIS2_PLACEMENT_3D ( 'NONE', #74416, #35778, #76354 ) ;
#74581 = EDGE_CURVE ( 'NONE', #51138, #69316, #89687, .T. ) ;
#74580 = DIRECTION ( 'NONE',  ( 0.000000000000000000, 0.000000000000000000, 1.000000000000000000 ) ) ;
#74582 = AXIS2_PLACEMENT_3D ( 'NONE', #17221, #15299, #106911 ) ;
#74583 = EDGE_LOOP ( 'NONE', ( #96358, #103852 ) ) ;
#74584 = ORIENTED_EDGE ( 'NONE', *, *, #9143, .F. ) ;
#74585 = LINE ( 'NONE', #79113, #47513 ) ;
#74586 = CIRCLE ( 'NONE', #34901, 0.1000000000000002554 ) ;
#74587 = CARTESIAN_POINT ( 'NONE',  ( 104.9410342067506150, 6.602324511409650043, -3.967845207721173661 ) ) ;
#74588 = DIRECTION ( 'NONE',  ( -0.000000000000000000, 1.000000000000000000, -0.000000000000000000 ) ) ;
#74590 = EDGE_LOOP ( 'NONE', ( #113617, #8943, #47077, #90770 ) ) ;
#74589 = EDGE_LOOP ( 'NONE', ( #124844, #29612, #108972, #113451 ) ) ;
#74591 = ORIENTED_EDGE ( 'NONE', *, *, #16369, .F. ) ;
#74592 = DIRECTION ( 'NONE',  ( 0.000000000000000000, 0.000000000000000000, 1.000000000000000000 ) ) ;
#74593 = CONICAL_SURFACE ( 'NONE', #99737, 0.1000000000000000056, 0.003490658503988666988 ) ;
#74594 = FACE_OUTER_BOUND ( 'NONE', #44221, .T. ) ;
#74595 = DIRECTION ( 'NONE',  ( 0.000000000000000000, 1.000000000000000000, 0.000000000000000000 ) ) ;
#74596 = AXIS2_PLACEMENT_3D ( 'NONE', #40714, #31516, #11219 ) ;
#74597 =( NAMED_UNIT ( * ) SI_UNIT ( $, .STERADIAN. ) SOLID_ANGLE_UNIT ( ) );
#74598 = CARTESIAN_POINT ( 'NONE',  ( 4.349999999999936584, 12.50000000000000000, 6.148780366869520009 ) ) ;
#74599 = DIRECTION ( 'NONE',  ( -0.000000000000000000, 1.000000000000000000, -0.000000000000000000 ) ) ;
#74600 = DIRECTION ( 'NONE',  ( 0.000000000000000000, 1.000000000000000000, 0.000000000000000000 ) ) ;
#74601 = DIRECTION ( 'NONE',  ( 0.000000000000000000, 1.000000000000000000, 0.000000000000000000 ) ) ;
#74602 = CARTESIAN_POINT ( 'NONE',  ( 1.049999999999953637, 2.500000000000000000, 2.611473670974873151 ) ) ;
#74603 = CONICAL_SURFACE ( 'NONE', #89272, 0.1000000000000002554, 0.003490658503988666988 ) ;
#74604 = DIRECTION ( 'NONE',  ( 0.000000000000000000, 0.000000000000000000, -1.000000000000000000 ) ) ;
#74605 = AXIS2_PLACEMENT_3D ( 'NONE', #21070, #60998, #91112 ) ;
#74606 = ORIENTED_EDGE ( 'NONE', *, *, #86182, .F. ) ;
#74608 = AXIS2_PLACEMENT_3D ( 'NONE', #76510, #4505, #75214 ) ;
#74607 = CIRCLE ( 'NONE', #11900, 0.1000000000000000472 ) ;
#74609 = LINE ( 'NONE', #114517, #31942 ) ;
#74610 = ORIENTED_EDGE ( 'NONE', *, *, #24128, .F. ) ;
#74611 = EDGE_LOOP ( 'NONE', ( #39746, #118097, #70828, #101157 ) ) ;
#74612 = PLANE ( 'NONE',  #81754 ) ;
#74613 = DIRECTION ( 'NONE',  ( 0.000000000000000000, 1.000000000000000000, 0.000000000000000000 ) ) ;
#74614 = DIRECTION ( 'NONE',  ( 1.000000000000000000, 0.000000000000000000, 0.000000000000000000 ) ) ;
#74615 = CARTESIAN_POINT ( 'NONE',  ( 3.949999999999941558, 12.50000000000000000, -1.818653347947326138 ) ) ;
#74616 = ADVANCED_FACE ( 'NONE', ( #27719 ), #43456, .T. ) ;
#74617 = DIRECTION ( 'NONE',  ( -0.000000000000000000, 1.000000000000000000, -0.000000000000000000 ) ) ;
#74618 = DIRECTION ( 'NONE',  ( 0.000000000000000000, 0.000000000000000000, -1.000000000000000000 ) ) ;
#74619 = DIRECTION ( 'NONE',  ( 0.000000000000000000, 0.000000000000000000, -1.000000000000000000 ) ) ;
#74620 = EDGE_LOOP ( 'NONE', ( #12053, #38405, #31470, #13386 ) ) ;
#74621 = CARTESIAN_POINT ( 'NONE',  ( -11.05000000000000249, 2.500000000000000000, -6.148780366869522673 ) ) ;
#74622 = VECTOR ( 'NONE', #68450, 1000.000000000000000 ) ;
#74623 = LINE ( 'NONE', #76561, #56290 ) ;
#74624 = ORIENTED_EDGE ( 'NONE', *, *, #114161, .F. ) ;
#74625 = EDGE_LOOP ( 'NONE', ( #89203, #76637, #8952, #385 ) ) ;
#74626 = ORIENTED_EDGE ( 'NONE', *, *, #58941, .F. ) ;
#74627 = ORIENTED_EDGE ( 'NONE', *, *, #75726, .T. ) ;
#74628 = CARTESIAN_POINT ( 'NONE',  ( 0.6499999999999561684, 12.50000000000000000, -1.883746621131363375 ) ) ;
#74629 = LINE ( 'NONE', #96190, #93807 ) ;
#74630 = CIRCLE ( 'NONE', #18188, 0.1000000000000002554 ) ;
#74631 = LINE ( 'NONE', #61609, #17171 ) ;
#74633 = DIRECTION ( 'NONE',  ( -0.000000000000000000, -1.000000000000000000, -0.000000000000000000 ) ) ;
#74632 = VECTOR ( 'NONE', #578, 1000.000000000000000 ) ;
#74634 = CARTESIAN_POINT ( 'NONE',  ( 5.399999999999932854, 2.500000000000000000, 4.922947341949748257 ) ) ;
#74635 = ORIENTED_EDGE ( 'NONE', *, *, #22269, .T. ) ;
#74636 = CARTESIAN_POINT ( 'NONE',  ( 11.24999999999990941, 12.50000000000000000, 7.188010851410848723 ) ) ;
#74637 = CARTESIAN_POINT ( 'NONE',  ( 13.94999999999989448, 12.50000000000000000, -2.511473670974877948 ) ) ;
#74639 = AXIS2_PLACEMENT_3D ( 'NONE', #113114, #23447, #123568 ) ;
#74638 = CONICAL_SURFACE ( 'NONE', #45409, 0.1000000000000000472, 0.003490658503988666988 ) ;
#74640 = DIRECTION ( 'NONE',  ( -0.000000000000000000, 1.000000000000000000, -0.000000000000000000 ) ) ;
#74641 = VERTEX_POINT ( 'NONE', #127858 ) ;
#74642 = ORIENTED_EDGE ( 'NONE', *, *, #105540, .F. ) ;
#74643 = ORIENTED_EDGE ( 'NONE', *, *, #108026, .T. ) ;
#74644 = DIRECTION ( 'NONE',  ( 0.000000000000000000, 0.000000000000000000, 1.000000000000000000 ) ) ;
#74646 = AXIS2_PLACEMENT_3D ( 'NONE', #54251, #114449, #25409 ) ;
#74645 = AXIS2_PLACEMENT_3D ( 'NONE', #85097, #18771, #99281 ) ;
#74647 = FACE_OUTER_BOUND ( 'NONE', #69525, .T. ) ;
#74648 = PLANE ( 'NONE',  #71171 ) ;
#74650 = EDGE_CURVE ( 'NONE', #3051, #95827, #16512, .T. ) ;
#74649 = AXIS2_PLACEMENT_3D ( 'NONE', #107558, #49305, #46703 ) ;
#74651 = VERTEX_POINT ( 'NONE', #108851 ) ;
#74652 = CARTESIAN_POINT ( 'NONE',  ( 10.79999999999991012, 2.500000000000000000, 4.330127018922196314 ) ) ;
#74653 = CARTESIAN_POINT ( 'NONE',  ( -13.54999999999998828, 2.500000000000000000, 1.818653347947325472 ) ) ;
#74654 = EDGE_CURVE ( 'NONE', #119878, #27277, #116370, .T. ) ;
#74655 = DIRECTION ( 'NONE',  ( 0.000000000000000000, 0.000000000000000000, -1.000000000000000000 ) ) ;
#74656 = CARTESIAN_POINT ( 'NONE',  ( 2.099999999999947686, 2.500000000000000000, 4.922947341949748257 ) ) ;
#74657 = DIRECTION ( 'NONE',  ( -0.000000000000000000, -1.000000000000000000, -0.000000000000000000 ) ) ;
#74658 = ADVANCED_FACE ( 'NONE', ( #129185 ), #122861, .T. ) ;
#74659 = EDGE_LOOP ( 'NONE', ( #12027, #83366, #73986, #9336 ) ) ;
#74660 = DIRECTION ( 'NONE',  ( -0.000000000000000000, 1.000000000000000000, -0.000000000000000000 ) ) ;
#74661 = ORIENTED_EDGE ( 'NONE', *, *, #116320, .F. ) ;
#74662 = EDGE_CURVE ( 'NONE', #52767, #91667, #56231, .T. ) ;
#74663 = ADVANCED_FACE ( 'NONE', ( #31602 ), #30933, .T. ) ;
#74664 = ORIENTED_EDGE ( 'NONE', *, *, #125947, .F. ) ;
#74665 = EDGE_CURVE ( 'NONE', #59178, #58192, #22446, .T. ) ;
#74667 = EDGE_CURVE ( 'NONE', #28644, #59160, #116585, .T. ) ;
#74666 = DIRECTION ( 'NONE',  ( -0.000000000000000000, 1.000000000000000000, -0.000000000000000000 ) ) ;
#74668 = ADVANCED_FACE ( 'NONE', ( #72181 ), #127074, .T. ) ;
#74669 = FACE_BOUND ( 'NONE', #28204, .T. ) ;
#74670 = CIRCLE ( 'NONE', #124853, 0.06509327318403745899 ) ;
#74671 = DIRECTION ( 'NONE',  ( -4.274815082592931898E-19, -0.9999939076577903929, -0.003490651415223739937 ) ) ;
#74672 = CARTESIAN_POINT ( 'NONE',  ( -7.500000000000001776, -2.500000000000000000, 9.000000000000001776 ) ) ;
#74673 = AXIS2_PLACEMENT_3D ( 'NONE', #99542, #28216, #128370 ) ;
#74674 = CARTESIAN_POINT ( 'NONE',  ( 11.04999999999991012, 2.500000000000000000, -1.818653347947326138 ) ) ;
#74675 = VERTEX_POINT ( 'NONE', #91164 ) ;
#74676 = CIRCLE ( 'NONE', #91393, 0.1000000000000002554 ) ;
#74677 = ORIENTED_EDGE ( 'NONE', *, *, #52602, .F. ) ;
#74678 = CARTESIAN_POINT ( 'NONE',  ( -4.150000000000025224, 12.50000000000000000, -1.472243186433550122 ) ) ;
#74679 = DIRECTION ( 'NONE',  ( 0.000000000000000000, 1.000000000000000000, 0.000000000000000000 ) ) ;
#74680 = EDGE_CURVE ( 'NONE', #73467, #97281, #41441, .T. ) ;
#74682 = CARTESIAN_POINT ( 'NONE',  ( 15.83209681635555910, -2.500000000000000000, -5.404881881984148428 ) ) ;
#74681 = CIRCLE ( 'NONE', #18328, 0.06509327318403745899 ) ;
#74684 = CARTESIAN_POINT ( 'NONE',  ( -10.84999999999999964, 12.50000000000000000, 1.407149913249508000 ) ) ;
#74683 = AXIS2_PLACEMENT_3D ( 'NONE', #103863, #52818, #113024 ) ;
#74685 = VERTEX_POINT ( 'NONE', #101637 ) ;
#74686 = DIRECTION ( 'NONE',  ( -4.274815082592931898E-19, -0.9999939076577903929, -0.003490651415223739937 ) ) ;
#74687 = AXIS2_PLACEMENT_3D ( 'NONE', #103477, #62908, #73362 ) ;
#74688 = FACE_OUTER_BOUND ( 'NONE', #27992, .T. ) ;
#74689 = ORIENTED_EDGE ( 'NONE', *, *, #72, .T. ) ;
#74690 = DIRECTION ( 'NONE',  ( -4.274815082592931898E-19, -0.9999939076577903929, -0.003490651415223739937 ) ) ;
#74691 = AXIS2_PLACEMENT_3D ( 'NONE', #2447, #50286, #43070 ) ;
#74692 = VERTEX_POINT ( 'NONE', #11950 ) ;
#74693 = FACE_BOUND ( 'NONE', #76962, .T. ) ;
#74694 = CARTESIAN_POINT ( 'NONE',  ( -12.49999999999995914, 2.500000000000000000, 1.843143693225357538E-15 ) ) ;
#74696 = CIRCLE ( 'NONE', #83033, 0.06509327318403745899 ) ;
#74695 = AXIS2_PLACEMENT_3D ( 'NONE', #31782, #71700, #61899 ) ;
#74697 = VERTEX_POINT ( 'NONE', #81353 ) ;
#74698 = CARTESIAN_POINT ( 'NONE',  ( 12.49999999999990230, 12.50000000000000000, -0.6277270498435166823 ) ) ;
#74699 = LINE ( 'NONE', #113325, #108637 ) ;
#74700 = ORIENTED_EDGE ( 'NONE', *, *, #63426, .T. ) ;
#74701 = VERTEX_POINT ( 'NONE', #40129 ) ;
#74702 = CARTESIAN_POINT ( 'NONE',  ( 185.5885416670080872, -6.551208109652273848, -3.782341765625003571 ) ) ;
#74703 = CARTESIAN_POINT ( 'NONE',  ( 185.7135416670080588, 4.367472073101518859, -7.564683531249999149 ) ) ;
#74704 = CARTESIAN_POINT ( 'NONE',  ( -12.89999999999999147, 2.500000000000000000, 1.843143693225357538E-15 ) ) ;
#74705 = DIRECTION ( 'NONE',  ( 0.000000000000000000, 0.000000000000000000, 1.000000000000000000 ) ) ;
#74706 = DIRECTION ( 'NONE',  ( 0.000000000000000000, 0.000000000000000000, -1.000000000000000000 ) ) ;
#74707 = DIRECTION ( 'NONE',  ( 0.000000000000000000, 0.000000000000000000, 1.000000000000000000 ) ) ;
#74708 = ADVANCED_FACE ( 'NONE', ( #91807 ), #14172, .T. ) ;
#74709 = DIRECTION ( 'NONE',  ( 0.000000000000000000, 0.000000000000000000, 1.000000000000000000 ) ) ;
#74710 = CIRCLE ( 'NONE', #14051, 0.06509327318403745899 ) ;
#74711 = EDGE_CURVE ( 'NONE', #99143, #30225, #64359, .T. ) ;
#74712 = VERTEX_POINT ( 'NONE', #111429 ) ;
#74713 = ADVANCED_FACE ( 'NONE', ( #10634 ), #81106, .T. ) ;
#74714 = ORIENTED_EDGE ( 'NONE', *, *, #5126, .F. ) ;
#74715 = CARTESIAN_POINT ( 'NONE',  ( -8.150000000000012790, 2.500000000000000000, -2.511473670974877948 ) ) ;
#74716 = DIRECTION ( 'NONE',  ( -0.000000000000000000, -1.000000000000000000, -0.000000000000000000 ) ) ;
#74717 = DIRECTION ( 'NONE',  ( 0.000000000000000000, 0.000000000000000000, -1.000000000000000000 ) ) ;
#74718 = FACE_OUTER_BOUND ( 'NONE', #92984, .T. ) ;
#74720 = ORIENTED_EDGE ( 'NONE', *, *, #18722, .F. ) ;
#74719 = EDGE_LOOP ( 'NONE', ( #13875, #84989, #18263, #117509 ) ) ;
#74721 = CARTESIAN_POINT ( 'NONE',  ( 3.349999999999945466, 12.50000000000000000, -2.165063509461101710 ) ) ;
#74722 = EDGE_LOOP ( 'NONE', ( #120486, #4322, #5059, #822 ) ) ;
#74723 = ADVANCED_FACE ( 'NONE', ( #12587 ), #52519, .T. ) ;
#74724 = DIRECTION ( 'NONE',  ( -0.000000000000000000, -1.000000000000000000, -0.000000000000000000 ) ) ;
#74725 = CARTESIAN_POINT ( 'NONE',  ( -10.40000000000000213, 2.500000000000000000, -0.5928203230275541635 ) ) ;
#74727 = VERTEX_POINT ( 'NONE', #80711 ) ;
#74726 = EDGE_CURVE ( 'NONE', #106877, #117445, #5759, .T. ) ;
#74728 = CARTESIAN_POINT ( 'NONE',  ( 9.349999999999919709, 2.500000000000000000, -6.048780366869526581 ) ) ;
#74729 = CARTESIAN_POINT ( 'NONE',  ( -9.150000000000005684, 12.50000000000000000, 6.495190528383297135 ) ) ;
#74731 = EDGE_CURVE ( 'NONE', #41978, #90278, #119980, .T. ) ;
#74730 = CIRCLE ( 'NONE', #95658, 0.09999999999999982514 ) ;
#74732 = DIRECTION ( 'NONE',  ( -0.000000000000000000, 1.000000000000000000, -0.000000000000000000 ) ) ;
#74733 = VECTOR ( 'NONE', #64979, 1000.000000000000000 ) ;
#74734 = EDGE_CURVE ( 'NONE', #121834, #104854, #30977, .T. ) ;
#74735 = DIRECTION ( 'NONE',  ( 0.000000000000000000, 0.000000000000000000, -1.000000000000000000 ) ) ;
#74736 = LINE ( 'NONE', #7260, #101780 ) ;
#74737 = DIRECTION ( 'NONE',  ( 0.000000000000000000, 1.000000000000000000, 0.000000000000000000 ) ) ;
#74738 = CARTESIAN_POINT ( 'NONE',  ( 187.1510416670080588, 4.367472073101518859, -7.564683531249999149 ) ) ;
#74739 = CARTESIAN_POINT ( 'NONE',  ( 4.599999999999938360, 12.50000000000000000, -2.276824562219559311E-15 ) ) ;
#74741 = EDGE_CURVE ( 'NONE', #109874, #77490, #22531, .T. ) ;
#74740 = DIRECTION ( 'NONE',  ( 0.000000000000000000, 0.000000000000000000, -1.000000000000000000 ) ) ;
#74743 = CIRCLE ( 'NONE', #124916, 0.09999999999999982514 ) ;
#74742 = AXIS2_PLACEMENT_3D ( 'NONE', #15570, #106535, #55518 ) ;
#74744 = ORIENTED_EDGE ( 'NONE', *, *, #92553, .T. ) ;
#74745 = EDGE_LOOP ( 'NONE', ( #66617, #80258, #21013, #28328 ) ) ;
#74746 = AXIS2_PLACEMENT_3D ( 'NONE', #64921, #114040, #115967 ) ;
#74747 = ORIENTED_EDGE ( 'NONE', *, *, #109467, .F. ) ;
#74748 = DIRECTION ( 'NONE',  ( 0.000000000000000000, 0.000000000000000000, -1.000000000000000000 ) ) ;
#74749 = ORIENTED_EDGE ( 'NONE', *, *, #98076, .T. ) ;
#74750 = CARTESIAN_POINT ( 'NONE',  ( 0.8499999999999550138, 2.500000000000000000, -5.702370205355749455 ) ) ;
#74752 = ORIENTED_EDGE ( 'NONE', *, *, #92889, .T. ) ;
#74751 = ORIENTED_EDGE ( 'NONE', *, *, #110678, .T. ) ;
#74753 = EDGE_LOOP ( 'NONE', ( #25023, #10895, #5044, #26779 ) ) ;
#74754 = DIRECTION ( 'NONE',  ( 0.000000000000000000, 0.000000000000000000, 1.000000000000000000 ) ) ;
#74755 = AXIS2_PLACEMENT_3D ( 'NONE', #74966, #114878, #76264 ) ;
#74756 = AXIS2_PLACEMENT_3D ( 'NONE', #30945, #41410, #11921 ) ;
#74757 = FACE_OUTER_BOUND ( 'NONE', #49971, .T. ) ;
#74758 = DIRECTION ( 'NONE',  ( 0.000000000000000000, 1.000000000000000000, 0.000000000000000000 ) ) ;
#74759 = DIRECTION ( 'NONE',  ( 0.000000000000000000, -0.9999939076577903929, 0.003490651415223739937 ) ) ;
#74760 = DIRECTION ( 'NONE',  ( 0.000000000000000000, 1.000000000000000000, 0.000000000000000000 ) ) ;
#74761 = ADVANCED_FACE ( 'NONE', ( #70015 ), #38637, .T. ) ;
#74762 = ORIENTED_EDGE ( 'NONE', *, *, #52108, .F. ) ;
#74763 = DIRECTION ( 'NONE',  ( 0.000000000000000000, 0.000000000000000000, -1.000000000000000000 ) ) ;
#74764 = EDGE_LOOP ( 'NONE', ( #39979, #91496 ) ) ;
#74765 = CIRCLE ( 'NONE', #129071, 0.09999999999999982514 ) ;
#74766 = EDGE_LOOP ( 'NONE', ( #32650, #26670, #42555, #23876 ) ) ;
#74767 = EDGE_LOOP ( 'NONE', ( #126227, #47288 ) ) ;
#74768 = CONICAL_SURFACE ( 'NONE', #74855, 0.1000000000000000472, 0.003490658503988666988 ) ;
#74769 = CARTESIAN_POINT ( 'NONE',  ( -1.050000000000037792, 12.50000000000000000, 1.883746621131358934 ) ) ;
#74770 = ORIENTED_EDGE ( 'NONE', *, *, #56900, .T. ) ;
#74771 = ORIENTED_EDGE ( 'NONE', *, *, #74264, .T. ) ;
#74772 = VERTEX_POINT ( 'NONE', #109279 ) ;
#74773 = CONICAL_SURFACE ( 'NONE', #3656, 0.1000000000000002554, 0.003490658503988666988 ) ;
#74775 = CARTESIAN_POINT ( 'NONE',  ( -3.642919299551294898E-14, 12.50000000000000000, 0.6928203230275518099 ) ) ;
#74774 = CIRCLE ( 'NONE', #62262, 0.09999999999999999167 ) ;
#74776 = DIRECTION ( 'NONE',  ( 0.000000000000000000, -0.9999939076577903929, 0.003490651415223739937 ) ) ;
#74778 = AXIS2_PLACEMENT_3D ( 'NONE', #65131, #86060, #124718 ) ;
#74777 = CARTESIAN_POINT ( 'NONE',  ( -1.250000000000035749, 12.50000000000000000, -7.188010851410854052 ) ) ;
#74779 = EDGE_CURVE ( 'NONE', #41136, #17717, #95673, .T. ) ;
#74780 = CARTESIAN_POINT ( 'NONE',  ( 1.899999999999951283, 2.500000000000000000, 0.4464101615137736623 ) ) ;
#74781 = DIRECTION ( 'NONE',  ( 0.000000000000000000, 0.000000000000000000, -1.000000000000000000 ) ) ;
#74782 = CARTESIAN_POINT ( 'NONE',  ( 8.949999999999917577, 12.50000000000000000, -2.446380397790840266 ) ) ;
#74783 = ORIENTED_EDGE ( 'NONE', *, *, #14551, .F. ) ;
#74784 = AXIS2_PLACEMENT_3D ( 'NONE', #25132, #96440, #6129 ) ;
#74786 = VECTOR ( 'NONE', #80851, 1000.000000000000000 ) ;
#74785 = CARTESIAN_POINT ( 'NONE',  ( 9.599999999999914380, 2.500000000000000000, 5.122947341949749323 ) ) ;
#74787 = ORIENTED_EDGE ( 'NONE', *, *, #112257, .T. ) ;
#74788 = AXIS2_PLACEMENT_3D ( 'NONE', #59567, #39281, #70638 ) ;
#74789 = PLANE ( 'NONE',  #40140 ) ;
#74790 = ORIENTED_EDGE ( 'NONE', *, *, #77206, .F. ) ;
#74791 = CARTESIAN_POINT ( 'NONE',  ( -11.69999999999999574, 2.500000000000000000, 4.330127018922196314 ) ) ;
#74792 = ORIENTED_EDGE ( 'NONE', *, *, #20197, .F. ) ;
#74793 = CIRCLE ( 'NONE', #18341, 0.1000000000000002554 ) ;
#74794 = EDGE_CURVE ( 'NONE', #83303, #52300, #58903, .T. ) ;
#74795 = EDGE_LOOP ( 'NONE', ( #97941, #44337 ) ) ;
#74796 = FACE_OUTER_BOUND ( 'NONE', #21041, .T. ) ;
#74797 = CARTESIAN_POINT ( 'NONE',  ( 4.349999999999941025, 2.500000000000000000, -6.248780366869526759 ) ) ;
#74799 = AXIS2_PLACEMENT_3D ( 'NONE', #17154, #106224, #105581 ) ;
#74798 = AXIS2_PLACEMENT_3D ( 'NONE', #60467, #878, #90535 ) ;
#74800 = FACE_OUTER_BOUND ( 'NONE', #102366, .T. ) ;
#74801 = DIRECTION ( 'NONE',  ( 0.000000000000000000, 0.000000000000000000, 1.000000000000000000 ) ) ;
#74802 = ORIENTED_EDGE ( 'NONE', *, *, #2983, .T. ) ;
#74803 = DIRECTION ( 'NONE',  ( -0.000000000000000000, -1.000000000000000000, -0.000000000000000000 ) ) ;
#74804 = DIRECTION ( 'NONE',  ( 0.000000000000000000, 0.000000000000000000, 1.000000000000000000 ) ) ;
#74805 = CARTESIAN_POINT ( 'NONE',  ( -11.04999999999999893, 2.500000000000000000, 1.818653347947321475 ) ) ;
#74806 = DIRECTION ( 'NONE',  ( 0.000000000000000000, 1.000000000000000000, 0.000000000000000000 ) ) ;
#74807 = CARTESIAN_POINT ( 'NONE',  ( 1.849999999999950129, 12.50000000000000000, -6.841600689897078702 ) ) ;
#74808 = VERTEX_POINT ( 'NONE', #57616 ) ;
#74809 = EDGE_LOOP ( 'NONE', ( #21662, #53944 ) ) ;
#74810 = ORIENTED_EDGE ( 'NONE', *, *, #98030, .F. ) ;
#74811 = DIRECTION ( 'NONE',  ( 0.000000000000000000, 1.000000000000000000, 0.000000000000000000 ) ) ;
#74812 = DIRECTION ( 'NONE',  ( -0.000000000000000000, 1.000000000000000000, -0.000000000000000000 ) ) ;
#74813 = EDGE_CURVE ( 'NONE', #87854, #91937, #55953, .T. ) ;
#74814 = VECTOR ( 'NONE', #63291, 1000.000000000000000 ) ;
#74815 = CARTESIAN_POINT ( 'NONE',  ( 185.7552083336747444, 6.551208109652275624, -3.782341765624998686 ) ) ;
#74816 = LINE ( 'NONE', #24424, #82434 ) ;
#74817 = CARTESIAN_POINT ( 'NONE',  ( 2.499999999999983569, 2.500000000000000000, -2.276824562219559311E-15 ) ) ;
#74818 = LINE ( 'NONE', #14587, #89985 ) ;
#74819 = DIRECTION ( 'NONE',  ( 0.000000000000000000, 0.000000000000000000, 1.000000000000000000 ) ) ;
#74820 = ORIENTED_EDGE ( 'NONE', *, *, #47603, .T. ) ;
#74821 = CIRCLE ( 'NONE', #7907, 0.06509327318403745899 ) ;
#74822 = AXIS2_PLACEMENT_3D ( 'NONE', #63563, #102813, #30895 ) ;
#74823 = CARTESIAN_POINT ( 'NONE',  ( -2.300000000000033573, 2.500000000000000000, -3.983716857408426293 ) ) ;
#74824 = DIRECTION ( 'NONE',  ( -4.274815082592931898E-19, -0.9999939076577903929, -0.003490651415223739937 ) ) ;
#74825 = ORIENTED_EDGE ( 'NONE', *, *, #96889, .F. ) ;
#74826 = EDGE_CURVE ( 'NONE', #87658, #69489, #129146, .T. ) ;
#74827 = ADVANCED_FACE ( 'NONE', ( #19618 ), #49096, .T. ) ;
#74828 = ADVANCED_FACE ( 'NONE', ( #7847 ), #8486, .T. ) ;
#74829 = EDGE_CURVE ( 'NONE', #90721, #48277, #10084, .T. ) ;
#74830 = AXIS2_PLACEMENT_3D ( 'NONE', #17262, #57217, #127263 ) ;
#74831 = DIRECTION ( 'NONE',  ( -0.000000000000000000, 1.000000000000000000, -0.000000000000000000 ) ) ;
#74832 = CIRCLE ( 'NONE', #127073, 0.1000000000000002554 ) ;
#74833 = AXIS2_PLACEMENT_3D ( 'NONE', #107989, #10436, #28150 ) ;
#74834 = EDGE_LOOP ( 'NONE', ( #106210, #57753, #2075, #23205 ) ) ;
#74835 = EDGE_CURVE ( 'NONE', #37927, #59380, #58121, .T. ) ;
#74836 = DIRECTION ( 'NONE',  ( 0.000000000000000000, -0.9999939076577903929, 0.003490651415223739937 ) ) ;
#74837 = ORIENTED_EDGE ( 'NONE', *, *, #8656, .T. ) ;
#74838 = DIRECTION ( 'NONE',  ( -0.000000000000000000, 1.000000000000000000, -0.000000000000000000 ) ) ;
#74839 = CARTESIAN_POINT ( 'NONE',  ( 10.64999999999991331, 2.500000000000000000, -1.718653347947325827 ) ) ;
#74840 = ADVANCED_FACE ( 'NONE', ( #79198 ), #26808, .T. ) ;
#74841 = DIRECTION ( 'NONE',  ( 0.000000000000000000, 0.000000000000000000, -1.000000000000000000 ) ) ;
#74842 = ORIENTED_EDGE ( 'NONE', *, *, #81555, .F. ) ;
#74843 = ADVANCED_FACE ( 'NONE', ( #29443 ), #93701, .T. ) ;
#74844 = CONICAL_SURFACE ( 'NONE', #58125, 0.1000000000000000472, 0.003490658503988666988 ) ;
#74846 = EDGE_CURVE ( 'NONE', #49848, #75839, #5857, .T. ) ;
#74845 = FACE_OUTER_BOUND ( 'NONE', #52352, .T. ) ;
#74847 = CARTESIAN_POINT ( 'NONE',  ( 186.6250000000000000, -8.891194145520236347, -1.633285867636356299E-15 ) ) ;
#74848 = CIRCLE ( 'NONE', #45615, 0.09999999999999982514 ) ;
#74849 = ADVANCED_FACE ( 'NONE', ( #117142 ), #100117, .T. ) ;
#74850 = ORIENTED_EDGE ( 'NONE', *, *, #34460, .T. ) ;
#74851 = CARTESIAN_POINT ( 'NONE',  ( -5.450000000000019718, 12.50000000000000000, 6.430097255199259010 ) ) ;
#74852 = VECTOR ( 'NONE', #6388, 1000.000000000000000 ) ;
#74853 = VERTEX_POINT ( 'NONE', #68064 ) ;
#74854 = ORIENTED_EDGE ( 'NONE', *, *, #41147, .F. ) ;
#74855 = AXIS2_PLACEMENT_3D ( 'NONE', #79433, #99065, #129195 ) ;
#74856 = CARTESIAN_POINT ( 'NONE',  ( -5.850000000000022737, 2.500000000000000000, -2.065063509461102065 ) ) ;
#74857 = DIRECTION ( 'NONE',  ( 0.000000000000000000, -0.9999939076577903929, 0.003490651415223739937 ) ) ;
#74858 = ORIENTED_EDGE ( 'NONE', *, *, #11743, .T. ) ;
#74859 = VECTOR ( 'NONE', #74759, 1000.000000000000000 ) ;
#74860 = DIRECTION ( 'NONE',  ( -0.000000000000000000, 1.000000000000000000, -0.000000000000000000 ) ) ;
#74861 = DIRECTION ( 'NONE',  ( -4.274815082592931898E-19, -0.9999939076577903929, -0.003490651415223739937 ) ) ;
#74862 = AXIS2_PLACEMENT_3D ( 'NONE', #77966, #30830, #108070 ) ;
#74863 = ORIENTED_EDGE ( 'NONE', *, *, #84487, .F. ) ;
#74864 = DIRECTION ( 'NONE',  ( 0.000000000000000000, 0.000000000000000000, 1.000000000000000000 ) ) ;
#74865 = LINE ( 'NONE', #115393, #76495 ) ;
#74866 = CIRCLE ( 'NONE', #18428, 0.06509327318403745899 ) ;
#74867 = CARTESIAN_POINT ( 'NONE',  ( 0.6499999999999543920, 2.500000000000000000, 6.148780366869520897 ) ) ;
#74868 = CARTESIAN_POINT ( 'NONE',  ( -13.29999999999999005, 2.500000000000000000, 1.843143693225357538E-15 ) ) ;
#74869 = DIRECTION ( 'NONE',  ( -0.000000000000000000, -1.000000000000000000, -0.000000000000000000 ) ) ;
#74870 = LINE ( 'NONE', #25760, #45176 ) ;
#74871 = AXIS2_PLACEMENT_3D ( 'NONE', #16424, #87121, #125740 ) ;
#74872 = DIRECTION ( 'NONE',  ( -0.000000000000000000, -1.000000000000000000, -0.000000000000000000 ) ) ;
#74873 = VERTEX_POINT ( 'NONE', #37338 ) ;
#74874 = EDGE_LOOP ( 'NONE', ( #16901, #4334 ) ) ;
#74875 = ORIENTED_EDGE ( 'NONE', *, *, #90177, .F. ) ;
#74876 = VERTEX_POINT ( 'NONE', #128294 ) ;
#74877 = CARTESIAN_POINT ( 'NONE',  ( -2.900000000000030109, 2.500000000000000000, 0.7928203230275495672 ) ) ;
#74878 = CARTESIAN_POINT ( 'NONE',  ( 88.00000000000001421, 0.000000000000000000, -8.199999999999999289 ) ) ;
#74879 = DIRECTION ( 'NONE',  ( 0.000000000000000000, 0.000000000000000000, -1.000000000000000000 ) ) ;
#74880 = AXIS2_PLACEMENT_3D ( 'NONE', #122517, #93066, #91120 ) ;
#74881 = VERTEX_POINT ( 'NONE', #118451 ) ;
#74882 = FACE_BOUND ( 'NONE', #23941, .T. ) ;
#74883 = DIRECTION ( 'NONE',  ( 0.000000000000000000, -0.000000000000000000, 1.000000000000000000 ) ) ;
#74884 = CARTESIAN_POINT ( 'NONE',  ( -1.250000000000036193, 12.50000000000000000, 1.472243186433545459 ) ) ;
#74885 = EDGE_CURVE ( 'NONE', #73184, #63382, #108280, .T. ) ;
#74886 = CARTESIAN_POINT ( 'NONE',  ( 8.299999999999922551, 12.50000000000000000, -0.06509327318403980434 ) ) ;
#74888 = CONICAL_SURFACE ( 'NONE', #112550, 0.09999999999999982514, 0.003490658503988666988 ) ;
#74887 = AXIS2_PLACEMENT_3D ( 'NONE', #30685, #66870, #127105 ) ;
#74889 = CARTESIAN_POINT ( 'NONE',  ( -3.950000000000025491, 2.500000000000000000, 6.048780366869521252 ) ) ;
#74890 = EDGE_CURVE ( 'NONE', #27457, #111073, #129243, .T. ) ;
#74891 = FACE_OUTER_BOUND ( 'NONE', #102328, .T. ) ;
#74892 = DIRECTION ( 'NONE',  ( 0.000000000000000000, 1.000000000000000000, 0.000000000000000000 ) ) ;
#74893 = CARTESIAN_POINT ( 'NONE',  ( 12.09999999999990550, 12.50000000000000000, -5.022947341949754119 ) ) ;
#74894 = DIRECTION ( 'NONE',  ( -0.000000000000000000, -1.000000000000000000, -0.000000000000000000 ) ) ;
#74895 = DIRECTION ( 'NONE',  ( 0.000000000000000000, 1.000000000000000000, 0.000000000000000000 ) ) ;
#74897 = EDGE_CURVE ( 'NONE', #40079, #118967, #99972, .T. ) ;
#74896 = DIRECTION ( 'NONE',  ( 0.000000000000000000, 0.000000000000000000, 1.000000000000000000 ) ) ;
#74898 = ORIENTED_EDGE ( 'NONE', *, *, #108976, .F. ) ;
#74899 = VERTEX_POINT ( 'NONE', #112517 ) ;
#74900 = ORIENTED_EDGE ( 'NONE', *, *, #46316, .T. ) ;
#74901 = VERTEX_POINT ( 'NONE', #21552 ) ;
#74902 = DIRECTION ( 'NONE',  ( -0.000000000000000000, 1.000000000000000000, -0.000000000000000000 ) ) ;
#74903 = ORIENTED_EDGE ( 'NONE', *, *, #88238, .F. ) ;
#74904 = CONICAL_SURFACE ( 'NONE', #56103, 0.1000000000000000472, 0.003490658503988666988 ) ;
#74905 = DIRECTION ( 'NONE',  ( 0.000000000000000000, -0.000000000000000000, 1.000000000000000000 ) ) ;
#74906 = ORIENTED_EDGE ( 'NONE', *, *, #53539, .T. ) ;
#74907 = ORIENTED_EDGE ( 'NONE', *, *, #29790, .T. ) ;
#74908 = AXIS2_PLACEMENT_3D ( 'NONE', #81251, #113931, #112001 ) ;
#74910 = CIRCLE ( 'NONE', #26787, 0.06509327318403743123 ) ;
#74909 = CARTESIAN_POINT ( 'NONE',  ( 10.79999999999991012, 12.50000000000000000, -4.395220292106239768 ) ) ;
#74912 = CARTESIAN_POINT ( 'NONE',  ( 8.949999999999919353, 12.50000000000000000, -6.083687093685488989 ) ) ;
#74911 = VECTOR ( 'NONE', #120323, 1000.000000000000000 ) ;
#74913 = DIRECTION ( 'NONE',  ( -4.274815082592931898E-19, -0.9999939076577903929, -0.003490651415223739937 ) ) ;
#74914 = PLANE ( 'NONE',  #64297 ) ;
#74915 = ORIENTED_EDGE ( 'NONE', *, *, #5457, .F. ) ;
#74916 = AXIS2_PLACEMENT_3D ( 'NONE', #25486, #83776, #94237 ) ;
#74917 = VERTEX_POINT ( 'NONE', #32691 ) ;
#74918 = CIRCLE ( 'NONE', #112661, 0.1000000000000002554 ) ;
#74919 = ORIENTED_EDGE ( 'NONE', *, *, #56962, .F. ) ;
#74921 = ORIENTED_EDGE ( 'NONE', *, *, #90400, .F. ) ;
#74920 = LINE ( 'NONE', #17754, #44769 ) ;
#74922 = PLANE ( 'NONE',  #123621 ) ;
#74923 = EDGE_LOOP ( 'NONE', ( #109521, #3028 ) ) ;
#74924 = VERTEX_POINT ( 'NONE', #52953 ) ;
#74925 = CIRCLE ( 'NONE', #18478, 0.09999999999999982514 ) ;
#74926 = DIRECTION ( 'NONE',  ( -0.000000000000000000, 1.000000000000000000, -0.000000000000000000 ) ) ;
#74927 = AXIS2_PLACEMENT_3D ( 'NONE', #104095, #7165, #47121 ) ;
#74928 = DIRECTION ( 'NONE',  ( -0.000000000000000000, -1.000000000000000000, -0.000000000000000000 ) ) ;
#74929 = CARTESIAN_POINT ( 'NONE',  ( 7.899999999999924860, 12.50000000000000000, 4.330127018922196314 ) ) ;
#74930 = PLANE ( 'NONE',  #29454 ) ;
#74931 = DIRECTION ( 'NONE',  ( 0.000000000000000000, 0.000000000000000000, 1.000000000000000000 ) ) ;
#74932 = VERTEX_POINT ( 'NONE', #92882 ) ;
#74933 = DIRECTION ( 'NONE',  ( 0.000000000000000000, 0.000000000000000000, 1.000000000000000000 ) ) ;
#74934 = CONICAL_SURFACE ( 'NONE', #106235, 0.1000000000000002554, 0.003490658503988666988 ) ;
#74935 = EDGE_LOOP ( 'NONE', ( #124122, #41801, #5767, #18643 ) ) ;
#74936 = FACE_OUTER_BOUND ( 'NONE', #28517, .T. ) ;
#74937 = EDGE_LOOP ( 'NONE', ( #84384, #114027, #84061, #2167 ) ) ;
#74938 = DIRECTION ( 'NONE',  ( 0.000000000000000000, 0.000000000000000000, 1.000000000000000000 ) ) ;
#74939 = CARTESIAN_POINT ( 'NONE',  ( -4.999999999999986677, 12.50000000000000000, 4.265033745738159077 ) ) ;
#74940 = EDGE_CURVE ( 'NONE', #20160, #13428, #3817, .T. ) ;
#74941 = AXIS2_PLACEMENT_3D ( 'NONE', #101034, #52573, #42118 ) ;
#74942 = DIRECTION ( 'NONE',  ( 0.000000000000000000, 1.000000000000000000, 0.000000000000000000 ) ) ;
#74943 = ADVANCED_FACE ( 'NONE', ( #70647 ), #22623, .T. ) ;
#74944 = DIRECTION ( 'NONE',  ( 0.000000000000000000, -0.000000000000000000, 1.000000000000000000 ) ) ;
#74945 = EDGE_LOOP ( 'NONE', ( #29309, #84367, #106340, #23302 ) ) ;
#74947 = VECTOR ( 'NONE', #1849, 1000.000000000000000 ) ;
#74946 = CARTESIAN_POINT ( 'NONE',  ( 1.649999999999951505, 12.50000000000000000, -1.407149913249512663 ) ) ;
#74948 =( GEOMETRIC_REPRESENTATION_CONTEXT ( 3 ) GLOBAL_UNCERTAINTY_ASSIGNED_CONTEXT ( ( #82270 ) ) GLOBAL_UNIT_ASSIGNED_CONTEXT ( ( #92961, #13074, #102127 ) ) REPRESENTATION_CONTEXT ( 'NONE', 'WORKASPACE' ) );
#74949 = DIRECTION ( 'NONE',  ( 0.000000000000000000, 0.000000000000000000, 1.000000000000000000 ) ) ;
#74950 = ORIENTED_EDGE ( 'NONE', *, *, #128959, .T. ) ;
#74951 = ORIENTED_EDGE ( 'NONE', *, *, #62139, .T. ) ;
#74953 = VERTEX_POINT ( 'NONE', #30751 ) ;
#74952 = EDGE_CURVE ( 'NONE', #125908, #79919, #113148, .T. ) ;
#74954 = CARTESIAN_POINT ( 'NONE',  ( -4.550000000000022915, 12.50000000000000000, 6.560283801567334372 ) ) ;
#74955 = DIRECTION ( 'NONE',  ( 0.000000000000000000, 0.000000000000000000, -1.000000000000000000 ) ) ;
#74956 = CARTESIAN_POINT ( 'NONE',  ( 184.2760416670080588, 6.551208109652274736, 3.782341765625001351 ) ) ;
#74958 = AXIS2_PLACEMENT_3D ( 'NONE', #74929, #43550, #25169 ) ;
#74957 = DIRECTION ( 'NONE',  ( -0.000000000000000000, 1.000000000000000000, -0.000000000000000000 ) ) ;
#74959 = DIRECTION ( 'NONE',  ( 0.000000000000000000, 0.000000000000000000, 1.000000000000000000 ) ) ;
#74960 = DIRECTION ( 'NONE',  ( -0.000000000000000000, -1.000000000000000000, -0.000000000000000000 ) ) ;
#74961 = CIRCLE ( 'NONE', #26842, 0.1000000000000002554 ) ;
#74962 = VERTEX_POINT ( 'NONE', #110572 ) ;
#74963 = DIRECTION ( 'NONE',  ( 0.000000000000000000, 1.000000000000000000, 0.000000000000000000 ) ) ;
#74964 = EDGE_CURVE ( 'NONE', #99874, #36233, #43548, .T. ) ;
#74965 = ORIENTED_EDGE ( 'NONE', *, *, #92853, .F. ) ;
#74966 = CARTESIAN_POINT ( 'NONE',  ( -13.74999999999998934, 2.500000000000000000, 2.857883832488652853 ) ) ;
#74967 = CARTESIAN_POINT ( 'NONE',  ( -12.09999999999999609, 12.50000000000000000, 4.330127018922196314 ) ) ;
#74968 = DIRECTION ( 'NONE',  ( 0.000000000000000000, 0.000000000000000000, 1.000000000000000000 ) ) ;
#74969 = EDGE_LOOP ( 'NONE', ( #22747, #103487 ) ) ;
#74970 = ADVANCED_FACE ( 'NONE', ( #73232 ), #85288, .T. ) ;
#74972 = CIRCLE ( 'NONE', #12262, 0.1000000000000000472 ) ;
#74971 = AXIS2_PLACEMENT_3D ( 'NONE', #4179, #44124, #24487 ) ;
#74973 = CARTESIAN_POINT ( 'NONE',  ( 127.5000000000000000, -2.000000000000000000, -1.999999999999998224 ) ) ;
#74974 = CARTESIAN_POINT ( 'NONE',  ( -6.450000000000016165, 2.500000000000000000, 6.841600689897072485 ) ) ;
#74975 = ADVANCED_FACE ( 'NONE', ( #42497 ), #83062, .T. ) ;
#74976 = EDGE_CURVE ( 'NONE', #122967, #25509, #56035, .T. ) ;
#74977 = EDGE_CURVE ( 'NONE', #121192, #25178, #45597, .T. ) ;
#74978 = EDGE_CURVE ( 'NONE', #77678, #58293, #92210, .T. ) ;
#74979 = ORIENTED_EDGE ( 'NONE', *, *, #42173, .T. ) ;
#74980 = FACE_OUTER_BOUND ( 'NONE', #125537, .T. ) ;
#74981 = ORIENTED_EDGE ( 'NONE', *, *, #5274, .F. ) ;
#74982 = EDGE_LOOP ( 'NONE', ( #24514, #38344 ) ) ;
#74983 = DIRECTION ( 'NONE',  ( -0.000000000000000000, 1.000000000000000000, -0.000000000000000000 ) ) ;
#74984 = EDGE_CURVE ( 'NONE', #90660, #12748, #70716, .T. ) ;
#74985 = CIRCLE ( 'NONE', #54156, 0.06509327318403745899 ) ;
#74986 = EDGE_CURVE ( 'NONE', #35098, #78690, #62133, .T. ) ;
#74987 = ORIENTED_EDGE ( 'NONE', *, *, #96981, .T. ) ;
#74988 = FACE_OUTER_BOUND ( 'NONE', #47506, .T. ) ;
#74989 = LINE ( 'NONE', #114898, #121615 ) ;
#74990 = PLANE ( 'NONE',  #100294 ) ;
#74991 = ORIENTED_EDGE ( 'NONE', *, *, #9217, .T. ) ;
#74992 = EDGE_CURVE ( 'NONE', #125017, #15707, #49809, .T. ) ;
#74993 = AXIS2_PLACEMENT_3D ( 'NONE', #103312, #23451, #111167 ) ;
#74995 = EDGE_CURVE ( 'NONE', #65424, #126915, #41399, .T. ) ;
#74994 = FACE_BOUND ( 'NONE', #86504, .T. ) ;
#74996 = VECTOR ( 'NONE', #99103, 1000.000000000000000 ) ;
#74997 = CIRCLE ( 'NONE', #18561, 0.06509327318403745899 ) ;
#74998 = DIRECTION ( 'NONE',  ( 0.000000000000000000, 0.000000000000000000, 1.000000000000000000 ) ) ;
#75000 = VERTEX_POINT ( 'NONE', #51027 ) ;
#74999 = CARTESIAN_POINT ( 'NONE',  ( 3.149999999999944400, 2.500000000000000000, 1.918653347947321564 ) ) ;
#75001 = CARTESIAN_POINT ( 'NONE',  ( 3.949999999999942446, 2.500000000000000000, -2.411473670974877859 ) ) ;
#75002 = DIRECTION ( 'NONE',  ( 0.000000000000000000, 0.000000000000000000, 1.000000000000000000 ) ) ;
#75003 = EDGE_CURVE ( 'NONE', #33429, #18914, #63412, .T. ) ;
#75004 = CIRCLE ( 'NONE', #43624, 0.06509327318403745899 ) ;
#75005 = ORIENTED_EDGE ( 'NONE', *, *, #11658, .F. ) ;
#75006 = AXIS2_PLACEMENT_3D ( 'NONE', #17603, #57547, #28084 ) ;
#75007 = CIRCLE ( 'NONE', #39533, 0.06509327318403745899 ) ;
#75008 = ORIENTED_EDGE ( 'NONE', *, *, #99561, .F. ) ;
#75009 = ORIENTED_EDGE ( 'NONE', *, *, #117795, .T. ) ;
#75010 = CARTESIAN_POINT ( 'NONE',  ( 5.849999999999932143, 2.500000000000000000, 1.572243186433545548 ) ) ;
#75011 = DIRECTION ( 'NONE',  ( 0.000000000000000000, 1.000000000000000000, 0.000000000000000000 ) ) ;
#75012 = CARTESIAN_POINT ( 'NONE',  ( -12.09999999999999432, 2.500000000000000000, 5.122947341949749323 ) ) ;
#75013 = FACE_BOUND ( 'NONE', #67220, .T. ) ;
#75014 = ORIENTED_EDGE ( 'NONE', *, *, #48546, .T. ) ;
#75015 = CARTESIAN_POINT ( 'NONE',  ( 185.1093750003413732, 9.264065473108010111E-16, -7.564683531250000925 ) ) ;
#75016 = CARTESIAN_POINT ( 'NONE',  ( 14.34999999999989662, 12.50000000000000000, 1.818653347947321475 ) ) ;
#75017 = DIRECTION ( 'NONE',  ( -0.000000000000000000, 1.000000000000000000, -0.000000000000000000 ) ) ;
#75018 = VECTOR ( 'NONE', #104579, 1000.000000000000000 ) ;
#75019 = DIRECTION ( 'NONE',  ( 0.000000000000000000, -0.000000000000000000, 1.000000000000000000 ) ) ;
#75020 = CARTESIAN_POINT ( 'NONE',  ( 3.099999999999945466, 12.50000000000000000, 0.4115034346978109769 ) ) ;
#75021 = DIRECTION ( 'NONE',  ( 0.000000000000000000, -0.000000000000000000, 1.000000000000000000 ) ) ;
#75022 = DIRECTION ( 'NONE',  ( 0.000000000000000000, 0.000000000000000000, -1.000000000000000000 ) ) ;
#75023 = DIRECTION ( 'NONE',  ( 0.000000000000000000, 0.000000000000000000, -1.000000000000000000 ) ) ;
#75024 = CIRCLE ( 'NONE', #58311, 0.09999999999999999167 ) ;
#75025 = DIRECTION ( 'NONE',  ( 0.000000000000000000, 1.000000000000000000, 0.000000000000000000 ) ) ;
#75026 = ORIENTED_EDGE ( 'NONE', *, *, #57908, .T. ) ;
#75027 = ORIENTED_EDGE ( 'NONE', *, *, #52894, .T. ) ;
#75028 = VERTEX_POINT ( 'NONE', #111871 ) ;
#75029 = VERTEX_POINT ( 'NONE', #40570 ) ;
#75030 = EDGE_LOOP ( 'NONE', ( #95181, #15709, #108741, #125981 ) ) ;
#75031 = CARTESIAN_POINT ( 'NONE',  ( 10.39999999999991154, 12.50000000000000000, -3.637306695894650055 ) ) ;
#75032 = CARTESIAN_POINT ( 'NONE',  ( -2.500000000000032863, 2.500000000000000000, 4.922947341949748257 ) ) ;
#75033 = ORIENTED_EDGE ( 'NONE', *, *, #97705, .T. ) ;
#75034 = FACE_BOUND ( 'NONE', #101969, .T. ) ;
#75035 = FACE_OUTER_BOUND ( 'NONE', #108890, .T. ) ;
#75036 = EDGE_CURVE ( 'NONE', #37274, #942, #100737, .T. ) ;
#75037 = CIRCLE ( 'NONE', #47862, 0.09999999999999982514 ) ;
#75038 = DIRECTION ( 'NONE',  ( 0.000000000000000000, 0.000000000000000000, 1.000000000000000000 ) ) ;
#75039 = ADVANCED_FACE ( 'NONE', ( #22218 ), #112493, .T. ) ;
#75040 = EDGE_LOOP ( 'NONE', ( #37201, #112476 ) ) ;
#75041 = CARTESIAN_POINT ( 'NONE',  ( 4.999999999999936939, 12.50000000000000000, -3.572213422710612374 ) ) ;
#75042 = CARTESIAN_POINT ( 'NONE',  ( 9.599999999999914380, 2.500000000000000000, -4.230127018922201998 ) ) ;
#75043 = DIRECTION ( 'NONE',  ( -4.274815082592931898E-19, -0.9999939076577903929, -0.003490651415223739937 ) ) ;
#75044 = EDGE_LOOP ( 'NONE', ( #83290, #26214 ) ) ;
#75045 = CONICAL_SURFACE ( 'NONE', #18608, 0.1000000000000002554, 0.003490658503988666988 ) ;
#75046 = DIRECTION ( 'NONE',  ( 0.000000000000000000, -0.9999939076577903929, 0.003490651415223739937 ) ) ;
#75048 = ORIENTED_EDGE ( 'NONE', *, *, #60760, .F. ) ;
#75047 = AXIS2_PLACEMENT_3D ( 'NONE', #37335, #117784, #117139 ) ;
#75049 = EDGE_LOOP ( 'NONE', ( #89114, #80942, #75911, #93948 ) ) ;
#75050 = ORIENTED_EDGE ( 'NONE', *, *, #58369, .T. ) ;
#75051 = DIRECTION ( 'NONE',  ( 0.000000000000000000, 0.000000000000000000, 1.000000000000000000 ) ) ;
#75052 = CARTESIAN_POINT ( 'NONE',  ( -4.600000000000025402, 2.500000000000000000, -2.385244779468109755E-15 ) ) ;
#75053 = LINE ( 'NONE', #25956, #94805 ) ;
#75054 = CONICAL_SURFACE ( 'NONE', #98029, 0.09999999999999982514, 0.003490658503988666988 ) ;
#75055 = ORIENTED_EDGE ( 'NONE', *, *, #9351, .T. ) ;
#75056 = CARTESIAN_POINT ( 'NONE',  ( 3.710216157319381924, 2.500000000002297718, -9.999999999875349488 ) ) ;
#75057 = DIRECTION ( 'NONE',  ( 0.000000000000000000, -0.9999939076577903929, 0.003490651415223739937 ) ) ;
#75059 = AXIS2_PLACEMENT_3D ( 'NONE', #71960, #2540, #51035 ) ;
#75058 = DIRECTION ( 'NONE',  ( -0.000000000000000000, -1.000000000000000000, -0.000000000000000000 ) ) ;
#75060 = CARTESIAN_POINT ( 'NONE',  ( 183.9062500006828031, -8.891194145520236347, -1.633285867636356693E-15 ) ) ;
#75061 = DIRECTION ( 'NONE',  ( 0.000000000000000000, 1.000000000000000000, 0.000000000000000000 ) ) ;
#75062 = AXIS2_PLACEMENT_3D ( 'NONE', #99195, #31736, #11444 ) ;
#75063 = DIRECTION ( 'NONE',  ( 0.000000000000000000, -0.000000000000000000, 1.000000000000000000 ) ) ;
#75064 = EDGE_LOOP ( 'NONE', ( #70106, #47564 ) ) ;
#75065 = CARTESIAN_POINT ( 'NONE',  ( -2.499999999999996447, 2.500000000000000000, 4.430127018922196847 ) ) ;
#75067 = AXIS2_PLACEMENT_3D ( 'NONE', #92698, #32514, #112341 ) ;
#75066 = AXIS2_PLACEMENT_3D ( 'NONE', #82367, #122286, #32639 ) ;
#75068 = ORIENTED_EDGE ( 'NONE', *, *, #16235, .T. ) ;
#75069 = ORIENTED_EDGE ( 'NONE', *, *, #99768, .T. ) ;
#75070 = DIRECTION ( 'NONE',  ( 0.000000000000000000, 1.000000000000000000, 0.000000000000000000 ) ) ;
#75071 = DIRECTION ( 'NONE',  ( 0.000000000000000000, 0.000000000000000000, -1.000000000000000000 ) ) ;
#75072 = DIRECTION ( 'NONE',  ( 0.000000000000000000, -0.9999939076577903929, 0.003490651415223739937 ) ) ;
#75073 = CARTESIAN_POINT ( 'NONE',  ( 13.54999999999989946, 12.50000000000000000, 2.511473670974873507 ) ) ;
#75074 = CARTESIAN_POINT ( 'NONE',  ( 3.149999999999944400, 2.500000000000000000, 2.511473670974873507 ) ) ;
#75075 = ORIENTED_EDGE ( 'NONE', *, *, #8992, .F. ) ;
#75076 = VERTEX_POINT ( 'NONE', #83176 ) ;
#75077 = EDGE_CURVE ( 'NONE', #70759, #49015, #127166, .T. ) ;
#75078 = FACE_OUTER_BOUND ( 'NONE', #116314, .T. ) ;
#75079 = DIRECTION ( 'NONE',  ( 0.000000000000000000, 0.000000000000000000, -1.000000000000000000 ) ) ;
#75080 = PLANE ( 'NONE',  #121300 ) ;
#75082 = ORIENTED_EDGE ( 'NONE', *, *, #17978, .F. ) ;
#75081 = AXIS2_PLACEMENT_3D ( 'NONE', #17544, #76491, #35910 ) ;
#75083 = ORIENTED_EDGE ( 'NONE', *, *, #68637, .T. ) ;
#75084 = DIRECTION ( 'NONE',  ( -4.274815082592931898E-19, -0.9999939076577903929, -0.003490651415223739937 ) ) ;
#75085 = VERTEX_POINT ( 'NONE', #63533 ) ;
#75086 = CARTESIAN_POINT ( 'NONE',  ( -1.650000000000034772, 2.500000000000000000, 1.372243186433545370 ) ) ;
#75087 = CIRCLE ( 'NONE', #64615, 0.06509327318403745899 ) ;
#75089 = DIRECTION ( 'NONE',  ( 0.000000000000000000, 1.000000000000000000, 0.000000000000000000 ) ) ;
#75088 = AXIS2_PLACEMENT_3D ( 'NONE', #107299, #107953, #89601 ) ;
#75090 = ORIENTED_EDGE ( 'NONE', *, *, #29787, .T. ) ;
#75091 = PLANE ( 'NONE',  #127597 ) ;
#75092 = DIRECTION ( 'NONE',  ( -4.274815082592931898E-19, -0.9999939076577903929, -0.003490651415223739937 ) ) ;
#75093 = FACE_OUTER_BOUND ( 'NONE', #39009, .T. ) ;
#75094 = ADVANCED_FACE ( 'NONE', ( #73331 ), #42617, .T. ) ;
#75095 = EDGE_CURVE ( 'NONE', #34711, #105977, #125005, .T. ) ;
#75096 = DIRECTION ( 'NONE',  ( 0.000000000000000000, 0.000000000000000000, 1.000000000000000000 ) ) ;
#75097 = AXIS2_PLACEMENT_3D ( 'NONE', #4745, #2183, #44706 ) ;
#75098 = ORIENTED_EDGE ( 'NONE', *, *, #88513, .F. ) ;
#75099 = AXIS2_PLACEMENT_3D ( 'NONE', #95380, #5691, #72531 ) ;
#75101 = DIRECTION ( 'NONE',  ( -0.000000000000000000, -1.000000000000000000, -0.000000000000000000 ) ) ;
#75100 = CIRCLE ( 'NONE', #91827, 0.1000000000000002554 ) ;
#75102 = DIRECTION ( 'NONE',  ( -4.274815082592931898E-19, -0.9999939076577903929, -0.003490651415223739937 ) ) ;
#75103 = EDGE_LOOP ( 'NONE', ( #124424, #109074 ) ) ;
#75104 = ORIENTED_EDGE ( 'NONE', *, *, #106281, .T. ) ;
#75105 = EDGE_CURVE ( 'NONE', #10740, #65870, #87430, .T. ) ;
#75106 = FACE_OUTER_BOUND ( 'NONE', #124771, .T. ) ;
#75107 = CARTESIAN_POINT ( 'NONE',  ( 12.49999999999990230, 2.500000000000000000, -0.6928203230275541413 ) ) ;
#75108 = FACE_OUTER_BOUND ( 'NONE', #59083, .T. ) ;
#75109 = AXIS2_PLACEMENT_3D ( 'NONE', #92551, #19957, #101738 ) ;
#75110 = CARTESIAN_POINT ( 'NONE',  ( 4.349999999999940137, 12.50000000000000000, -2.511473670974877948 ) ) ;
#75111 = CARTESIAN_POINT ( 'NONE',  ( -5.400000000000024336, 12.50000000000000000, -3.637306695894650055 ) ) ;
#75112 = VECTOR ( 'NONE', #107961, 1000.000000000000000 ) ;
#75113 = DIRECTION ( 'NONE',  ( -0.000000000000000000, 1.000000000000000000, -0.000000000000000000 ) ) ;
#75114 = DIRECTION ( 'NONE',  ( -0.000000000000000000, 1.000000000000000000, -0.000000000000000000 ) ) ;
#75115 = LINE ( 'NONE', #25347, #89611 ) ;
#75116 = CARTESIAN_POINT ( 'NONE',  ( -7.100000000000017408, 2.500000000000000000, -0.6928203230275542523 ) ) ;
#75117 = DIRECTION ( 'NONE',  ( -0.000000000000000000, -1.000000000000000000, -0.000000000000000000 ) ) ;
#75118 = VERTEX_POINT ( 'NONE', #32796 ) ;
#75119 = EDGE_LOOP ( 'NONE', ( #79036, #114272 ) ) ;
#75120 = CONICAL_SURFACE ( 'NONE', #18681, 0.1000000000000000472, 0.003490658503988666988 ) ;
#75121 = ORIENTED_EDGE ( 'NONE', *, *, #19557, .F. ) ;
#75122 = DIRECTION ( 'NONE',  ( -0.000000000000000000, 1.000000000000000000, -0.000000000000000000 ) ) ;
#75123 = CARTESIAN_POINT ( 'NONE',  ( 7.499999999999927169, 12.50000000000000000, 3.637306695894644726 ) ) ;
#75124 = CARTESIAN_POINT ( 'NONE',  ( -7.700000000000014388, 2.500000000000000000, -0.3464101615137782364 ) ) ;
#75125 = ORIENTED_EDGE ( 'NONE', *, *, #46021, .F. ) ;
#75126 = CARTESIAN_POINT ( 'NONE',  ( 3.749999999999944045, 2.500000000000000000, -2.957883832488653830 ) ) ;
#75127 = EDGE_CURVE ( 'NONE', #4337, #39809, #2648, .T. ) ;
#75128 = CARTESIAN_POINT ( 'NONE',  ( 11.04999999999991189, 2.500000000000000000, 6.148780366869520897 ) ) ;
#75130 = ORIENTED_EDGE ( 'NONE', *, *, #6534, .T. ) ;
#75129 = DIRECTION ( 'NONE',  ( 0.000000000000000000, -0.000000000000000000, 1.000000000000000000 ) ) ;
#75131 = EDGE_CURVE ( 'NONE', #97166, #74962, #22961, .T. ) ;
#75132 = AXIS2_PLACEMENT_3D ( 'NONE', #23749, #32941, #53846 ) ;
#75133 = EDGE_CURVE ( 'NONE', #47787, #67958, #28874, .T. ) ;
#75134 = CARTESIAN_POINT ( 'NONE',  ( -3.100000000000028955, 12.50000000000000000, 4.676537180435972552 ) ) ;
#75135 = ORIENTED_EDGE ( 'NONE', *, *, #57739, .F. ) ;
#75136 = VERTEX_POINT ( 'NONE', #34073 ) ;
#75137 = EDGE_LOOP ( 'NONE', ( #102499, #4678, #22483, #54454 ) ) ;
#75138 = EDGE_LOOP ( 'NONE', ( #47555, #77519, #41605, #103237 ) ) ;
#75139 = DIRECTION ( 'NONE',  ( 0.000000000000000000, 1.000000000000000000, 0.000000000000000000 ) ) ;
#75140 = ADVANCED_FACE ( 'NONE', ( #13763 ), #24752, .T. ) ;
#75141 = EDGE_CURVE ( 'NONE', #64674, #5452, #81190, .T. ) ;
#75142 = CIRCLE ( 'NONE', #123262, 0.1000000000000000472 ) ;
#75143 = ADVANCED_FACE ( 'NONE', ( #112632 ), #123046, .T. ) ;
#75144 = EDGE_CURVE ( 'NONE', #81046, #107875, #102163, .T. ) ;
#75145 = DIRECTION ( 'NONE',  ( -0.000000000000000000, -1.000000000000000000, -0.000000000000000000 ) ) ;
#75146 = PLANE ( 'NONE',  #88050 ) ;
#75147 = CARTESIAN_POINT ( 'NONE',  ( -12.69999999999999218, 12.50000000000000000, 4.676537180435972552 ) ) ;
#75148 = ORIENTED_EDGE ( 'NONE', *, *, #112374, .T. ) ;
#75151 = ADVANCED_FACE ( 'NONE', ( #13111 ), #54087, .T. ) ;
#75150 = CONICAL_SURFACE ( 'NONE', #16635, 0.09999999999999982514, 0.003490658503988666988 ) ;
#75149 = CONICAL_SURFACE ( 'NONE', #60502, 0.1000000000000000472, 0.003490658503988666988 ) ;
#75152 = DIRECTION ( 'NONE',  ( -0.000000000000000000, -1.000000000000000000, -0.000000000000000000 ) ) ;
#75153 = ORIENTED_EDGE ( 'NONE', *, *, #54873, .F. ) ;
#75154 = CARTESIAN_POINT ( 'NONE',  ( 3.549999999999943867, 2.500000000000000000, -6.048780366869526581 ) ) ;
#75156 = VECTOR ( 'NONE', #116088, 1000.000000000000000 ) ;
#75155 = CARTESIAN_POINT ( 'NONE',  ( 9.549999999999918998, 12.50000000000000000, -6.495190528383302464 ) ) ;
#75157 = DIRECTION ( 'NONE',  ( 0.000000000000000000, 1.000000000000000000, 0.000000000000000000 ) ) ;
#75158 = CARTESIAN_POINT ( 'NONE',  ( 18.98912670146762594, -2.543039972613341693, 4.488908218019908247 ) ) ;
#75159 = EDGE_CURVE ( 'NONE', #42013, #54592, #95856, .T. ) ;
#75160 = ORIENTED_EDGE ( 'NONE', *, *, #103331, .F. ) ;
#75162 = AXIS2_PLACEMENT_3D ( 'NONE', #16046, #55981, #95914 ) ;
#75161 = CONICAL_SURFACE ( 'NONE', #89816, 0.1000000000000002554, 0.003490658503988666988 ) ;
#75163 = ORIENTED_EDGE ( 'NONE', *, *, #43119, .F. ) ;
#75164 = EDGE_LOOP ( 'NONE', ( #75480, #116932, #73696, #93400, #26448 ) ) ;
#75165 = DIRECTION ( 'NONE',  ( 0.000000000000000000, 0.000000000000000000, -1.000000000000000000 ) ) ;
#75166 = CARTESIAN_POINT ( 'NONE',  ( -3.350000000000028511, 12.50000000000000000, -2.857883832488653741 ) ) ;
#75167 = DIRECTION ( 'NONE',  ( -0.000000000000000000, 1.000000000000000000, -0.000000000000000000 ) ) ;
#75168 = FACE_BOUND ( 'NONE', #26828, .T. ) ;
#75169 = CARTESIAN_POINT ( 'NONE',  ( 5.849999999999933031, 12.50000000000000000, 7.253104124594885960 ) ) ;
#75170 = CARTESIAN_POINT ( 'NONE',  ( 6.849999999999927702, 12.50000000000000000, 2.576566944158910744 ) ) ;
#75171 = DIRECTION ( 'NONE',  ( 0.000000000000000000, 0.000000000000000000, 1.000000000000000000 ) ) ;
#75172 = LINE ( 'NONE', #95459, #123692 ) ;
#75173 = DIRECTION ( 'NONE',  ( 0.000000000000000000, 0.000000000000000000, 1.000000000000000000 ) ) ;
#75174 = CARTESIAN_POINT ( 'NONE',  ( 186.7812500006828031, 0.000000000000000000, 7.700000000000000178 ) ) ;
#75175 = ORIENTED_EDGE ( 'NONE', *, *, #113084, .T. ) ;
#75176 = AXIS2_PLACEMENT_3D ( 'NONE', #29118, #50668, #59876 ) ;
#75177 = AXIS2_PLACEMENT_3D ( 'NONE', #24728, #23430, #63366 ) ;
#75178 = CARTESIAN_POINT ( 'NONE',  ( -13.94999999999998685, 12.50000000000000000, 1.818653347947325472 ) ) ;
#75179 = EDGE_LOOP ( 'NONE', ( #103335, #27757 ) ) ;
#75180 = EDGE_LOOP ( 'NONE', ( #123117, #119512, #112768, #66530 ) ) ;
#75181 = ORIENTED_EDGE ( 'NONE', *, *, #21714, .F. ) ;
#75182 = ORIENTED_EDGE ( 'NONE', *, *, #65735, .F. ) ;
#75183 = DIRECTION ( 'NONE',  ( 0.000000000000000000, -0.9999939076577903929, 0.003490651415223739937 ) ) ;
#75184 = FACE_BOUND ( 'NONE', #77906, .T. ) ;
#75185 = CARTESIAN_POINT ( 'NONE',  ( -1.850000000000033840, 2.500000000000000000, 1.818653347947321475 ) ) ;
#75186 = CONICAL_SURFACE ( 'NONE', #100231, 0.1000000000000000472, 0.003490658503988666988 ) ;
#75188 = AXIS2_PLACEMENT_3D ( 'NONE', #1339, #48518, #28887 ) ;
#75187 = CONICAL_SURFACE ( 'NONE', #29234, 0.1000000000000002554, 0.003490658503988666988 ) ;
#75189 = ADVANCED_FACE ( 'NONE', ( #121153 ), #114719, .T. ) ;
#75190 = ORIENTED_EDGE ( 'NONE', *, *, #35060, .F. ) ;
#75191 = CARTESIAN_POINT ( 'NONE',  ( 87.49999999944498086, 3.974992050012154277, 6.359987280019447020 ) ) ;
#75192 = DIRECTION ( 'NONE',  ( 0.000000000000000000, 0.000000000000000000, -1.000000000000000000 ) ) ;
#75193 = CONICAL_SURFACE ( 'NONE', #125366, 0.1000000000000002554, 0.003490658503988666988 ) ;
#75194 = VERTEX_POINT ( 'NONE', #52410 ) ;
#75195 = CARTESIAN_POINT ( 'NONE',  ( 8.149999999999923972, 12.50000000000000000, -6.148780366869526226 ) ) ;
#75196 = CARTESIAN_POINT ( 'NONE',  ( -5.400000000000019895, 2.500000000000000000, 3.637306695894644726 ) ) ;
#75197 = ADVANCED_FACE ( 'NONE', ( #21674 ), #58305, .T. ) ;
#75198 = CIRCLE ( 'NONE', #119023, 0.09999999999999999167 ) ;
#75199 = AXIS2_PLACEMENT_3D ( 'NONE', #83374, #5435, #84655 ) ;
#75200 = ORIENTED_EDGE ( 'NONE', *, *, #102176, .F. ) ;
#75201 = DIRECTION ( 'NONE',  ( 0.000000000000000000, 0.000000000000000000, 1.000000000000000000 ) ) ;
#75202 = LINE ( 'NONE', #104021, #49694 ) ;
#75203 = CONICAL_SURFACE ( 'NONE', #18765, 0.1000000000000002554, 0.003490658503988666988 ) ;
#75204 = VERTEX_POINT ( 'NONE', #11833 ) ;
#75205 = DIRECTION ( 'NONE',  ( -0.000000000000000000, 1.000000000000000000, -0.000000000000000000 ) ) ;
#75206 = CARTESIAN_POINT ( 'NONE',  ( -0.8500000000000390576, 2.500000000000000000, -6.495190528383302464 ) ) ;
#75207 = CARTESIAN_POINT ( 'NONE',  ( 2.699999999999947331, 12.50000000000000000, -0.4115034346978157509 ) ) ;
#75208 = VECTOR ( 'NONE', #60443, 1000.000000000000000 ) ;
#75209 = ORIENTED_EDGE ( 'NONE', *, *, #56897, .F. ) ;
#75210 = ORIENTED_EDGE ( 'NONE', *, *, #30560, .T. ) ;
#75211 = DIRECTION ( 'NONE',  ( -4.274815082592931898E-19, -0.9999939076577903929, -0.003490651415223739937 ) ) ;
#75212 = ORIENTED_EDGE ( 'NONE', *, *, #32226, .F. ) ;
#75213 = FACE_OUTER_BOUND ( 'NONE', #11502, .T. ) ;
#75214 = DIRECTION ( 'NONE',  ( 0.000000000000000000, 0.000000000000000000, 1.000000000000000000 ) ) ;
#75215 = ORIENTED_EDGE ( 'NONE', *, *, #64067, .T. ) ;
#75216 = CARTESIAN_POINT ( 'NONE',  ( 109.6452891074249720, 6.075908156944702654, -4.732659750966558221 ) ) ;
#75217 = DIRECTION ( 'NONE',  ( -0.000000000000000000, -1.000000000000000000, -0.000000000000000000 ) ) ;
#75218 = DIRECTION ( 'NONE',  ( 0.000000000000000000, -0.9999939076577903929, 0.003490651415223739937 ) ) ;
#75219 = CARTESIAN_POINT ( 'NONE',  ( -5.600000000000023626, 12.50000000000000000, -3.983716857408426293 ) ) ;
#75220 = DIRECTION ( 'NONE',  ( 0.000000000000000000, -0.9999939076577903929, 0.003490651415223739937 ) ) ;
#75221 = ORIENTED_EDGE ( 'NONE', *, *, #52997, .T. ) ;
#75223 = EDGE_LOOP ( 'NONE', ( #86012, #60031 ) ) ;
#75222 = EDGE_CURVE ( 'NONE', #179, #49864, #102115, .T. ) ;
#75224 = PLANE ( 'NONE',  #18155 ) ;
#75225 = CARTESIAN_POINT ( 'NONE',  ( 17.91370874550463554, -0.4812889678259977266, 4.985910759330125508 ) ) ;
#75226 = DIRECTION ( 'NONE',  ( 0.000000000000000000, 0.000000000000000000, -1.000000000000000000 ) ) ;
#75228 = EDGE_LOOP ( 'NONE', ( #35958, #129358, #1325, #68419 ) ) ;
#75227 = ORIENTED_EDGE ( 'NONE', *, *, #72783, .F. ) ;
#75229 = VERTEX_POINT ( 'NONE', #81859 ) ;
#75230 = AXIS2_PLACEMENT_3D ( 'NONE', #49013, #9717, #49660 ) ;
#75231 = DIRECTION ( 'NONE',  ( -0.000000000000000000, -1.000000000000000000, -0.000000000000000000 ) ) ;
#75233 = ADVANCED_FACE ( 'NONE', ( #62249 ), #76571, .T. ) ;
#75232 = CARTESIAN_POINT ( 'NONE',  ( -5.850000000000018296, 2.500000000000000000, 1.472243186433545459 ) ) ;
#75234 = CARTESIAN_POINT ( 'NONE',  ( 5.849999999999933920, 12.50000000000000000, 5.802370205355744659 ) ) ;
#75236 = AXIS2_PLACEMENT_3D ( 'NONE', #125403, #75636, #45566 ) ;
#75235 = AXIS2_PLACEMENT_3D ( 'NONE', #69006, #95899, #67714 ) ;
#75237 = DIRECTION ( 'NONE',  ( 0.000000000000000000, 0.000000000000000000, 1.000000000000000000 ) ) ;
#75238 = CARTESIAN_POINT ( 'NONE',  ( -3.150000000000030553, 12.50000000000000000, 6.213873640053558134 ) ) ;
#75239 = CARTESIAN_POINT ( 'NONE',  ( -5.650000000000019895, 2.500000000000000000, 2.611473670974873151 ) ) ;
#75240 = FACE_OUTER_BOUND ( 'NONE', #120591, .T. ) ;
#75241 = CARTESIAN_POINT ( 'NONE',  ( -3.150000000000029665, 12.50000000000000000, 6.841600689897072485 ) ) ;
#75242 = EDGE_CURVE ( 'NONE', #116514, #109859, #74629, .T. ) ;
#75243 = ADVANCED_FACE ( 'NONE', ( #26184 ), #36664, .T. ) ;
#75244 = CARTESIAN_POINT ( 'NONE',  ( -5.200000000000020606, 2.500000000000000000, -0.4464101615137782142 ) ) ;
#75246 = CONICAL_SURFACE ( 'NONE', #79184, 0.1000000000000000472, 0.003490658503988666988 ) ;
#75245 = CIRCLE ( 'NONE', #91973, 0.1000000000000002554 ) ;
#75247 = VERTEX_POINT ( 'NONE', #15692 ) ;
#75248 = ADVANCED_FACE ( 'NONE', ( #86375 ), #112587, .T. ) ;
#75249 = DIRECTION ( 'NONE',  ( -4.274815082592931898E-19, -0.9999939076577903929, -0.003490651415223739937 ) ) ;
#75250 = VERTEX_POINT ( 'NONE', #16330 ) ;
#75251 = ORIENTED_EDGE ( 'NONE', *, *, #98158, .T. ) ;
#75252 = ADVANCED_FACE ( 'NONE', ( #114542 ), #41593, .T. ) ;
#75253 = CARTESIAN_POINT ( 'NONE',  ( 7.899999999999924860, 12.50000000000000000, -3.637306695894650055 ) ) ;
#75254 = CARTESIAN_POINT ( 'NONE',  ( 4.399999999999937295, 2.500000000000000000, 4.083716857408421497 ) ) ;
#75255 = DIRECTION ( 'NONE',  ( 0.000000000000000000, 1.000000000000000000, 0.000000000000000000 ) ) ;
#75256 = DIRECTION ( 'NONE',  ( 0.000000000000000000, 1.000000000000000000, 0.000000000000000000 ) ) ;
#75257 = CARTESIAN_POINT ( 'NONE',  ( 5.399999999999932854, 2.500000000000000000, 5.022947341949748790 ) ) ;
#75258 = DIRECTION ( 'NONE',  ( 0.000000000000000000, -0.9999939076577903929, 0.003490651415223739937 ) ) ;
#75259 = ORIENTED_EDGE ( 'NONE', *, *, #106176, .T. ) ;
#75260 = CARTESIAN_POINT ( 'NONE',  ( 0.000000000000000000, 0.000000000000000000, 6.000000000000005329 ) ) ;
#75261 = CARTESIAN_POINT ( 'NONE',  ( 4.599999999999935696, 2.500000000000000000, 4.922947341949748257 ) ) ;
#75262 = EDGE_LOOP ( 'NONE', ( #100882, #42307 ) ) ;
#75263 = AXIS2_PLACEMENT_3D ( 'NONE', #105994, #56867, #117720 ) ;
#75265 = ORIENTED_EDGE ( 'NONE', *, *, #50132, .T. ) ;
#75264 = CONICAL_SURFACE ( 'NONE', #52291, 0.1000000000000002554, 0.003490658503988666988 ) ;
#75266 = ORIENTED_EDGE ( 'NONE', *, *, #31336, .T. ) ;
#75267 = EDGE_LOOP ( 'NONE', ( #93111, #102870 ) ) ;
#75268 = DIRECTION ( 'NONE',  ( -0.000000000000000000, -1.000000000000000000, -0.000000000000000000 ) ) ;
#75269 = CARTESIAN_POINT ( 'NONE',  ( 7.299999999999924327, 2.500000000000000000, 0.4464101615137735513 ) ) ;
#75270 = CIRCLE ( 'NONE', #18835, 0.06509327318403743123 ) ;
#75271 = CARTESIAN_POINT ( 'NONE',  ( -3.150000000000029221, 12.50000000000000000, -1.818653347947326138 ) ) ;
#75272 = CARTESIAN_POINT ( 'NONE',  ( 5.399999999999936406, 12.50000000000000000, -4.957854068765716882 ) ) ;
#75273 = CARTESIAN_POINT ( 'NONE',  ( -4.800000000000024691, 2.500000000000000000, 0.2464101615137735679 ) ) ;
#75274 = EDGE_LOOP ( 'NONE', ( #5359, #38401 ) ) ;
#75275 = CARTESIAN_POINT ( 'NONE',  ( 11.04999999999990834, 2.500000000000000000, -6.841600689897077814 ) ) ;
#75276 = CARTESIAN_POINT ( 'NONE',  ( -4.200000000000029488, 12.50000000000000000, -4.330127018922201643 ) ) ;
#75277 = AXIS2_PLACEMENT_3D ( 'NONE', #3375, #52469, #104157 ) ;
#75278 = ADVANCED_FACE ( 'NONE', ( #124387 ), #77070, .T. ) ;
#75279 = CARTESIAN_POINT ( 'NONE',  ( 6.049999999999932321, 2.500000000000000000, -1.818653347947326138 ) ) ;
#75280 = CIRCLE ( 'NONE', #29248, 0.06509327318403745899 ) ;
#75281 = ORIENTED_EDGE ( 'NONE', *, *, #85632, .T. ) ;
#75282 = AXIS2_PLACEMENT_3D ( 'NONE', #14448, #45874, #75959 ) ;
#75283 = ORIENTED_EDGE ( 'NONE', *, *, #123069, .T. ) ;
#75284 = ORIENTED_EDGE ( 'NONE', *, *, #49073, .F. ) ;
#75285 = EDGE_CURVE ( 'NONE', #69514, #4494, #51953, .T. ) ;
#75286 = DIRECTION ( 'NONE',  ( 0.000000000000000000, 1.000000000000000000, 0.000000000000000000 ) ) ;
#75287 = EDGE_CURVE ( 'NONE', #88053, #60113, #110521, .T. ) ;
#75288 = EDGE_CURVE ( 'NONE', #51687, #33188, #125092, .T. ) ;
#75290 = ADVANCED_FACE ( 'NONE', ( #36006 ), #96837, .T. ) ;
#75289 = CIRCLE ( 'NONE', #21004, 0.1000000000000000472 ) ;
#75291 = CARTESIAN_POINT ( 'NONE',  ( 2.949999999999946887, 2.500000000000000000, -2.265063509461101798 ) ) ;
#75292 = FACE_OUTER_BOUND ( 'NONE', #123983, .T. ) ;
#75293 = EDGE_CURVE ( 'NONE', #17445, #32739, #85386, .T. ) ;
#75294 = ORIENTED_EDGE ( 'NONE', *, *, #40414, .T. ) ;
#75295 = CARTESIAN_POINT ( 'NONE',  ( 13.94999999999989271, 12.50000000000000000, -1.818653347947326138 ) ) ;
#75296 = DIRECTION ( 'NONE',  ( -0.000000000000000000, -1.000000000000000000, -0.000000000000000000 ) ) ;
#75297 = CARTESIAN_POINT ( 'NONE',  ( -7.900000000000011013, 12.50000000000000000, 4.330127018922196314 ) ) ;
#75298 = CARTESIAN_POINT ( 'NONE',  ( 10.64999999999991331, 2.500000000000000000, 6.248780366869521430 ) ) ;
#75299 = DIRECTION ( 'NONE',  ( 0.000000000000000000, 1.000000000000000000, 0.000000000000000000 ) ) ;
#75300 = ADVANCED_FACE ( 'NONE', ( #45827 ), #49897, .T. ) ;
#75301 = ORIENTED_EDGE ( 'NONE', *, *, #18225, .F. ) ;
#75302 = EDGE_CURVE ( 'NONE', #83089, #85131, #104264, .T. ) ;
#75303 = CARTESIAN_POINT ( 'NONE',  ( 13.14999999999989733, 12.50000000000000000, -2.511473670974877948 ) ) ;
#75304 = EDGE_LOOP ( 'NONE', ( #120223, #1264, #112826, #4994 ) ) ;
#75305 = ORIENTED_EDGE ( 'NONE', *, *, #122529, .T. ) ;
#75306 = ORIENTED_EDGE ( 'NONE', *, *, #28265, .T. ) ;
#75307 = CARTESIAN_POINT ( 'NONE',  ( -3.750000000000027978, 12.50000000000000000, 7.188010851410848723 ) ) ;
#75308 = FACE_BOUND ( 'NONE', #122071, .T. ) ;
#75309 = CARTESIAN_POINT ( 'NONE',  ( -3.350000000000031619, 2.500000000000000000, -5.902370205355750521 ) ) ;
#75310 = DIRECTION ( 'NONE',  ( 0.000000000000000000, -0.9999939076577903929, 0.003490651415223739937 ) ) ;
#75311 = CARTESIAN_POINT ( 'NONE',  ( 5.399999999999932854, 2.500000000000000000, 5.022947341949748790 ) ) ;
#75312 = AXIS2_PLACEMENT_3D ( 'NONE', #122738, #52706, #112917 ) ;
#75313 = ORIENTED_EDGE ( 'NONE', *, *, #124002, .F. ) ;
#75315 = VECTOR ( 'NONE', #56067, 1000.000000000000000 ) ;
#75314 = CARTESIAN_POINT ( 'NONE',  ( 14.99999999999989342, 2.500000000000000000, -0.6928203230275541413 ) ) ;
#75316 = CARTESIAN_POINT ( 'NONE',  ( 9.199999999999919353, 2.500000000000000000, -2.276824562219559311E-15 ) ) ;
#75317 = DIRECTION ( 'NONE',  ( 0.000000000000000000, 1.000000000000000000, 0.000000000000000000 ) ) ;
#75318 = FACE_OUTER_BOUND ( 'NONE', #28980, .T. ) ;
#75319 = EDGE_LOOP ( 'NONE', ( #41436, #106951, #44515, #71621 ) ) ;
#75320 = CARTESIAN_POINT ( 'NONE',  ( 1.649999999999948841, 12.50000000000000000, 6.560283801567334372 ) ) ;
#75322 = VECTOR ( 'NONE', #14620, 1000.000000000000000 ) ;
#75321 = CIRCLE ( 'NONE', #58617, 0.06509327318403745899 ) ;
#75323 = CARTESIAN_POINT ( 'NONE',  ( 4.399999999999939071, 2.500000000000000000, -0.3464101615137782364 ) ) ;
#75324 = ORIENTED_EDGE ( 'NONE', *, *, #100441, .T. ) ;
#75325 = FACE_OUTER_BOUND ( 'NONE', #121271, .T. ) ;
#75326 = EDGE_LOOP ( 'NONE', ( #89466, #1636, #123878, #68259 ) ) ;
#75327 = FACE_BOUND ( 'NONE', #64427, .T. ) ;
#75328 = DIRECTION ( 'NONE',  ( 0.000000000000000000, 1.000000000000000000, 0.000000000000000000 ) ) ;
#75329 = ORIENTED_EDGE ( 'NONE', *, *, #74826, .F. ) ;
#75330 = DIRECTION ( 'NONE',  ( 0.000000000000000000, 0.000000000000000000, 1.000000000000000000 ) ) ;
#75331 = DIRECTION ( 'NONE',  ( 0.000000000000000000, 0.000000000000000000, 1.000000000000000000 ) ) ;
#75332 = EDGE_LOOP ( 'NONE', ( #33130, #50782 ) ) ;
#75333 = ORIENTED_EDGE ( 'NONE', *, *, #60039, .T. ) ;
#75334 = CARTESIAN_POINT ( 'NONE',  ( 185.2968750003414300, 8.734944146203032389, 5.348610694689227483E-16 ) ) ;
#75335 = ORIENTED_EDGE ( 'NONE', *, *, #93458, .F. ) ;
#75336 = CARTESIAN_POINT ( 'NONE',  ( 185.7968750003414300, 8.734944146203032389, 5.348610694689227483E-16 ) ) ;
#75337 = DIRECTION ( 'NONE',  ( -0.000000000000000000, -1.000000000000000000, -0.000000000000000000 ) ) ;
#75338 = EDGE_CURVE ( 'NONE', #87541, #105417, #62422, .T. ) ;
#75339 = CARTESIAN_POINT ( 'NONE',  ( -13.29999999999999005, 2.500000000000000000, -4.330127018922198978 ) ) ;
#75340 = DIRECTION ( 'NONE',  ( -0.000000000000000000, -1.000000000000000000, -0.000000000000000000 ) ) ;
#75341 = CARTESIAN_POINT ( 'NONE',  ( -2.500000000000032419, 2.500000000000000000, 0.6928203230275494784 ) ) ;
#75342 = CARTESIAN_POINT ( 'NONE',  ( -10.84999999999999964, 12.50000000000000000, 1.537336459617582918 ) ) ;
#75343 = AXIS2_PLACEMENT_3D ( 'NONE', #9912, #1366, #121151 ) ;
#75344 = EDGE_LOOP ( 'NONE', ( #49261, #107030, #17784, #47853 ) ) ;
#75345 = ORIENTED_EDGE ( 'NONE', *, *, #56473, .T. ) ;
#75346 = DIRECTION ( 'NONE',  ( 0.000000000000000000, 0.000000000000000000, -1.000000000000000000 ) ) ;
#75347 = CARTESIAN_POINT ( 'NONE',  ( 8.149999999999923972, 2.500000000000000000, -6.248780366869526759 ) ) ;
#75348 = CARTESIAN_POINT ( 'NONE',  ( 10.39999999999991331, 2.500000000000000000, -2.385244779468109755E-15 ) ) ;
#75349 = LINE ( 'NONE', #106110, #23907 ) ;
#75351 = VERTEX_POINT ( 'NONE', #75269 ) ;
#75350 = ORIENTED_EDGE ( 'NONE', *, *, #35282, .T. ) ;
#75352 = FACE_BOUND ( 'NONE', #12903, .T. ) ;
#75353 = EDGE_LOOP ( 'NONE', ( #22054, #44707, #20060, #72717, #116026, #18415 ) ) ;
#75354 = CARTESIAN_POINT ( 'NONE',  ( -10.20000000000000462, 12.50000000000000000, -4.611443907251935315 ) ) ;
#75355 = CARTESIAN_POINT ( 'NONE',  ( 11.89999999999990798, 12.50000000000000000, -4.676537180435977881 ) ) ;
#75356 = AXIS2_PLACEMENT_3D ( 'NONE', #89478, #51501, #91407 ) ;
#75357 = ORIENTED_EDGE ( 'NONE', *, *, #85798, .T. ) ;
#75358 = DIRECTION ( 'NONE',  ( 0.000000000000000000, 1.000000000000000000, 0.000000000000000000 ) ) ;
#75359 = FACE_OUTER_BOUND ( 'NONE', #102422, .T. ) ;
#75360 = DIRECTION ( 'NONE',  ( 0.000000000000000000, 0.000000000000000000, 1.000000000000000000 ) ) ;
#75361 = DIRECTION ( 'NONE',  ( 0.000000000000000000, 1.000000000000000000, 0.000000000000000000 ) ) ;
#75362 = FACE_OUTER_BOUND ( 'NONE', #84988, .T. ) ;
#75363 = DIRECTION ( 'NONE',  ( 0.000000000000000000, 0.000000000000000000, 1.000000000000000000 ) ) ;
#75364 = CARTESIAN_POINT ( 'NONE',  ( 187.1093750003414016, 9.264065473108010111E-16, -7.564683531250000925 ) ) ;
#75365 = FACE_OUTER_BOUND ( 'NONE', #105822, .T. ) ;
#75366 = FACE_OUTER_BOUND ( 'NONE', #16211, .T. ) ;
#75367 = EDGE_LOOP ( 'NONE', ( #109045, #114028, #19689, #83813 ) ) ;
#75368 = AXIS2_PLACEMENT_3D ( 'NONE', #84335, #54237, #94152 ) ;
#75369 = ORIENTED_EDGE ( 'NONE', *, *, #53430, .F. ) ;
#75370 = DIRECTION ( 'NONE',  ( 0.000000000000000000, 0.000000000000000000, -1.000000000000000000 ) ) ;
#75371 = EDGE_LOOP ( 'NONE', ( #100784, #68853 ) ) ;
#75372 = LINE ( 'NONE', #35474, #1833 ) ;
#75374 = VERTEX_POINT ( 'NONE', #73990 ) ;
#75373 = EDGE_LOOP ( 'NONE', ( #18528, #113343 ) ) ;
#75375 = ORIENTED_EDGE ( 'NONE', *, *, #112539, .F. ) ;
#75376 = FACE_OUTER_BOUND ( 'NONE', #48898, .T. ) ;
#75377 = AXIS2_PLACEMENT_3D ( 'NONE', #14293, #63413, #51672 ) ;
#75378 = EDGE_CURVE ( 'NONE', #100973, #115124, #113923, .T. ) ;
#75379 = DIRECTION ( 'NONE',  ( 0.000000000000000000, 1.000000000000000000, 0.000000000000000000 ) ) ;
#75380 = CARTESIAN_POINT ( 'NONE',  ( -13.54999999999998828, 2.500000000000000000, 1.718653347947325383 ) ) ;
#75381 = AXIS2_PLACEMENT_3D ( 'NONE', #102069, #12387, #2549 ) ;
#75382 = FACE_OUTER_BOUND ( 'NONE', #103259, .T. ) ;
#75383 = DIRECTION ( 'NONE',  ( 0.000000000000000000, 1.000000000000000000, 0.000000000000000000 ) ) ;
#75384 = EDGE_CURVE ( 'NONE', #32532, #40814, #87519, .T. ) ;
#75385 = EDGE_LOOP ( 'NONE', ( #122069, #19637, #45922, #56020 ) ) ;
#75386 = ADVANCED_FACE ( 'NONE', ( #35363 ), #125019, .T. ) ;
#75387 = DIRECTION ( 'NONE',  ( -0.000000000000000000, 1.000000000000000000, -0.000000000000000000 ) ) ;
#75388 = ORIENTED_EDGE ( 'NONE', *, *, #101281, .T. ) ;
#75389 = ORIENTED_EDGE ( 'NONE', *, *, #114716, .T. ) ;
#75390 = ORIENTED_EDGE ( 'NONE', *, *, #105946, .F. ) ;
#75391 = ORIENTED_EDGE ( 'NONE', *, *, #107367, .T. ) ;
#75392 = ADVANCED_FACE ( 'NONE', ( #37931 ), #27447, .T. ) ;
#75394 = EDGE_CURVE ( 'NONE', #97846, #51736, #119704, .T. ) ;
#75393 = DIRECTION ( 'NONE',  ( -0.000000000000000000, 1.000000000000000000, -0.000000000000000000 ) ) ;
#75395 =( BOUNDED_CURVE ( )  B_SPLINE_CURVE ( 2, ( #62974, #102886, #70869, #40787, #52503, #32252, #122549 ),
 .UNSPECIFIED., .F., .F. ) 
 B_SPLINE_CURVE_WITH_KNOTS ( ( 3, 2, 2, 3 ),
 ( 0.7857142857142862535, 0.8095238095238102005, 0.8333333333333340365, 0.8571428571428578724 ),
 .UNSPECIFIED. ) 
 CURVE ( )  GEOMETRIC_REPRESENTATION_ITEM ( )  RATIONAL_B_SPLINE_CURVE ( ( 0.9999999999999968914, 0.8660254037844418162, 1.000000000000000000, 0.8660254037844387076, 1.000000000000000000, 0.8660254037844343777, 1.000000000000004441 ) ) 
 REPRESENTATION_ITEM ( '' )  );
#75397 = VERTEX_POINT ( 'NONE', #20228 ) ;
#75396 = ADVANCED_FACE ( 'NONE', ( #50331 ), #18918, .T. ) ;
#75398 = ORIENTED_EDGE ( 'NONE', *, *, #41866, .T. ) ;
#75399 = ADVANCED_FACE ( 'NONE', ( #58861 ), #91644, .T. ) ;
#75400 = CARTESIAN_POINT ( 'NONE',  ( 2.099999999999948574, 12.50000000000000000, 3.702399969078682407 ) ) ;
#75401 = CARTESIAN_POINT ( 'NONE',  ( 6.049999999999932321, 2.500000000000000000, 6.841600689897072485 ) ) ;
#75402 = DIRECTION ( 'NONE',  ( 0.000000000000000000, 0.000000000000000000, 1.000000000000000000 ) ) ;
#75403 = DIRECTION ( 'NONE',  ( 0.000000000000000000, 0.000000000000000000, 1.000000000000000000 ) ) ;
#75404 = DIRECTION ( 'NONE',  ( 0.000000000000000000, 0.000000000000000000, 1.000000000000000000 ) ) ;
#75405 = AXIS2_PLACEMENT_3D ( 'NONE', #60922, #11169, #41305 ) ;
#75406 = DIRECTION ( 'NONE',  ( 0.000000000000000000, 1.000000000000000000, 0.000000000000000000 ) ) ;
#75407 = EDGE_LOOP ( 'NONE', ( #103958, #78950, #92111, #70645 ) ) ;
#75408 = AXIS2_PLACEMENT_3D ( 'NONE', #5391, #66242, #86530 ) ;
#75409 = CIRCLE ( 'NONE', #8496, 0.09999999999999982514 ) ;
#75410 = EDGE_CURVE ( 'NONE', #108949, #7522, #18480, .T. ) ;
#75411 = CARTESIAN_POINT ( 'NONE',  ( -3.300000000000027800, 2.500000000000000000, -4.330127018922201643 ) ) ;
#75412 = ORIENTED_EDGE ( 'NONE', *, *, #59684, .T. ) ;
#75413 = CARTESIAN_POINT ( 'NONE',  ( -5.650000000000019895, 12.50000000000000000, 6.841600689897072485 ) ) ;
#75414 =( GEOMETRIC_REPRESENTATION_CONTEXT ( 3 ) GLOBAL_UNCERTAINTY_ASSIGNED_CONTEXT ( ( #75436 ) ) GLOBAL_UNIT_ASSIGNED_CONTEXT ( ( #66281, #46647, #66912 ) ) REPRESENTATION_CONTEXT ( 'NONE', 'WORKASPACE' ) );
#75415 = ORIENTED_EDGE ( 'NONE', *, *, #124740, .F. ) ;
#75416 = DIRECTION ( 'NONE',  ( 0.000000000000000000, 0.000000000000000000, -1.000000000000000000 ) ) ;
#75417 = ORIENTED_EDGE ( 'NONE', *, *, #42005, .F. ) ;
#75418 = CONICAL_SURFACE ( 'NONE', #6430, 0.09999999999999982514, 0.003490658503988666988 ) ;
#75419 = VERTEX_POINT ( 'NONE', #38598 ) ;
#75420 = LINE ( 'NONE', #55155, #84592 ) ;
#75421 = DIRECTION ( 'NONE',  ( -0.000000000000000000, -1.000000000000000000, -0.000000000000000000 ) ) ;
#75422 = CARTESIAN_POINT ( 'NONE',  ( -1.700000000000034817, 2.500000000000000000, -0.1000000000000023925 ) ) ;
#75423 = CARTESIAN_POINT ( 'NONE',  ( -8.350000000000012079, 2.500000000000000000, 1.372243186433545370 ) ) ;
#75424 = LINE ( 'NONE', #61931, #28238 ) ;
#75425 = EDGE_LOOP ( 'NONE', ( #20020, #33393, #125308, #35469 ) ) ;
#75426 = CARTESIAN_POINT ( 'NONE',  ( 0.1999999999999627909, 2.500000000000000000, 0.3464101615137758494 ) ) ;
#75427 = DIRECTION ( 'NONE',  ( 0.000000000000000000, 1.000000000000000000, 0.000000000000000000 ) ) ;
#75428 = ADVANCED_FACE ( 'NONE', ( #7813 ), #26898, .T. ) ;
#75429 = LINE ( 'NONE', #76090, #89913 ) ;
#75430 = DIRECTION ( 'NONE',  ( -0.000000000000000000, 1.000000000000000000, -0.000000000000000000 ) ) ;
#75431 = CARTESIAN_POINT ( 'NONE',  ( 10.64999999999991331, 12.50000000000000000, -1.883746621131363375 ) ) ;
#75432 = ORIENTED_EDGE ( 'NONE', *, *, #4771, .F. ) ;
#75433 = CIRCLE ( 'NONE', #209, 0.06509327318403745899 ) ;
#75434 = ORIENTED_EDGE ( 'NONE', *, *, #44102, .T. ) ;
#75435 = EDGE_CURVE ( 'NONE', #40951, #108184, #49059, .T. ) ;
#75436 = UNCERTAINTY_MEASURE_WITH_UNIT (LENGTH_MEASURE( 1.000000000000000082E-05 ), #66281, 'distance_accuracy_value', 'NONE');
#75437 = EDGE_CURVE ( 'NONE', #13624, #114894, #22710, .T. ) ;
#75438 = ORIENTED_EDGE ( 'NONE', *, *, #121826, .F. ) ;
#75439 = FACE_OUTER_BOUND ( 'NONE', #121247, .T. ) ;
#75440 = AXIS2_PLACEMENT_3D ( 'NONE', #129564, #39882, #81087 ) ;
#75441 = DIRECTION ( 'NONE',  ( 0.000000000000000000, 0.000000000000000000, -1.000000000000000000 ) ) ;
#75442 = AXIS2_PLACEMENT_3D ( 'NONE', #79601, #110345, #118233 ) ;
#75443 = EDGE_CURVE ( 'NONE', #96072, #65503, #78526, .T. ) ;
#75444 = CARTESIAN_POINT ( 'NONE',  ( 185.5468750003414300, -8.734944146203032389, -1.604583208406768146E-15 ) ) ;
#75445 = CARTESIAN_POINT ( 'NONE',  ( -11.44999999999999751, 2.500000000000000000, -2.511473670974873951 ) ) ;
#75446 = CARTESIAN_POINT ( 'NONE',  ( -1.650000000000034328, 2.500000000000000000, -7.188010851410854052 ) ) ;
#75447 = ADVANCED_FACE ( 'NONE', ( #128919 ), #12314, .T. ) ;
#75448 = CARTESIAN_POINT ( 'NONE',  ( -3.550000000000031797, 2.500000000000000000, -6.148780366869526226 ) ) ;
#75449 = FACE_OUTER_BOUND ( 'NONE', #15533, .T. ) ;
#75450 = EDGE_LOOP ( 'NONE', ( #86298, #72294 ) ) ;
#75451 = CIRCLE ( 'NONE', #50412, 0.1000000000000000472 ) ;
#75452 = EDGE_CURVE ( 'NONE', #114600, #98683, #116856, .T. ) ;
#75453 = CIRCLE ( 'NONE', #81712, 0.1000000000000002554 ) ;
#75454 = EDGE_CURVE ( 'NONE', #70834, #54150, #50000, .T. ) ;
#75455 = ADVANCED_FACE ( 'NONE', ( #117111 ), #85474, .T. ) ;
#75456 = CARTESIAN_POINT ( 'NONE',  ( -10.45000000000000462, 2.500000000000000000, -2.265063509461097802 ) ) ;
#75457 = LINE ( 'NONE', #63720, #76913 ) ;
#75458 = ORIENTED_EDGE ( 'NONE', *, *, #99808, .T. ) ;
#75459 = CARTESIAN_POINT ( 'NONE',  ( 11.44999999999990692, 2.500000000000000000, -6.941600689897078347 ) ) ;
#75460 = DIRECTION ( 'NONE',  ( 0.000000000000000000, 0.000000000000000000, 1.000000000000000000 ) ) ;
#75461 = EDGE_CURVE ( 'NONE', #60587, #85684, #99446, .T. ) ;
#75462 = CARTESIAN_POINT ( 'NONE',  ( -8.750000000000010658, 2.500000000000000000, -1.572243186433550211 ) ) ;
#75463 = CIRCLE ( 'NONE', #50342, 0.1000000000000002554 ) ;
#75464 = AXIS2_PLACEMENT_3D ( 'NONE', #60691, #51509, #92056 ) ;
#75465 = ORIENTED_EDGE ( 'NONE', *, *, #96847, .F. ) ;
#75466 = PRODUCT_DEFINITION_SHAPE ( 'NONE', 'NONE',  #98771 ) ;
#75467 = PLANE ( 'NONE',  #88667 ) ;
#75468 = ORIENTED_EDGE ( 'NONE', *, *, #17938, .T. ) ;
#75469 = CARTESIAN_POINT ( 'NONE',  ( 6.049999999999932321, 2.500000000000000000, 6.741600689897071952 ) ) ;
#75470 = DIRECTION ( 'NONE',  ( 0.000000000000000000, 0.000000000000000000, 1.000000000000000000 ) ) ;
#75471 = AXIS2_PLACEMENT_3D ( 'NONE', #36390, #16701, #96558 ) ;
#75472 = ORIENTED_EDGE ( 'NONE', *, *, #79610, .T. ) ;
#75473 = DIRECTION ( 'NONE',  ( -0.000000000000000000, 1.000000000000000000, -0.000000000000000000 ) ) ;
#75474 = CARTESIAN_POINT ( 'NONE',  ( 12.04999999999990479, 12.50000000000000000, -6.430097255199264339 ) ) ;
#75475 = AXIS2_PLACEMENT_3D ( 'NONE', #98505, #67772, #90637 ) ;
#75476 = VECTOR ( 'NONE', #76387, 1000.000000000000000 ) ;
#75477 = ORIENTED_EDGE ( 'NONE', *, *, #20914, .T. ) ;
#75478 = DIRECTION ( 'NONE',  ( 0.000000000000000000, 0.000000000000000000, 1.000000000000000000 ) ) ;
#75479 = ORIENTED_EDGE ( 'NONE', *, *, #85992, .F. ) ;
#75480 = ORIENTED_EDGE ( 'NONE', *, *, #59895, .F. ) ;
#75481 = DIRECTION ( 'NONE',  ( -0.000000000000000000, -1.000000000000000000, -0.000000000000000000 ) ) ;
#75482 = DIRECTION ( 'NONE',  ( 0.000000000000000000, 0.000000000000000000, -1.000000000000000000 ) ) ;
#75483 = VERTEX_POINT ( 'NONE', #28768 ) ;
#75484 = DIRECTION ( 'NONE',  ( 0.000000000000000000, 1.000000000000000000, 0.000000000000000000 ) ) ;
#75485 = DIRECTION ( 'NONE',  ( -4.274815082592931898E-19, -0.9999939076577903929, -0.003490651415223739937 ) ) ;
#75486 = ORIENTED_EDGE ( 'NONE', *, *, #64171, .T. ) ;
#75487 = PLANE ( 'NONE',  #126149 ) ;
#75488 = DIRECTION ( 'NONE',  ( 1.000000000000000000, 0.000000000000000000, 0.000000000000000000 ) ) ;
#75489 = EDGE_CURVE ( 'NONE', #125527, #2669, #118925, .T. ) ;
#75490 = AXIS2_PLACEMENT_3D ( 'NONE', #26162, #7140, #7796 ) ;
#75491 = DIRECTION ( 'NONE',  ( 0.000000000000000000, 0.000000000000000000, 1.000000000000000000 ) ) ;
#75492 = CARTESIAN_POINT ( 'NONE',  ( 13.09999999999990195, 12.50000000000000000, -3.983716857408426293 ) ) ;
#75493 = AXIS2_PLACEMENT_3D ( 'NONE', #19058, #116631, #49213 ) ;
#75494 = CARTESIAN_POINT ( 'NONE',  ( -15.19999999999998330, 2.500000000000000000, 0.4464101615137758272 ) ) ;
#75495 = CARTESIAN_POINT ( 'NONE',  ( 0.1999999999999636513, 2.500000000000000000, -0.2464101615137760659 ) ) ;
#75496 = CIRCLE ( 'NONE', #10731, 0.06509327318403745899 ) ;
#75497 = ORIENTED_EDGE ( 'NONE', *, *, #109585, .F. ) ;
#75499 = VERTEX_POINT ( 'NONE', #89610 ) ;
#75498 = CIRCLE ( 'NONE', #60935, 0.06509327318403745899 ) ;
#75500 = VERTEX_POINT ( 'NONE', #28114 ) ;
#75501 = EDGE_LOOP ( 'NONE', ( #1202, #33162 ) ) ;
#75502 = FACE_OUTER_BOUND ( 'NONE', #93104, .T. ) ;
#75503 = CARTESIAN_POINT ( 'NONE',  ( 8.549999999999924327, 2.500000000000000000, 1.818653347947321475 ) ) ;
#75504 = AXIS2_PLACEMENT_3D ( 'NONE', #76858, #116764, #57866 ) ;
#75505 = CARTESIAN_POINT ( 'NONE',  ( 11.24999999999990941, 2.500000000000000000, 7.188010851410848723 ) ) ;
#75506 = ORIENTED_EDGE ( 'NONE', *, *, #113831, .T. ) ;
#75507 = EDGE_CURVE ( 'NONE', #7967, #99945, #68029, .T. ) ;
#75508 = FACE_BOUND ( 'NONE', #81506, .T. ) ;
#75509 = FACE_OUTER_BOUND ( 'NONE', #19556, .T. ) ;
#75510 = DIRECTION ( 'NONE',  ( 0.000000000000000000, 0.000000000000000000, 1.000000000000000000 ) ) ;
#75511 = FACE_OUTER_BOUND ( 'NONE', #49750, .T. ) ;
#75512 = FACE_OUTER_BOUND ( 'NONE', #62283, .T. ) ;
#75513 = PLANE ( 'NONE',  #95288 ) ;
#75514 = DIRECTION ( 'NONE',  ( 0.000000000000000000, -0.9999939076577903929, 0.003490651415223739937 ) ) ;
#75515 = DIRECTION ( 'NONE',  ( 0.000000000000000000, 0.000000000000000000, 1.000000000000000000 ) ) ;
#75516 = DIRECTION ( 'NONE',  ( 0.000000000000000000, 1.000000000000000000, 0.000000000000000000 ) ) ;
#75517 = DIRECTION ( 'NONE',  ( 0.000000000000000000, 0.000000000000000000, 1.000000000000000000 ) ) ;
#75518 = CARTESIAN_POINT ( 'NONE',  ( -5.400000000000019895, 2.500000000000000000, 4.330127018922196314 ) ) ;
#75519 = ORIENTED_EDGE ( 'NONE', *, *, #13009, .T. ) ;
#75520 = ORIENTED_EDGE ( 'NONE', *, *, #86630, .F. ) ;
#75521 = VERTEX_POINT ( 'NONE', #18281 ) ;
#75522 = ORIENTED_EDGE ( 'NONE', *, *, #124031, .T. ) ;
#75523 = DIRECTION ( 'NONE',  ( 0.000000000000000000, 0.000000000000000000, 1.000000000000000000 ) ) ;
#75524 = EDGE_LOOP ( 'NONE', ( #91811, #67079 ) ) ;
#75525 = DIRECTION ( 'NONE',  ( 0.000000000000000000, 1.000000000000000000, 0.000000000000000000 ) ) ;
#75526 = VERTEX_POINT ( 'NONE', #40534 ) ;
#75527 = ORIENTED_EDGE ( 'NONE', *, *, #55192, .T. ) ;
#75528 = CARTESIAN_POINT ( 'NONE',  ( -3.100000000000028511, 12.50000000000000000, -3.983716857408426293 ) ) ;
#75529 = CONICAL_SURFACE ( 'NONE', #40046, 0.1000000000000002554, 0.003490658503988666988 ) ;
#75530 = AXIS2_PLACEMENT_3D ( 'NONE', #59176, #70919, #110826 ) ;
#75531 = EDGE_CURVE ( 'NONE', #47341, #100839, #52041, .T. ) ;
#75532 = CARTESIAN_POINT ( 'NONE',  ( 8.340322510127135658, -2.499999999999999556, 8.517653997967773449 ) ) ;
#75533 = LINE ( 'NONE', #65723, #93833 ) ;
#75534 = CARTESIAN_POINT ( 'NONE',  ( 13.94999999999989626, 2.500000000000000000, 2.611473670974873151 ) ) ;
#75535 = CARTESIAN_POINT ( 'NONE',  ( 6.649999999999927525, 2.500000000000000000, 2.165063509461097713 ) ) ;
#75536 = EDGE_LOOP ( 'NONE', ( #50327, #27128, #84036, #92239 ) ) ;
#75537 = CONICAL_SURFACE ( 'NONE', #100669, 0.09999999999999999167, 0.003490658503988666988 ) ;
#75538 = ADVANCED_FACE ( 'NONE', ( #81710 ), #113108, .T. ) ;
#75539 = AXIS2_PLACEMENT_3D ( 'NONE', #34052, #111974, #25495 ) ;
#75540 = ORIENTED_EDGE ( 'NONE', *, *, #78274, .T. ) ;
#75541 = EDGE_LOOP ( 'NONE', ( #95900, #88406 ) ) ;
#75542 = ORIENTED_EDGE ( 'NONE', *, *, #76780, .T. ) ;
#75543 = ADVANCED_FACE ( 'NONE', ( #31994 ), #81387, .T. ) ;
#75545 = EDGE_CURVE ( 'NONE', #11304, #4486, #106400, .T. ) ;
#75544 = CARTESIAN_POINT ( 'NONE',  ( 184.6666666666666856, -6.668395609140176816, -3.850000000000003642 ) ) ;
#75547 = ORIENTED_EDGE ( 'NONE', *, *, #14288, .T. ) ;
#75546 = ADVANCED_FACE ( 'NONE', ( #111156 ), #110606, .T. ) ;
#75548 = EDGE_CURVE ( 'NONE', #118876, #91012, #22182, .T. ) ;
#75549 = ORIENTED_EDGE ( 'NONE', *, *, #40718, .F. ) ;
#75550 = CIRCLE ( 'NONE', #102737, 0.09999999999999999167 ) ;
#75551 = CARTESIAN_POINT ( 'NONE',  ( -11.44999999999999751, 2.500000000000000000, 6.841600689897072485 ) ) ;
#75552 = AXIS2_PLACEMENT_3D ( 'NONE', #64127, #104058, #54311 ) ;
#75553 = AXIS2_PLACEMENT_3D ( 'NONE', #21900, #1584, #109627 ) ;
#75554 = CARTESIAN_POINT ( 'NONE',  ( -12.09999999999999609, 12.50000000000000000, -5.022947341949751454 ) ) ;
#75555 = CARTESIAN_POINT ( 'NONE',  ( -12.49999999999995914, 2.500000000000000000, 0.1000000000000018513 ) ) ;
#75556 = LINE ( 'NONE', #23905, #108854 ) ;
#75557 = AXIS2_PLACEMENT_3D ( 'NONE', #26522, #54049, #25874 ) ;
#75558 = PLANE ( 'NONE',  #56608 ) ;
#75559 = CARTESIAN_POINT ( 'NONE',  ( 13.94999999999989626, 12.50000000000000000, 2.511473670974873507 ) ) ;
#75560 = EDGE_CURVE ( 'NONE', #40528, #30572, #3987, .T. ) ;
#75561 = VECTOR ( 'NONE', #47484, 1000.000000000000000 ) ;
#75562 = VERTEX_POINT ( 'NONE', #122306 ) ;
#75563 = CARTESIAN_POINT ( 'NONE',  ( -8.550000000000013145, 12.50000000000000000, -1.883746621131363597 ) ) ;
#75564 = EDGE_CURVE ( 'NONE', #27825, #5027, #54188, .T. ) ;
#75565 = ADVANCED_FACE ( 'NONE', ( #12958, #92845 ), #1861, .F. ) ;
#75566 = VERTEX_POINT ( 'NONE', #80443 ) ;
#75567 = FACE_OUTER_BOUND ( 'NONE', #25439, .T. ) ;
#75568 = ORIENTED_EDGE ( 'NONE', *, *, #17766, .F. ) ;
#75569 = CARTESIAN_POINT ( 'NONE',  ( -1.650000000000034772, 2.500000000000000000, 5.902370205355745192 ) ) ;
#75570 = CIRCLE ( 'NONE', #44180, 10.00000000000000000 ) ;
#75571 = LINE ( 'NONE', #46777, #13524 ) ;
#75572 = EDGE_LOOP ( 'NONE', ( #32704, #108621, #62683, #21668 ) ) ;
#75573 = CARTESIAN_POINT ( 'NONE',  ( -2.900000000000029665, 2.500000000000000000, 4.230127018922196669 ) ) ;
#75574 = CARTESIAN_POINT ( 'NONE',  ( 139.9358549477330200, 2.500000000000000000, -1.098523788719517169 ) ) ;
#75575 = ORIENTED_EDGE ( 'NONE', *, *, #105553, .T. ) ;
#75576 = DIRECTION ( 'NONE',  ( 0.000000000000000000, 1.000000000000000000, 0.000000000000000000 ) ) ;
#75577 = PLANE ( 'NONE',  #19426 ) ;
#75578 = EDGE_LOOP ( 'NONE', ( #32676, #30218, #80370, #34544 ) ) ;
#75579 = ORIENTED_EDGE ( 'NONE', *, *, #15566, .F. ) ;
#75580 = CARTESIAN_POINT ( 'NONE',  ( -0.4000000000000331624, 12.50000000000000000, -0.6277270498435144619 ) ) ;
#75581 = FACE_OUTER_BOUND ( 'NONE', #4843, .T. ) ;
#75582 = CARTESIAN_POINT ( 'NONE',  ( 184.1927083336747160, 6.551208109652275624, -3.782341765624998686 ) ) ;
#75583 = DIRECTION ( 'NONE',  ( 0.000000000000000000, 1.000000000000000000, 0.000000000000000000 ) ) ;
#75584 = CARTESIAN_POINT ( 'NONE',  ( 9.399999999999915090, 12.50000000000000000, -4.741630453620015118 ) ) ;
#75585 = DIRECTION ( 'NONE',  ( 0.000000000000000000, 1.000000000000000000, 0.000000000000000000 ) ) ;
#75586 = CIRCLE ( 'NONE', #125749, 0.09999999999999982514 ) ;
#75587 = AXIS2_PLACEMENT_3D ( 'NONE', #6631, #106171, #8582 ) ;
#75588 = EDGE_LOOP ( 'NONE', ( #65837, #63221, #93914, #42662 ) ) ;
#75589 = DIRECTION ( 'NONE',  ( -0.000000000000000000, 1.000000000000000000, -0.000000000000000000 ) ) ;
#75590 = VECTOR ( 'NONE', #101802, 1000.000000000000000 ) ;
#75591 = EDGE_LOOP ( 'NONE', ( #17733, #93130, #27631, #12288 ) ) ;
#75592 = CIRCLE ( 'NONE', #117430, 0.1000000000000002554 ) ;
#75593 = DIRECTION ( 'NONE',  ( 0.000000000000000000, 1.000000000000000000, 0.000000000000000000 ) ) ;
#75594 = DIRECTION ( 'NONE',  ( 0.000000000000000000, 0.000000000000000000, 1.000000000000000000 ) ) ;
#75595 = EDGE_CURVE ( 'NONE', #102282, #56299, #29064, .T. ) ;
#75596 = FACE_OUTER_BOUND ( 'NONE', #100361, .T. ) ;
#75597 = ORIENTED_EDGE ( 'NONE', *, *, #33937, .T. ) ;
#75598 = CIRCLE ( 'NONE', #117438, 0.06509327318403745899 ) ;
#75599 = EDGE_CURVE ( 'NONE', #126826, #71554, #93897, .T. ) ;
#75600 = ADVANCED_FACE ( 'NONE', ( #53557 ), #45781, .T. ) ;
#75601 = CARTESIAN_POINT ( 'NONE',  ( -14.79999999999998295, 2.500000000000000000, -0.4464101615137760493 ) ) ;
#75602 = LINE ( 'NONE', #4922, #114471 ) ;
#75603 = ORIENTED_EDGE ( 'NONE', *, *, #103490, .T. ) ;
#75604 = ADVANCED_FACE ( 'NONE', ( #1225 ), #41681, .T. ) ;
#75605 = DIRECTION ( 'NONE',  ( -0.000000000000000000, -1.000000000000000000, -0.000000000000000000 ) ) ;
#75606 = ORIENTED_EDGE ( 'NONE', *, *, #3585, .F. ) ;
#75607 = EDGE_LOOP ( 'NONE', ( #38177, #89822 ) ) ;
#75608 = DIRECTION ( 'NONE',  ( 0.000000000000000000, 0.000000000000000000, -1.000000000000000000 ) ) ;
#75609 = ORIENTED_EDGE ( 'NONE', *, *, #87692, .F. ) ;
#75610 = CARTESIAN_POINT ( 'NONE',  ( -0.6500000000000389910, 12.50000000000000000, -6.213873640053564351 ) ) ;
#75611 = CARTESIAN_POINT ( 'NONE',  ( -4.800000000000022915, 2.500000000000000000, -0.3464101615137783474 ) ) ;
#75612 = FACE_OUTER_BOUND ( 'NONE', #95517, .T. ) ;
#75613 = VECTOR ( 'NONE', #112958, 1000.000000000000000 ) ;
#75614 = ORIENTED_EDGE ( 'NONE', *, *, #22360, .T. ) ;
#75615 = VECTOR ( 'NONE', #41481, 1000.000000000000000 ) ;
#75616 = FACE_BOUND ( 'NONE', #93380, .T. ) ;
#75618 = VERTEX_POINT ( 'NONE', #71248 ) ;
#75617 = DIRECTION ( 'NONE',  ( -4.274815082592931898E-19, -0.9999939076577903929, -0.003490651415223739937 ) ) ;
#75619 = PLANE ( 'NONE',  #33977 ) ;
#75620 = CARTESIAN_POINT ( 'NONE',  ( -10.20000000000000462, 2.500000000000000000, -4.776537180435973085 ) ) ;
#75621 = EDGE_CURVE ( 'NONE', #61759, #20290, #6043, .T. ) ;
#75622 = AXIS2_PLACEMENT_3D ( 'NONE', #118296, #129439, #58739 ) ;
#75623 = ORIENTED_EDGE ( 'NONE', *, *, #125123, .T. ) ;
#75624 = VECTOR ( 'NONE', #86535, 1000.000000000000000 ) ;
#75625 = AXIS2_PLACEMENT_3D ( 'NONE', #64493, #4261, #44200 ) ;
#75626 = EDGE_LOOP ( 'NONE', ( #121266, #22955 ) ) ;
#75627 = AXIS2_PLACEMENT_3D ( 'NONE', #92435, #2765, #32897 ) ;
#75628 = ORIENTED_EDGE ( 'NONE', *, *, #66593, .F. ) ;
#75629 = CARTESIAN_POINT ( 'NONE',  ( -11.44999999999999751, 12.50000000000000000, 6.841600689897072485 ) ) ;
#75630 = FACE_OUTER_BOUND ( 'NONE', #77542, .T. ) ;
#75631 = LINE ( 'NONE', #54080, #39992 ) ;
#75632 = FACE_BOUND ( 'NONE', #22719, .T. ) ;
#75633 = ORIENTED_EDGE ( 'NONE', *, *, #9069, .F. ) ;
#75634 = CARTESIAN_POINT ( 'NONE',  ( 184.9427083336747160, -6.551208109652278289, 3.782341765624995134 ) ) ;
#75635 = DIRECTION ( 'NONE',  ( 0.000000000000000000, -0.000000000000000000, 1.000000000000000000 ) ) ;
#75636 = DIRECTION ( 'NONE',  ( -0.000000000000000000, -1.000000000000000000, -0.000000000000000000 ) ) ;
#75637 = AXIS2_PLACEMENT_3D ( 'NONE', #83531, #73686, #113625 ) ;
#75638 = CIRCLE ( 'NONE', #106944, 0.06509327318403745899 ) ;
#75639 = LINE ( 'NONE', #35109, #105648 ) ;
#75640 = ADVANCED_FACE ( 'NONE', ( #63376 ), #570, .T. ) ;
#75641 = VECTOR ( 'NONE', #126542, 1000.000000000000000 ) ;
#75642 = CIRCLE ( 'NONE', #19208, 0.1000000000000002554 ) ;
#75643 = AXIS2_PLACEMENT_3D ( 'NONE', #25280, #14175, #25954 ) ;
#75644 = DIRECTION ( 'NONE',  ( -0.000000000000000000, -1.000000000000000000, -0.000000000000000000 ) ) ;
#75645 = DIRECTION ( 'NONE',  ( -4.274815082592931898E-19, -0.9999939076577903929, -0.003490651415223739937 ) ) ;
#75646 = DIRECTION ( 'NONE',  ( 0.000000000000000000, 1.000000000000000000, 0.000000000000000000 ) ) ;
#75647 = CONICAL_SURFACE ( 'NONE', #107042, 0.09999999999999982514, 0.003490658503988666988 ) ;
#75648 = FACE_OUTER_BOUND ( 'NONE', #84639, .T. ) ;
#75649 = DIRECTION ( 'NONE',  ( 0.000000000000000000, 0.000000000000000000, 1.000000000000000000 ) ) ;
#75650 = ORIENTED_EDGE ( 'NONE', *, *, #28461, .F. ) ;
#75651 = AXIS2_PLACEMENT_3D ( 'NONE', #50546, #90465, #32875 ) ;
#75652 = ORIENTED_EDGE ( 'NONE', *, *, #125934, .T. ) ;
#75653 = ORIENTED_EDGE ( 'NONE', *, *, #63015, .F. ) ;
#75654 = ORIENTED_EDGE ( 'NONE', *, *, #117792, .T. ) ;
#75655 = ORIENTED_EDGE ( 'NONE', *, *, #4619, .F. ) ;
#75656 = CARTESIAN_POINT ( 'NONE',  ( 14.14999999999989377, 2.500000000000000000, -2.857883832488653741 ) ) ;
#75657 = DIRECTION ( 'NONE',  ( 0.000000000000000000, -0.000000000000000000, 1.000000000000000000 ) ) ;
#75658 = ORIENTED_EDGE ( 'NONE', *, *, #95206, .T. ) ;
#75659 = EDGE_CURVE ( 'NONE', #102047, #1314, #121078, .T. ) ;
#75660 = FACE_BOUND ( 'NONE', #124575, .T. ) ;
#75661 = DIRECTION ( 'NONE',  ( -0.000000000000000000, -1.000000000000000000, -0.000000000000000000 ) ) ;
#75662 = CARTESIAN_POINT ( 'NONE',  ( 127.5000000000000000, 5.000000000000000000, 5.000000000000001776 ) ) ;
#75663 = DIRECTION ( 'NONE',  ( 1.000000000000000000, 0.000000000000000000, 0.000000000000000000 ) ) ;
#75664 = EDGE_CURVE ( 'NONE', #127955, #65687, #43742, .T. ) ;
#75665 = FACE_OUTER_BOUND ( 'NONE', #30163, .T. ) ;
#75666 = DIRECTION ( 'NONE',  ( 0.000000000000000000, 0.000000000000000000, 1.000000000000000000 ) ) ;
#75667 = ORIENTED_EDGE ( 'NONE', *, *, #71100, .T. ) ;
#75668 = CARTESIAN_POINT ( 'NONE',  ( 127.5000000000000000, -5.000000000000000000, 2.000000000000001776 ) ) ;
#75669 = VERTEX_POINT ( 'NONE', #87981 ) ;
#75670 = ORIENTED_EDGE ( 'NONE', *, *, #97021, .T. ) ;
#75671 = AXIS2_PLACEMENT_3D ( 'NONE', #113652, #63910, #78256 ) ;
#75672 = EDGE_LOOP ( 'NONE', ( #75048, #19825, #68077, #89677 ) ) ;
#75673 = AXIS2_PLACEMENT_3D ( 'NONE', #19683, #20965, #99541 ) ;
#75674 = CARTESIAN_POINT ( 'NONE',  ( 13.94999999999989271, 12.50000000000000000, -1.818653347947326138 ) ) ;
#75675 = CARTESIAN_POINT ( 'NONE',  ( -12.69999999999999041, 2.500000000000000000, 3.883716857408421319 ) ) ;
#75676 = DIRECTION ( 'NONE',  ( 0.000000000000000000, 1.000000000000000000, 0.000000000000000000 ) ) ;
#75677 = ORIENTED_EDGE ( 'NONE', *, *, #99580, .T. ) ;
#75678 = CARTESIAN_POINT ( 'NONE',  ( 3.710216157338618537, 1.500000000000638156, -9.999999999999998224 ) ) ;
#75679 = DIRECTION ( 'NONE',  ( -4.274815082592931898E-19, -0.9999939076577903929, -0.003490651415223739937 ) ) ;
#75680 = CIRCLE ( 'NONE', #100724, 0.09999999999999982514 ) ;
#75681 = CIRCLE ( 'NONE', #119600, 0.06509327318403745899 ) ;
#75683 = EDGE_CURVE ( 'NONE', #124666, #102847, #114395, .T. ) ;
#75682 = CIRCLE ( 'NONE', #121754, 0.1000000000000002554 ) ;
#75684 = DIRECTION ( 'NONE',  ( 0.000000000000000000, 0.000000000000000000, -1.000000000000000000 ) ) ;
#75685 = CARTESIAN_POINT ( 'NONE',  ( 185.1145833340161175, 6.668395609140177704, -3.849999999999998312 ) ) ;
#75686 = DIRECTION ( 'NONE',  ( 0.000000000000000000, 0.000000000000000000, 1.000000000000000000 ) ) ;
#75687 = CONICAL_SURFACE ( 'NONE', #19247, 0.1000000000000000056, 0.003490658503988666988 ) ;
#75688 = CIRCLE ( 'NONE', #19248, 0.06509327318403745899 ) ;
#75689 = CARTESIAN_POINT ( 'NONE',  ( 3.099999999999944134, 2.500000000000000000, 4.576537180435972019 ) ) ;
#75690 = ORIENTED_EDGE ( 'NONE', *, *, #122553, .T. ) ;
#75691 = DIRECTION ( 'NONE',  ( 0.000000000000000000, 1.000000000000000000, 0.000000000000000000 ) ) ;
#75692 = CONICAL_SURFACE ( 'NONE', #19255, 0.09999999999999999167, 0.003490658503988666988 ) ;
#75693 = EDGE_CURVE ( 'NONE', #60634, #95189, #112672, .T. ) ;
#75694 = VERTEX_POINT ( 'NONE', #35218 ) ;
#75695 = EDGE_LOOP ( 'NONE', ( #10841, #114587 ) ) ;
#75696 = DIRECTION ( 'NONE',  ( 0.000000000000000000, 0.000000000000000000, -1.000000000000000000 ) ) ;
#75697 = EDGE_CURVE ( 'NONE', #129522, #1501, #83663, .T. ) ;
#75698 = LINE ( 'NONE', #63964, #17424 ) ;
#75700 = EDGE_CURVE ( 'NONE', #110514, #21869, #70912, .T. ) ;
#75699 = DIRECTION ( 'NONE',  ( 0.000000000000000000, -0.000000000000000000, 1.000000000000000000 ) ) ;
#75701 = EDGE_CURVE ( 'NONE', #35149, #11533, #67708, .T. ) ;
#75702 = EDGE_CURVE ( 'NONE', #105674, #14788, #4415, .T. ) ;
#75703 = ORIENTED_EDGE ( 'NONE', *, *, #78097, .T. ) ;
#75704 = EDGE_LOOP ( 'NONE', ( #53189, #54373 ) ) ;
#75705 = CARTESIAN_POINT ( 'NONE',  ( 3.749999999999942268, 12.50000000000000000, 1.472243186433545459 ) ) ;
#75706 = CARTESIAN_POINT ( 'NONE',  ( 3.149999999999944400, 2.500000000000000000, 2.611473670974873151 ) ) ;
#75707 = EDGE_CURVE ( 'NONE', #84904, #6379, #35317, .T. ) ;
#75708 = DIRECTION ( 'NONE',  ( 0.000000000000000000, 0.000000000000000000, 1.000000000000000000 ) ) ;
#75709 = VERTEX_POINT ( 'NONE', #33912 ) ;
#75710 = EDGE_LOOP ( 'NONE', ( #101896, #76138 ) ) ;
#75711 = ADVANCED_FACE ( 'NONE', ( #24737 ), #57914, .T. ) ;
#75712 = DIRECTION ( 'NONE',  ( 0.000000000000000000, 0.000000000000000000, -1.000000000000000000 ) ) ;
#75713 = ADVANCED_FACE ( 'NONE', ( #84939 ), #73833, .T. ) ;
#75715 = ORIENTED_EDGE ( 'NONE', *, *, #13020, .T. ) ;
#75714 = AXIS2_PLACEMENT_3D ( 'NONE', #76419, #56113, #116318 ) ;
#75716 = DIRECTION ( 'NONE',  ( 0.000000000000000000, 1.000000000000000000, 0.000000000000000000 ) ) ;
#75717 = ADVANCED_FACE ( 'NONE', ( #37630 ), #108451, .T. ) ;
#75718 = ADVANCED_FACE ( 'NONE', ( #17295 ), #57261, .T. ) ;
#75719 = FACE_OUTER_BOUND ( 'NONE', #74105, .T. ) ;
#75720 = ORIENTED_EDGE ( 'NONE', *, *, #2644, .T. ) ;
#75721 = DIRECTION ( 'NONE',  ( 0.000000000000000000, -0.000000000000000000, 1.000000000000000000 ) ) ;
#75722 = FACE_OUTER_BOUND ( 'NONE', #105290, .T. ) ;
#75723 = DIRECTION ( 'NONE',  ( 0.000000000000000000, 1.000000000000000000, 0.000000000000000000 ) ) ;
#75726 = EDGE_CURVE ( 'NONE', #18013, #109495, #113769, .T. ) ;
#75725 = AXIS2_PLACEMENT_3D ( 'NONE', #43621, #25232, #106383 ) ;
#75724 = DIRECTION ( 'NONE',  ( 0.000000000000000000, 0.000000000000000000, -1.000000000000000000 ) ) ;
#75727 = ORIENTED_EDGE ( 'NONE', *, *, #110973, .F. ) ;
#75728 = CARTESIAN_POINT ( 'NONE',  ( 3.749999999999942268, 2.500000000000000000, -1.472243186433550122 ) ) ;
#75729 = AXIS2_PLACEMENT_3D ( 'NONE', #79486, #90574, #119383 ) ;
#75730 = CARTESIAN_POINT ( 'NONE',  ( 6.849999999999927702, 2.500000000000000000, 1.718653347947321386 ) ) ;
#75731 = VERTEX_POINT ( 'NONE', #103943 ) ;
#75732 = ORIENTED_EDGE ( 'NONE', *, *, #87527, .T. ) ;
#75733 = CARTESIAN_POINT ( 'NONE',  ( 184.3385416670080872, 6.551208109652274736, 3.782341765625001351 ) ) ;
#75734 = CARTESIAN_POINT ( 'NONE',  ( 12.69999999999990337, 12.50000000000000000, -4.611443907251940644 ) ) ;
#75735 = LINE ( 'NONE', #115658, #30134 ) ;
#75736 = CARTESIAN_POINT ( 'NONE',  ( -6.050000000000017586, 2.500000000000000000, 6.148780366869520009 ) ) ;
#75737 = VECTOR ( 'NONE', #83835, 1000.000000000000000 ) ;
#75738 = LINE ( 'NONE', #85566, #115843 ) ;
#75739 = DIRECTION ( 'NONE',  ( 0.000000000000000000, -0.9999939076577903929, 0.003490651415223739937 ) ) ;
#75740 = AXIS2_PLACEMENT_3D ( 'NONE', #11252, #9327, #100298 ) ;
#75741 = FACE_OUTER_BOUND ( 'NONE', #46557, .T. ) ;
#75742 = AXIS2_PLACEMENT_3D ( 'NONE', #105995, #16926, #86992 ) ;
#75743 = DIRECTION ( 'NONE',  ( 0.000000000000000000, 1.000000000000000000, 0.000000000000000000 ) ) ;
#75744 = CONICAL_SURFACE ( 'NONE', #79954, 0.09999999999999982514, 0.003490658503988666988 ) ;
#75745 = CIRCLE ( 'NONE', #123757, 0.1000000000000002554 ) ;
#75746 = LINE ( 'NONE', #16162, #19137 ) ;
#75747 = AXIS2_PLACEMENT_3D ( 'NONE', #109962, #108656, #18979 ) ;
#75748 = DIRECTION ( 'NONE',  ( 0.000000000000000000, 0.000000000000000000, 1.000000000000000000 ) ) ;
#75749 = ORIENTED_EDGE ( 'NONE', *, *, #80935, .F. ) ;
#75750 = AXIS2_PLACEMENT_3D ( 'NONE', #55566, #75833, #5157 ) ;
#75751 = ORIENTED_EDGE ( 'NONE', *, *, #119486, .F. ) ;
#75752 = ORIENTED_EDGE ( 'NONE', *, *, #21842, .T. ) ;
#75753 = CARTESIAN_POINT ( 'NONE',  ( 9.599999999999914380, 2.500000000000000000, -3.737306695894649700 ) ) ;
#75754 = FACE_OUTER_BOUND ( 'NONE', #45386, .T. ) ;
#75755 = DIRECTION ( 'NONE',  ( 0.000000000000000000, 1.000000000000000000, 0.000000000000000000 ) ) ;
#75756 = ORIENTED_EDGE ( 'NONE', *, *, #53473, .F. ) ;
#75757 = DIRECTION ( 'NONE',  ( 0.000000000000000000, 0.000000000000000000, -1.000000000000000000 ) ) ;
#75758 = EDGE_CURVE ( 'NONE', #34246, #28179, #34578, .T. ) ;
#75759 = EDGE_CURVE ( 'NONE', #72461, #72089, #7500, .T. ) ;
#75760 = CARTESIAN_POINT ( 'NONE',  ( 4.199999999999938005, 12.50000000000000000, 4.330127018922196314 ) ) ;
#75762 = EDGE_LOOP ( 'NONE', ( #99187, #118734, #108723, #23738 ) ) ;
#75761 = DIRECTION ( 'NONE',  ( -0.000000000000000000, 1.000000000000000000, -0.000000000000000000 ) ) ;
#75763 = CIRCLE ( 'NONE', #105307, 0.06509327318403745899 ) ;
#75764 = CARTESIAN_POINT ( 'NONE',  ( 9.599999999999914380, 2.500000000000000000, -3.637306695894650055 ) ) ;
#75765 = VERTEX_POINT ( 'NONE', #87339 ) ;
#75766 = EDGE_CURVE ( 'NONE', #123488, #102877, #77530, .T. ) ;
#75767 = ORIENTED_EDGE ( 'NONE', *, *, #19811, .T. ) ;
#75768 = VERTEX_POINT ( 'NONE', #28452 ) ;
#75769 = AXIS2_PLACEMENT_3D ( 'NONE', #63103, #123314, #43484 ) ;
#75770 = ORIENTED_EDGE ( 'NONE', *, *, #46470, .T. ) ;
#75771 = DIRECTION ( 'NONE',  ( 0.000000000000000000, 1.000000000000000000, 0.000000000000000000 ) ) ;
#75772 = AXIS2_PLACEMENT_3D ( 'NONE', #47745, #37285, #126947 ) ;
#75773 = DIRECTION ( 'NONE',  ( -4.274815082592931898E-19, -0.9999939076577903929, -0.003490651415223739937 ) ) ;
#75774 = CARTESIAN_POINT ( 'NONE',  ( 1.049999999999952083, 12.50000000000000000, 6.776507416713035248 ) ) ;
#75775 = DIRECTION ( 'NONE',  ( 0.000000000000000000, -0.9999939076577903929, 0.003490651415223739937 ) ) ;
#75777 = ORIENTED_EDGE ( 'NONE', *, *, #93483, .T. ) ;
#75776 = CIRCLE ( 'NONE', #67431, 0.1000000000000000472 ) ;
#75778 = AXIS2_PLACEMENT_3D ( 'NONE', #119076, #1228, #28116 ) ;
#75779 = CIRCLE ( 'NONE', #69429, 0.1000000000000002554 ) ;
#75780 = CARTESIAN_POINT ( 'NONE',  ( -9.400000000000007461, 12.50000000000000000, 3.918623584224382839 ) ) ;
#75782 = ORIENTED_EDGE ( 'NONE', *, *, #23540, .T. ) ;
#75781 = AXIS2_PLACEMENT_3D ( 'NONE', #119983, #41442, #110162 ) ;
#75783 = CARTESIAN_POINT ( 'NONE',  ( 6.649999999999929301, 2.500000000000000000, -2.065063509461102065 ) ) ;
#75784 = DIRECTION ( 'NONE',  ( 0.000000000000000000, 1.000000000000000000, 0.000000000000000000 ) ) ;
#75785 = CARTESIAN_POINT ( 'NONE',  ( -2.500000000000031086, 2.500000000000000000, 3.637306695894644726 ) ) ;
#75786 = DIRECTION ( 'NONE',  ( 0.000000000000000000, 1.000000000000000000, 0.000000000000000000 ) ) ;
#75787 = CIRCLE ( 'NONE', #46539, 0.1000000000000002554 ) ;
#75788 = ORIENTED_EDGE ( 'NONE', *, *, #117055, .T. ) ;
#75789 = VERTEX_POINT ( 'NONE', #108283 ) ;
#75790 = VERTEX_POINT ( 'NONE', #68356 ) ;
#75791 = DIRECTION ( 'NONE',  ( 0.000000000000000000, 1.000000000000000000, 0.000000000000000000 ) ) ;
#75792 = CARTESIAN_POINT ( 'NONE',  ( 3.749999999999940492, 2.500000000000000000, 5.802370205355744659 ) ) ;
#75793 = CARTESIAN_POINT ( 'NONE',  ( 0.3999999999999568345, 12.50000000000000000, -3.572213422710612374 ) ) ;
#75794 = FACE_BOUND ( 'NONE', #998, .T. ) ;
#75795 = DIRECTION ( 'NONE',  ( -0.000000000000000000, 1.000000000000000000, -0.000000000000000000 ) ) ;
#75796 = DIRECTION ( 'NONE',  ( 0.000000000000000000, 0.000000000000000000, -1.000000000000000000 ) ) ;
#75797 = CARTESIAN_POINT ( 'NONE',  ( 13.54999999999989768, 2.500000000000000000, -2.511473670974877948 ) ) ;
#75798 = FACE_OUTER_BOUND ( 'NONE', #38599, .T. ) ;
#75799 = AXIS2_PLACEMENT_3D ( 'NONE', #59238, #99149, #89320 ) ;
#75800 = ADVANCED_FACE ( 'NONE', ( #18616 ), #116946, .T. ) ;
#75801 = CARTESIAN_POINT ( 'NONE',  ( 185.7135416670080588, 4.367472073101518859, -7.564683531249999149 ) ) ;
#75802 = DIRECTION ( 'NONE',  ( 0.000000000000000000, 0.000000000000000000, -1.000000000000000000 ) ) ;
#75803 = CARTESIAN_POINT ( 'NONE',  ( -7.500000000000016875, 12.50000000000000000, -3.572213422710612374 ) ) ;
#75804 = AXIS2_PLACEMENT_3D ( 'NONE', #27154, #36981, #86721 ) ;
#75805 = AXIS2_PLACEMENT_3D ( 'NONE', #14770, #125406, #105769 ) ;
#75806 = CIRCLE ( 'NONE', #29856, 0.1000000000000002554 ) ;
#75807 = DIRECTION ( 'NONE',  ( 0.000000000000000000, 0.000000000000000000, 1.000000000000000000 ) ) ;
#75808 = ORIENTED_EDGE ( 'NONE', *, *, #35738, .F. ) ;
#75809 = ORIENTED_EDGE ( 'NONE', *, *, #7098, .T. ) ;
#75810 = ORIENTED_EDGE ( 'NONE', *, *, #60978, .F. ) ;
#75811 = ORIENTED_EDGE ( 'NONE', *, *, #32112, .T. ) ;
#75812 = EDGE_CURVE ( 'NONE', #34635, #71492, #6135, .T. ) ;
#75813 = PLANE ( 'NONE',  #19401 ) ;
#75814 = EDGE_CURVE ( 'NONE', #13385, #49583, #102308, .T. ) ;
#75815 = FACE_BOUND ( 'NONE', #4098, .T. ) ;
#75816 = AXIS2_PLACEMENT_3D ( 'NONE', #127015, #45877, #37348 ) ;
#75817 = CARTESIAN_POINT ( 'NONE',  ( -3.550000000000027356, 12.50000000000000000, -2.511473670974877948 ) ) ;
#75818 = CIRCLE ( 'NONE', #38279, 0.1000000000000002554 ) ;
#75819 = AXIS2_PLACEMENT_3D ( 'NONE', #21774, #41426, #109500 ) ;
#75820 = AXIS2_PLACEMENT_3D ( 'NONE', #9450, #49390, #110225 ) ;
#75821 = EDGE_LOOP ( 'NONE', ( #80437, #5165 ) ) ;
#75822 = CARTESIAN_POINT ( 'NONE',  ( 32.28071041560450993, 1.401423001988622019, 4.680142630335600629 ) ) ;
#75823 = ADVANCED_FACE ( 'NONE', ( #70942 ), #41771, .T. ) ;
#75824 = DIRECTION ( 'NONE',  ( -0.000000000000000000, -1.000000000000000000, -0.000000000000000000 ) ) ;
#75825 = ORIENTED_EDGE ( 'NONE', *, *, #2523, .F. ) ;
#75827 = LINE ( 'NONE', #115755, #55331 ) ;
#75826 = AXIS2_PLACEMENT_3D ( 'NONE', #10441, #88334, #120408 ) ;
#75828 = DIRECTION ( 'NONE',  ( -0.000000000000000000, -1.000000000000000000, -0.000000000000000000 ) ) ;
#75829 = VECTOR ( 'NONE', #41789, 1000.000000000000000 ) ;
#75830 = CONICAL_SURFACE ( 'NONE', #128174, 0.09999999999999999167, 0.003490658503988666988 ) ;
#75831 = CIRCLE ( 'NONE', #4717, 0.06509327318403745899 ) ;
#75832 = EDGE_LOOP ( 'NONE', ( #101869, #40886 ) ) ;
#75833 = DIRECTION ( 'NONE',  ( -0.000000000000000000, -1.000000000000000000, -0.000000000000000000 ) ) ;
#75834 = DIRECTION ( 'NONE',  ( 0.000000000000000000, 0.000000000000000000, 1.000000000000000000 ) ) ;
#75835 = ORIENTED_EDGE ( 'NONE', *, *, #28176, .T. ) ;
#75836 = DIRECTION ( 'NONE',  ( 0.000000000000000000, 0.000000000000000000, 1.000000000000000000 ) ) ;
#75837 = AXIS2_PLACEMENT_3D ( 'NONE', #117030, #48983, #27367 ) ;
#75838 = DIRECTION ( 'NONE',  ( 0.000000000000000000, 0.000000000000000000, 1.000000000000000000 ) ) ;
#75839 = VERTEX_POINT ( 'NONE', #10089 ) ;
#75840 = FACE_OUTER_BOUND ( 'NONE', #30732, .T. ) ;
#75841 = EDGE_LOOP ( 'NONE', ( #78929, #33298, #28111, #39345 ) ) ;
#75842 = ORIENTED_EDGE ( 'NONE', *, *, #35672, .T. ) ;
#75843 = FACE_OUTER_BOUND ( 'NONE', #22599, .T. ) ;
#75844 = VERTEX_POINT ( 'NONE', #50656 ) ;
#75845 = CARTESIAN_POINT ( 'NONE',  ( -13.34999999999999076, 2.500000000000000000, -1.472243186433547901 ) ) ;
#75846 = DIRECTION ( 'NONE',  ( 0.000000000000000000, 0.000000000000000000, 1.000000000000000000 ) ) ;
#75847 = EDGE_CURVE ( 'NONE', #127429, #3902, #4086, .T. ) ;
#75848 = VERTEX_POINT ( 'NONE', #253 ) ;
#75849 = DIRECTION ( 'NONE',  ( -0.000000000000000000, 1.000000000000000000, -0.000000000000000000 ) ) ;
#75850 = FACE_OUTER_BOUND ( 'NONE', #92414, .T. ) ;
#75851 = DIRECTION ( 'NONE',  ( 0.000000000000000000, 1.000000000000000000, 0.000000000000000000 ) ) ;
#75852 = CIRCLE ( 'NONE', #115855, 0.09999999999999982514 ) ;
#75853 = DIRECTION ( 'NONE',  ( -4.274815082592931898E-19, -0.9999939076577903929, -0.003490651415223739937 ) ) ;
#75854 = CONICAL_SURFACE ( 'NONE', #115551, 0.1000000000000002554, 0.003490658503988666988 ) ;
#75856 = EDGE_CURVE ( 'NONE', #124197, #119064, #64724, .T. ) ;
#75855 = CARTESIAN_POINT ( 'NONE',  ( -11.44999999999999929, 2.500000000000000000, -6.148780366869522673 ) ) ;
#75857 = CARTESIAN_POINT ( 'NONE',  ( 115.5000000000000000, -1.500000000000000222, -1.322875655532295136 ) ) ;
#75858 = EDGE_CURVE ( 'NONE', #122865, #1265, #77256, .T. ) ;
#75859 = ORIENTED_EDGE ( 'NONE', *, *, #123228, .F. ) ;
#75860 = ORIENTED_EDGE ( 'NONE', *, *, #58525, .T. ) ;
#75861 = CARTESIAN_POINT ( 'NONE',  ( 7.099999999999928590, 12.50000000000000000, -4.330127018922201643 ) ) ;
#75862 = AXIS2_PLACEMENT_3D ( 'NONE', #52010, #42858, #42185 ) ;
#75863 = CARTESIAN_POINT ( 'NONE',  ( -4.150000000000024336, 2.500000000000000000, 2.065063509461097624 ) ) ;
#75864 = ADVANCED_FACE ( 'NONE', ( #91231 ), #33364, .T. ) ;
#75866 = CARTESIAN_POINT ( 'NONE',  ( -8.100000000000010303, 2.500000000000000000, 3.983716857408420964 ) ) ;
#75865 = CIRCLE ( 'NONE', #17361, 0.09999999999999982514 ) ;
#75868 = EDGE_LOOP ( 'NONE', ( #98010, #69586, #3517, #62704 ) ) ;
#75867 = EDGE_LOOP ( 'NONE', ( #72997, #40020, #104628, #98054 ) ) ;
#75869 = ADVANCED_FACE ( 'NONE', ( #39581 ), #20825, .T. ) ;
#75870 = ORIENTED_EDGE ( 'NONE', *, *, #80285, .T. ) ;
#75871 = EDGE_CURVE ( 'NONE', #99834, #92562, #78853, .T. ) ;
#75872 = DIRECTION ( 'NONE',  ( 0.000000000000000000, 0.000000000000000000, -1.000000000000000000 ) ) ;
#75873 = DIRECTION ( 'NONE',  ( 0.000000000000000000, 0.000000000000000000, -1.000000000000000000 ) ) ;
#75874 = AXIS2_PLACEMENT_3D ( 'NONE', #32173, #81873, #80616 ) ;
#75876 = CARTESIAN_POINT ( 'NONE',  ( -4.600000000000028066, 2.500000000000000000, -5.022947341949754119 ) ) ;
#75875 = AXIS2_PLACEMENT_3D ( 'NONE', #59382, #118914, #48243 ) ;
#75877 = CONICAL_SURFACE ( 'NONE', #9074, 0.09999999999999982514, 0.003490658503988666988 ) ;
#75878 =( NAMED_UNIT ( * ) SI_UNIT ( $, .STERADIAN. ) SOLID_ANGLE_UNIT ( ) );
#75879 = EDGE_CURVE ( 'NONE', #83615, #122680, #21193, .T. ) ;
#75880 = LINE ( 'NONE', #56236, #88764 ) ;
#75881 = LINE ( 'NONE', #96162, #37711 ) ;
#75882 = CARTESIAN_POINT ( 'NONE',  ( -9.350000000000006750, 2.500000000000000000, 2.511473670974873507 ) ) ;
#75883 = AXIS2_PLACEMENT_3D ( 'NONE', #79107, #49650, #70552 ) ;
#75884 = DIRECTION ( 'NONE',  ( 0.000000000000000000, 0.000000000000000000, 1.000000000000000000 ) ) ;
#75885 = CARTESIAN_POINT ( 'NONE',  ( 14.39999999999989555, 2.500000000000000000, -0.4464101615137782142 ) ) ;
#75886 = AXIS2_PLACEMENT_3D ( 'NONE', #48138, #959, #21240 ) ;
#75888 = EDGE_CURVE ( 'NONE', #1361, #74448, #61121, .T. ) ;
#75887 = DIRECTION ( 'NONE',  ( 0.000000000000000000, 0.000000000000000000, 1.000000000000000000 ) ) ;
#75889 = CIRCLE ( 'NONE', #52914, 0.1000000000000000472 ) ;
#75890 = ORIENTED_EDGE ( 'NONE', *, *, #25010, .F. ) ;
#75891 = CARTESIAN_POINT ( 'NONE',  ( -4.150000000000028777, 12.50000000000000000, -5.802370205355749988 ) ) ;
#75892 = ORIENTED_EDGE ( 'NONE', *, *, #13485, .T. ) ;
#75893 = EDGE_LOOP ( 'NONE', ( #103738, #90771 ) ) ;
#75894 = CARTESIAN_POINT ( 'NONE',  ( 1.249999999999988898, 2.500000000000000000, -6.495190528383302464 ) ) ;
#75895 = PLANE ( 'NONE',  #63652 ) ;
#75896 = CARTESIAN_POINT ( 'NONE',  ( 195.5000000000000000, 0.000000000000000000, 0.000000000000000000 ) ) ;
#75897 = AXIS2_PLACEMENT_3D ( 'NONE', #102995, #13322, #6699 ) ;
#75898 = DIRECTION ( 'NONE',  ( 0.000000000000000000, -0.000000000000000000, 1.000000000000000000 ) ) ;
#75899 = DIRECTION ( 'NONE',  ( 0.000000000000000000, 1.000000000000000000, 0.000000000000000000 ) ) ;
#75900 = CARTESIAN_POINT ( 'NONE',  ( 8.349999999999919709, 12.50000000000000000, 6.430097255199259010 ) ) ;
#75901 = DIRECTION ( 'NONE',  ( 0.000000000000000000, 0.000000000000000000, 1.000000000000000000 ) ) ;
#75902 = VERTEX_POINT ( 'NONE', #89929 ) ;
#75903 = CARTESIAN_POINT ( 'NONE',  ( 2.949999999999946887, 12.50000000000000000, -2.165063509461101710 ) ) ;
#75904 = VECTOR ( 'NONE', #51967, 1000.000000000000000 ) ;
#75906 = CIRCLE ( 'NONE', #34150, 0.06509327318403745899 ) ;
#75905 = FACE_OUTER_BOUND ( 'NONE', #70606, .T. ) ;
#75907 = ORIENTED_EDGE ( 'NONE', *, *, #64061, .T. ) ;
#75908 = AXIS2_PLACEMENT_3D ( 'NONE', #121497, #63244, #51504 ) ;
#75909 = ORIENTED_EDGE ( 'NONE', *, *, #95607, .F. ) ;
#75910 = VERTEX_POINT ( 'NONE', #20558 ) ;
#75911 = ORIENTED_EDGE ( 'NONE', *, *, #49696, .T. ) ;
#75912 = VECTOR ( 'NONE', #125550, 1000.000000000000000 ) ;
#75913 = LINE ( 'NONE', #63532, #27404 ) ;
#75914 = DIRECTION ( 'NONE',  ( 0.000000000000000000, 0.000000000000000000, 1.000000000000000000 ) ) ;
#75915 = AXIS2_PLACEMENT_3D ( 'NONE', #92152, #91515, #32630 ) ;
#75916 = AXIS2_PLACEMENT_3D ( 'NONE', #51086, #99537, #88393 ) ;
#75917 = CARTESIAN_POINT ( 'NONE',  ( 6.249999999999932498, 12.50000000000000000, -5.802370205355749988 ) ) ;
#75918 = CONICAL_SURFACE ( 'NONE', #605, 0.1000000000000000056, 0.003490658503988666988 ) ;
#75919 = ADVANCED_FACE ( 'NONE', ( #69651 ), #50091, .T. ) ;
#75920 = DIRECTION ( 'NONE',  ( 0.000000000000000000, -0.000000000000000000, 1.000000000000000000 ) ) ;
#75921 = CARTESIAN_POINT ( 'NONE',  ( 2.299999999999949640, 2.500000000000000000, -0.3464101615137782364 ) ) ;
#75922 = VERTEX_POINT ( 'NONE', #120690 ) ;
#75923 = LINE ( 'NONE', #3961, #28579 ) ;
#75925 = EDGE_CURVE ( 'NONE', #80146, #99999, #75198, .T. ) ;
#75924 = CARTESIAN_POINT ( 'NONE',  ( 187.0312500006828031, 9.429780353434619030E-16, -7.700000000000000178 ) ) ;
#75926 = ORIENTED_EDGE ( 'NONE', *, *, #70981, .F. ) ;
#75927 = CIRCLE ( 'NONE', #19492, 0.06509327318403745899 ) ;
#75928 = ORIENTED_EDGE ( 'NONE', *, *, #91991, .T. ) ;
#75929 = VERTEX_POINT ( 'NONE', #31665 ) ;
#75930 = DIRECTION ( 'NONE',  ( 0.000000000000000000, 1.000000000000000000, 0.000000000000000000 ) ) ;
#75931 = CONICAL_SURFACE ( 'NONE', #36242, 0.1000000000000002554, 0.003490658503988666988 ) ;
#75932 = PLANE ( 'NONE',  #46679 ) ;
#75933 = DIRECTION ( 'NONE',  ( 0.000000000000000000, -0.000000000000000000, 1.000000000000000000 ) ) ;
#75934 = ORIENTED_EDGE ( 'NONE', *, *, #27823, .F. ) ;
#75935 = DIRECTION ( 'NONE',  ( 0.000000000000000000, 1.000000000000000000, 0.000000000000000000 ) ) ;
#75936 = DIRECTION ( 'NONE',  ( 1.000000000000000000, 0.000000000000000000, 0.000000000000000000 ) ) ;
#75937 = DIRECTION ( 'NONE',  ( -0.000000000000000000, 1.000000000000000000, -0.000000000000000000 ) ) ;
#75938 = DIRECTION ( 'NONE',  ( -4.274815082592931898E-19, -0.9999939076577903929, -0.003490651415223739937 ) ) ;
#75939 = CARTESIAN_POINT ( 'NONE',  ( 4.399999999999939071, 2.500000000000000000, 0.3464101615137736845 ) ) ;
#75940 = ORIENTED_EDGE ( 'NONE', *, *, #61896, .T. ) ;
#75941 = CARTESIAN_POINT ( 'NONE',  ( -7.900000000000014566, 2.500000000000000000, -3.637306695894650055 ) ) ;
#75942 = ORIENTED_EDGE ( 'NONE', *, *, #93162, .F. ) ;
#75943 = VERTEX_POINT ( 'NONE', #58557 ) ;
#75944 = VECTOR ( 'NONE', #98737, 1000.000000000000000 ) ;
#75945 = VERTEX_POINT ( 'NONE', #19243 ) ;
#75946 = AXIS2_PLACEMENT_3D ( 'NONE', #31424, #62814, #81164 ) ;
#75947 = DIRECTION ( 'NONE',  ( 0.000000000000000000, 1.000000000000000000, 0.000000000000000000 ) ) ;
#75948 = FACE_BOUND ( 'NONE', #37411, .T. ) ;
#75949 = CARTESIAN_POINT ( 'NONE',  ( 2.099999999999947686, 12.50000000000000000, 4.957854068765711553 ) ) ;
#75950 = CARTESIAN_POINT ( 'NONE',  ( -5.600000000000020073, 2.500000000000000000, 3.983716857408420964 ) ) ;
#75951 = FACE_OUTER_BOUND ( 'NONE', #86180, .T. ) ;
#75952 = EDGE_CURVE ( 'NONE', #3331, #125340, #73052, .T. ) ;
#75953 = CIRCLE ( 'NONE', #6982, 0.1000000000000000472 ) ;
#75954 = VECTOR ( 'NONE', #17457, 1000.000000000000000 ) ;
#75955 = AXIS2_PLACEMENT_3D ( 'NONE', #105939, #16242, #56182 ) ;
#75956 = AXIS2_PLACEMENT_3D ( 'NONE', #10962, #81026, #24045 ) ;
#75957 = CIRCLE ( 'NONE', #17462, 0.09999999999999982514 ) ;
#75958 = EDGE_LOOP ( 'NONE', ( #119274, #54116, #22344, #29662 ) ) ;
#75959 = DIRECTION ( 'NONE',  ( 0.000000000000000000, 0.000000000000000000, 1.000000000000000000 ) ) ;
#75960 = CARTESIAN_POINT ( 'NONE',  ( 11.44999999999991047, 2.500000000000000000, -2.511473670974877948 ) ) ;
#75961 = DIRECTION ( 'NONE',  ( 0.000000000000000000, 0.000000000000000000, -1.000000000000000000 ) ) ;
#75962 = CARTESIAN_POINT ( 'NONE',  ( 17.50000000000000000, 2.500000000000000000, 0.000000000000000000 ) ) ;
#75963 = VERTEX_POINT ( 'NONE', #51326 ) ;
#75964 = EDGE_CURVE ( 'NONE', #115280, #59105, #71583, .T. ) ;
#75966 = CARTESIAN_POINT ( 'NONE',  ( -3.750000000000025757, 2.500000000000000000, 1.572243186433545548 ) ) ;
#75965 = AXIS2_PLACEMENT_3D ( 'NONE', #35378, #75286, #125661 ) ;
#75967 = CONICAL_SURFACE ( 'NONE', #55043, 0.1000000000000002554, 0.003490658503988666988 ) ;
#75968 = CIRCLE ( 'NONE', #19537, 0.09999999999999982514 ) ;
#75969 = DIRECTION ( 'NONE',  ( -0.000000000000000000, -1.000000000000000000, -0.000000000000000000 ) ) ;
#75970 = CONICAL_SURFACE ( 'NONE', #59278, 0.1000000000000000056, 0.003490658503988666988 ) ;
#75971 = ORIENTED_EDGE ( 'NONE', *, *, #121845, .T. ) ;
#75972 = AXIS2_PLACEMENT_3D ( 'NONE', #95712, #104235, #15184 ) ;
#75973 = EDGE_CURVE ( 'NONE', #129104, #97216, #110694, .T. ) ;
#75974 = CARTESIAN_POINT ( 'NONE',  ( 5.849999999999935696, 12.50000000000000000, -6.495190528383302464 ) ) ;
#75975 = EDGE_CURVE ( 'NONE', #50100, #123233, #81466, .T. ) ;
#75976 = FACE_BOUND ( 'NONE', #33230, .T. ) ;
#75977 = AXIS2_PLACEMENT_3D ( 'NONE', #106666, #37302, #36009 ) ;
#75978 = CARTESIAN_POINT ( 'NONE',  ( -13.94999999999998863, 12.50000000000000000, 2.446380397790839822 ) ) ;
#75979 = VERTEX_POINT ( 'NONE', #93176 ) ;
#75980 = CARTESIAN_POINT ( 'NONE',  ( 9.549999999999915445, 12.50000000000000000, 6.495190528383297135 ) ) ;
#75981 = CARTESIAN_POINT ( 'NONE',  ( 11.84999999999990727, 2.500000000000000000, -2.511473670974877948 ) ) ;
#75982 = ADVANCED_FACE ( 'NONE', ( #54510 ), #18758, .T. ) ;
#75983 = ORIENTED_EDGE ( 'NONE', *, *, #64645, .F. ) ;
#75984 = EDGE_LOOP ( 'NONE', ( #124997, #28559 ) ) ;
#75985 = ADVANCED_FACE ( 'NONE', ( #63057 ), #112771, .T. ) ;
#75986 = CARTESIAN_POINT ( 'NONE',  ( 184.3802083336747444, 4.367472073101515306, 7.564683531250000925 ) ) ;
#75987 = EDGE_LOOP ( 'NONE', ( #79245, #76207, #87426, #5164 ) ) ;
#75988 = CARTESIAN_POINT ( 'NONE',  ( 11.84999999999990372, 2.500000000000000000, 2.611473670974873151 ) ) ;
#75989 = DIRECTION ( 'NONE',  ( 0.000000000000000000, 0.000000000000000000, 1.000000000000000000 ) ) ;
#75990 = FACE_OUTER_BOUND ( 'NONE', #118192, .T. ) ;
#75991 = FACE_OUTER_BOUND ( 'NONE', #78430, .T. ) ;
#75992 = FACE_OUTER_BOUND ( 'NONE', #95186, .T. ) ;
#75993 = VECTOR ( 'NONE', #79804, 1000.000000000000000 ) ;
#75994 = VECTOR ( 'NONE', #123786, 1000.000000000000000 ) ;
#75995 = TOROIDAL_SURFACE ( 'NONE', #19573, 4.500000000000003553, 0.5000000000000000000 ) ;
#75996 = ORIENTED_EDGE ( 'NONE', *, *, #118435, .T. ) ;
#75997 = DIRECTION ( 'NONE',  ( 0.000000000000000000, -0.9999939076577903929, 0.003490651415223739937 ) ) ;
#75998 = FACE_OUTER_BOUND ( 'NONE', #3611, .T. ) ;
#75999 = DIRECTION ( 'NONE',  ( 0.000000000000000000, 0.000000000000000000, 1.000000000000000000 ) ) ;
#76000 = DIRECTION ( 'NONE',  ( 0.000000000000000000, -0.000000000000000000, 1.000000000000000000 ) ) ;
#76002 = VERTEX_POINT ( 'NONE', #12649 ) ;
#76001 = EDGE_LOOP ( 'NONE', ( #20732, #108923 ) ) ;
#76003 = FACE_BOUND ( 'NONE', #12127, .T. ) ;
#76004 = ORIENTED_EDGE ( 'NONE', *, *, #64193, .F. ) ;
#76005 = AXIS2_PLACEMENT_3D ( 'NONE', #84981, #7703, #77109 ) ;
#76006 = DIRECTION ( 'NONE',  ( 0.000000000000000000, 0.000000000000000000, -1.000000000000000000 ) ) ;
#76007 = CARTESIAN_POINT ( 'NONE',  ( -2.500000000000032419, 2.500000000000000000, -3.737306695894649700 ) ) ;
#76008 = AXIS2_PLACEMENT_3D ( 'NONE', #93296, #25848, #4894 ) ;
#76009 = ORIENTED_EDGE ( 'NONE', *, *, #37059, .F. ) ;
#76011 = PLANE ( 'NONE',  #38613 ) ;
#76010 = AXIS2_PLACEMENT_3D ( 'NONE', #34512, #104511, #6290 ) ;
#76012 = LINE ( 'NONE', #115937, #5547 ) ;
#76013 = VECTOR ( 'NONE', #62902, 1000.000000000000000 ) ;
#76014 = EDGE_CURVE ( 'NONE', #21053, #16047, #16596, .T. ) ;
#76015 = DIRECTION ( 'NONE',  ( 0.000000000000000000, 0.000000000000000000, 1.000000000000000000 ) ) ;
#76016 = CARTESIAN_POINT ( 'NONE',  ( 14.14999999999989555, 2.500000000000000000, 2.265063509461097357 ) ) ;
#76017 = ORIENTED_EDGE ( 'NONE', *, *, #120514, .F. ) ;
#76018 = CARTESIAN_POINT ( 'NONE',  ( 3.099999999999943245, 2.500000000000000000, 3.883716857408420431 ) ) ;
#76019 = CARTESIAN_POINT ( 'NONE',  ( -10.40000000000000213, 12.50000000000000000, -5.022947341949749678 ) ) ;
#76020 = CARTESIAN_POINT ( 'NONE',  ( 108.0000000000000142, 9.000000000000001776, 0.2500000000000000000 ) ) ;
#76021 = CARTESIAN_POINT ( 'NONE',  ( 108.0000000000000142, 9.000000000000001776, 0.000000000000000000 ) ) ;
#76022 = CIRCLE ( 'NONE', #21741, 0.1000000000000000056 ) ;
#76023 = DIRECTION ( 'NONE',  ( 0.000000000000000000, 0.000000000000000000, 1.000000000000000000 ) ) ;
#76024 = EDGE_CURVE ( 'NONE', #109299, #100844, #41800, .T. ) ;
#76025 = EDGE_LOOP ( 'NONE', ( #30327, #57360, #45529, #110672 ) ) ;
#76026 = ORIENTED_EDGE ( 'NONE', *, *, #23226, .F. ) ;
#76027 = DIRECTION ( 'NONE',  ( 0.000000000000000000, 1.000000000000000000, -1.846105847067148761E-16 ) ) ;
#76029 = EDGE_LOOP ( 'NONE', ( #37598, #28187, #122511, #106203 ) ) ;
#76028 = VECTOR ( 'NONE', #23815, 1000.000000000000000 ) ;
#76030 = AXIS2_PLACEMENT_3D ( 'NONE', #12631, #72857, #2824 ) ;
#76031 = CIRCLE ( 'NONE', #48858, 0.1000000000000002554 ) ;
#76032 = DIRECTION ( 'NONE',  ( -0.000000000000000000, 1.000000000000000000, -0.000000000000000000 ) ) ;
#76033 = EDGE_CURVE ( 'NONE', #27968, #126401, #27086, .T. ) ;
#76035 = ORIENTED_EDGE ( 'NONE', *, *, #9401, .T. ) ;
#76034 = EDGE_LOOP ( 'NONE', ( #114907, #71933 ) ) ;
#76036 = ORIENTED_EDGE ( 'NONE', *, *, #11933, .F. ) ;
#76037 = AXIS2_PLACEMENT_3D ( 'NONE', #78917, #29170, #69069 ) ;
#76038 = EDGE_CURVE ( 'NONE', #77490, #109874, #123235, .T. ) ;
#76039 = DIRECTION ( 'NONE',  ( -0.000000000000000000, 1.000000000000000000, -0.000000000000000000 ) ) ;
#76040 = ADVANCED_FACE ( 'NONE', ( #44059 ), #121983, .T. ) ;
#76041 = VECTOR ( 'NONE', #76793, 1000.000000000000000 ) ;
#76042 = CARTESIAN_POINT ( 'NONE',  ( 108.0000000000000142, 8.500000000000000000, 0.000000000000000000 ) ) ;
#76043 = SHAPE_REPRESENTATION_RELATIONSHIP ( 'NONE' , 'NONE' ,  #125483, #122749 ) ;
#76044 = EDGE_CURVE ( 'NONE', #87068, #8340, #100250, .T. ) ;
#76045 = DIRECTION ( 'NONE',  ( -4.274815082592931898E-19, -0.9999939076577903929, -0.003490651415223739937 ) ) ;
#76046 = DIRECTION ( 'NONE',  ( 0.000000000000000000, -0.9999939076577903929, 0.003490651415223739937 ) ) ;
#76047 = CARTESIAN_POINT ( 'NONE',  ( 5.849999999999933920, 2.500000000000000000, 5.702370205355745014 ) ) ;
#76048 = EDGE_LOOP ( 'NONE', ( #120808, #56086 ) ) ;
#76050 = ADVANCED_FACE ( 'NONE', ( #33604 ), #52129, .T. ) ;
#76049 = DIRECTION ( 'NONE',  ( 0.000000000000000000, 0.000000000000000000, 1.000000000000000000 ) ) ;
#76051 = ORIENTED_EDGE ( 'NONE', *, *, #102189, .F. ) ;
#76052 = EDGE_CURVE ( 'NONE', #59346, #110796, #108556, .T. ) ;
#76053 = ORIENTED_EDGE ( 'NONE', *, *, #52192, .F. ) ;
#76054 = ORIENTED_EDGE ( 'NONE', *, *, #119846, .T. ) ;
#76055 = ORIENTED_EDGE ( 'NONE', *, *, #40424, .F. ) ;
#76056 = CARTESIAN_POINT ( 'NONE',  ( -3.550000000000028244, 2.500000000000000000, -1.918653347947326004 ) ) ;
#76057 = AXIS2_PLACEMENT_3D ( 'NONE', #82466, #113183, #33370 ) ;
#76058 = ORIENTED_EDGE ( 'NONE', *, *, #89151, .T. ) ;
#76059 = ORIENTED_EDGE ( 'NONE', *, *, #26242, .T. ) ;
#76061 = DIRECTION ( 'NONE',  ( 0.000000000000000000, 1.000000000000000000, 0.000000000000000000 ) ) ;
#76060 = CONICAL_SURFACE ( 'NONE', #69800, 0.1000000000000000472, 0.003490658503988666988 ) ;
#76062 = AXIS2_PLACEMENT_3D ( 'NONE', #11182, #113096, #52897 ) ;
#76063 = DIRECTION ( 'NONE',  ( 0.000000000000000000, 0.000000000000000000, -1.000000000000000000 ) ) ;
#76064 = DIRECTION ( 'NONE',  ( -4.274815082592931898E-19, -0.9999939076577903929, -0.003490651415223739937 ) ) ;
#76065 = DIRECTION ( 'NONE',  ( -4.274815082592931898E-19, -0.9999939076577903929, -0.003490651415223739937 ) ) ;
#76066 = CONICAL_SURFACE ( 'NONE', #30112, 0.1000000000000000472, 0.003490658503988666988 ) ;
#76067 = CONICAL_SURFACE ( 'NONE', #25886, 0.1000000000000000472, 0.003490658503988666988 ) ;
#76068 = CARTESIAN_POINT ( 'NONE',  ( 0.8499999999999550138, 2.500000000000000000, -5.802370205355749988 ) ) ;
#76069 = ORIENTED_EDGE ( 'NONE', *, *, #44369, .T. ) ;
#76070 = CARTESIAN_POINT ( 'NONE',  ( 13.14999999999990088, 2.500000000000000000, 1.718653347947321386 ) ) ;
#76071 = AXIS2_PLACEMENT_3D ( 'NONE', #72576, #32669, #82403 ) ;
#76073 = ORIENTED_EDGE ( 'NONE', *, *, #6933, .T. ) ;
#76072 = CIRCLE ( 'NONE', #55145, 0.1000000000000000472 ) ;
#76074 = DIRECTION ( 'NONE',  ( 0.000000000000000000, -0.000000000000000000, 1.000000000000000000 ) ) ;
#76075 = AXIS2_PLACEMENT_3D ( 'NONE', #65671, #97074, #5456 ) ;
#76076 = EDGE_LOOP ( 'NONE', ( #109084, #63772, #66663, #54619 ) ) ;
#76077 = CARTESIAN_POINT ( 'NONE',  ( 4.599999999999938360, 2.500000000000000000, -0.1000000000000022815 ) ) ;
#76078 = EDGE_LOOP ( 'NONE', ( #70238, #128513 ) ) ;
#76079 = CIRCLE ( 'NONE', #61429, 0.06509327318403745899 ) ;
#76080 = ORIENTED_EDGE ( 'NONE', *, *, #86879, .F. ) ;
#76081 = CARTESIAN_POINT ( 'NONE',  ( -11.69999999999999929, 2.500000000000000000, 1.734723475976807094E-15 ) ) ;
#76082 = LINE ( 'NONE', #74797, #115327 ) ;
#76083 = FACE_OUTER_BOUND ( 'NONE', #96462, .T. ) ;
#76084 = EDGE_CURVE ( 'NONE', #129577, #121671, #125284, .T. ) ;
#76085 = DIRECTION ( 'NONE',  ( 0.000000000000000000, 0.000000000000000000, -1.000000000000000000 ) ) ;
#76086 = DIRECTION ( 'NONE',  ( 0.000000000000000000, 1.000000000000000000, 0.000000000000000000 ) ) ;
#76087 = VERTEX_POINT ( 'NONE', #4753 ) ;
#76088 = DIRECTION ( 'NONE',  ( 0.000000000000000000, -0.9999939076577903929, 0.003490651415223739937 ) ) ;
#76089 = FACE_OUTER_BOUND ( 'NONE', #56225, .T. ) ;
#76090 = CARTESIAN_POINT ( 'NONE',  ( 1.249999999999952038, 2.500000000000000000, -1.372243186433550033 ) ) ;
#76091 = FACE_OUTER_BOUND ( 'NONE', #23665, .T. ) ;
#76093 = EDGE_CURVE ( 'NONE', #39360, #20166, #8377, .T. ) ;
#76092 = CARTESIAN_POINT ( 'NONE',  ( -6.450000000000016165, 2.500000000000000000, 6.841600689897072485 ) ) ;
#76094 = ORIENTED_EDGE ( 'NONE', *, *, #36886, .T. ) ;
#76095 = ORIENTED_EDGE ( 'NONE', *, *, #89151, .F. ) ;
#76096 = CARTESIAN_POINT ( 'NONE',  ( -5.000000000000023093, 12.50000000000000000, 4.957854068765711553 ) ) ;
#76097 = EDGE_LOOP ( 'NONE', ( #96995, #19786 ) ) ;
#76098 = AXIS2_PLACEMENT_3D ( 'NONE', #2404, #112393, #82292 ) ;
#76099 = DIRECTION ( 'NONE',  ( 0.000000000000000000, 1.000000000000000000, 0.000000000000000000 ) ) ;
#76100 = DIRECTION ( 'NONE',  ( 0.000000000000000000, -0.000000000000000000, 1.000000000000000000 ) ) ;
#76101 = AXIS2_PLACEMENT_3D ( 'NONE', #56317, #47810, #105437 ) ;
#76102 = ORIENTED_EDGE ( 'NONE', *, *, #102189, .T. ) ;
#76103 = CARTESIAN_POINT ( 'NONE',  ( 185.9583333333333428, 4.445597072760117285, 7.699999999999999289 ) ) ;
#76104 = CARTESIAN_POINT ( 'NONE',  ( 9.399999999999915090, 2.500000000000000000, -3.983716857408426293 ) ) ;
#76105 = CARTESIAN_POINT ( 'NONE',  ( 13.34999999999989662, 2.500000000000000000, -2.065063509461102065 ) ) ;
#76106 = DIRECTION ( 'NONE',  ( 0.000000000000000000, 0.000000000000000000, 1.000000000000000000 ) ) ;
#76107 = AXIS2_PLACEMENT_3D ( 'NONE', #20764, #107852, #69869 ) ;
#76108 = DIRECTION ( 'NONE',  ( 0.000000000000000000, -0.000000000000000000, 1.000000000000000000 ) ) ;
#76109 = EDGE_LOOP ( 'NONE', ( #119300, #126884, #76167, #73112 ) ) ;
#76110 = VECTOR ( 'NONE', #108230, 1000.000000000000000 ) ;
#76111 = AXIS2_PLACEMENT_3D ( 'NONE', #23289, #52753, #94604 ) ;
#76112 = CARTESIAN_POINT ( 'NONE',  ( -10.65000000000000391, 12.50000000000000000, -6.148780366869522673 ) ) ;
#76113 = DIRECTION ( 'NONE',  ( 0.000000000000000000, -0.9999939076577903929, 0.003490651415223739937 ) ) ;
#76114 = ORIENTED_EDGE ( 'NONE', *, *, #103961, .F. ) ;
#76115 = DIRECTION ( 'NONE',  ( 0.000000000000000000, -0.000000000000000000, 1.000000000000000000 ) ) ;
#76116 = DIRECTION ( 'NONE',  ( -0.000000000000000000, 1.000000000000000000, -0.000000000000000000 ) ) ;
#76117 = LINE ( 'NONE', #95759, #23973 ) ;
#76118 = EDGE_LOOP ( 'NONE', ( #122585, #30589, #106035, #57707 ) ) ;
#76119 = CIRCLE ( 'NONE', #67796, 0.1000000000000002554 ) ;
#76120 = AXIS2_PLACEMENT_3D ( 'NONE', #67877, #77689, #120215 ) ;
#76121 = VECTOR ( 'NONE', #68236, 1000.000000000000000 ) ;
#76122 = CARTESIAN_POINT ( 'NONE',  ( -12.09999999999999432, 2.500000000000000000, 3.637306695894644726 ) ) ;
#76124 = ORIENTED_EDGE ( 'NONE', *, *, #53003, .T. ) ;
#76123 = VECTOR ( 'NONE', #34975, 1000.000000000000000 ) ;
#76125 = DIRECTION ( 'NONE',  ( -0.000000000000000000, 1.000000000000000000, -0.000000000000000000 ) ) ;
#76126 = CARTESIAN_POINT ( 'NONE',  ( 6.249999999999932498, 2.500000000000000000, -5.702370205355749455 ) ) ;
#76127 = DIRECTION ( 'NONE',  ( 0.000000000000000000, 0.000000000000000000, 1.000000000000000000 ) ) ;
#76128 = VECTOR ( 'NONE', #68560, 1000.000000000000000 ) ;
#76129 = EDGE_LOOP ( 'NONE', ( #109451, #89135, #47250, #11880 ) ) ;
#76130 = EDGE_CURVE ( 'NONE', #76377, #2854, #106582, .T. ) ;
#76131 = CARTESIAN_POINT ( 'NONE',  ( -4.350000000000027178, 2.500000000000000000, -6.148780366869526226 ) ) ;
#76132 = DIRECTION ( 'NONE',  ( 0.000000000000000000, -0.000000000000000000, 1.000000000000000000 ) ) ;
#76133 = ORIENTED_EDGE ( 'NONE', *, *, #24452, .F. ) ;
#76134 = ADVANCED_FACE ( 'NONE', ( #112163 ), #58578, .T. ) ;
#76135 = EDGE_CURVE ( 'NONE', #33970, #18481, #21863, .T. ) ;
#76136 = ORIENTED_EDGE ( 'NONE', *, *, #58988, .T. ) ;
#76137 = CARTESIAN_POINT ( 'NONE',  ( 5.849999999999933031, 2.500000000000000000, -1.572243186433550211 ) ) ;
#76138 = ORIENTED_EDGE ( 'NONE', *, *, #55909, .F. ) ;
#76139 = CARTESIAN_POINT ( 'NONE',  ( 4.799999999999934097, 12.50000000000000000, 4.676537180435972552 ) ) ;
#76140 = DIRECTION ( 'NONE',  ( 0.000000000000000000, -0.000000000000000000, 1.000000000000000000 ) ) ;
#76141 = EDGE_CURVE ( 'NONE', #112646, #127507, #104532, .T. ) ;
#76142 = VECTOR ( 'NONE', #97325, 1000.000000000000000 ) ;
#76143 = ADVANCED_FACE ( 'NONE', ( #51962 ), #14622, .T. ) ;
#76144 = CIRCLE ( 'NONE', #46907, 0.06509327318403745899 ) ;
#76145 = CIRCLE ( 'NONE', #105392, 0.1000000000000000472 ) ;
#76146 = ORIENTED_EDGE ( 'NONE', *, *, #45395, .F. ) ;
#76147 = ADVANCED_FACE ( 'NONE', ( #95101 ), #10443, .T. ) ;
#76148 = DIRECTION ( 'NONE',  ( 0.000000000000000000, 1.000000000000000000, 0.000000000000000000 ) ) ;
#76149 = CARTESIAN_POINT ( 'NONE',  ( 14.14999999999989377, 2.500000000000000000, -1.472243186433550122 ) ) ;
#76150 = ORIENTED_EDGE ( 'NONE', *, *, #43661, .F. ) ;
#76151 = PLANE ( 'NONE',  #19641 ) ;
#76153 = CARTESIAN_POINT ( 'NONE',  ( -0.8000000000000376810, 2.500000000000000000, -4.330127018922201643 ) ) ;
#76152 = AXIS2_PLACEMENT_3D ( 'NONE', #23479, #40066, #111870 ) ;
#76154 = AXIS2_PLACEMENT_3D ( 'NONE', #41015, #120837, #10239 ) ;
#76155 = AXIS2_PLACEMENT_3D ( 'NONE', #75445, #113447, #55816 ) ;
#76156 = AXIS2_PLACEMENT_3D ( 'NONE', #100202, #88427, #49189 ) ;
#76157 = CARTESIAN_POINT ( 'NONE',  ( 17.34779069867702361, -2.317761454549422506, -4.873653559264009338 ) ) ;
#76158 = DIRECTION ( 'NONE',  ( 0.000000000000000000, -0.9999939076577903929, 0.003490651415223739937 ) ) ;
#76159 = DIRECTION ( 'NONE',  ( 0.000000000000000000, 1.000000000000000000, 0.000000000000000000 ) ) ;
#76160 = FACE_OUTER_BOUND ( 'NONE', #50101, .T. ) ;
#76161 = AXIS2_PLACEMENT_3D ( 'NONE', #77700, #8959, #126820 ) ;
#76162 = AXIS2_PLACEMENT_3D ( 'NONE', #50312, #71229, #52890 ) ;
#76163 = AXIS2_PLACEMENT_3D ( 'NONE', #90459, #32224, #111385 ) ;
#76164 = ORIENTED_EDGE ( 'NONE', *, *, #22269, .F. ) ;
#76165 = ORIENTED_EDGE ( 'NONE', *, *, #37875, .T. ) ;
#76166 = ORIENTED_EDGE ( 'NONE', *, *, #47971, .F. ) ;
#76167 = ORIENTED_EDGE ( 'NONE', *, *, #119498, .T. ) ;
#76168 = DIRECTION ( 'NONE',  ( 0.000000000000000000, 1.000000000000000000, 0.000000000000000000 ) ) ;
#76169 = DIRECTION ( 'NONE',  ( 0.000000000000000000, 0.000000000000000000, 1.000000000000000000 ) ) ;
#76170 = AXIS2_PLACEMENT_3D ( 'NONE', #26811, #87011, #75901 ) ;
#76171 = DIRECTION ( 'NONE',  ( 0.000000000000000000, 0.000000000000000000, -1.000000000000000000 ) ) ;
#76172 = ORIENTED_EDGE ( 'NONE', *, *, #21456, .T. ) ;
#76173 = FACE_BOUND ( 'NONE', #108806, .T. ) ;
#76174 = DIRECTION ( 'NONE',  ( -0.000000000000000000, -1.000000000000000000, -0.000000000000000000 ) ) ;
#76175 = CARTESIAN_POINT ( 'NONE',  ( -3.950000000000025491, 12.50000000000000000, 6.148780366869520897 ) ) ;
#76176 = DIRECTION ( 'NONE',  ( 0.000000000000000000, 1.000000000000000000, 0.000000000000000000 ) ) ;
#76177 = DIRECTION ( 'NONE',  ( -0.000000000000000000, -1.000000000000000000, -0.000000000000000000 ) ) ;
#76178 = CARTESIAN_POINT ( 'NONE',  ( 16.87640210516308770, -2.500000000000000000, -4.436424697255247906 ) ) ;
#76179 = DIRECTION ( 'NONE',  ( 0.000000000000000000, 0.000000000000000000, -1.000000000000000000 ) ) ;
#76181 = FACE_OUTER_BOUND ( 'NONE', #109557, .T. ) ;
#76180 =( BOUNDED_SURFACE ( )  B_SPLINE_SURFACE ( 1, 2, ( 
 ( #39724, #82199, #81551, #121458, #71732, #40352, #29244, #80269, #119528, #69797, #19390, #54648, #114863, #122765, #102478, #25194, #103121, #114235, #13440, #93953, #62572, #122132, #32482, #72392, #112306, #33117, #92658, #22646, #12787, #4904, #52730, #112944, #2996, #23257, #44192, #84117, #42947, #54027, #82858, #73019, #65111, #123397, #105040, #63200, #53388, #93308, #94578, #15362, #74315, #124046, #3631, #24562, #55320, #43580, #83499, #33737, #64481, #95244, #73647, #113592, #45510, #23930, #63848, #103775, #14076, #34408, #5554, #4252, #104412, #14718, #44861, #84774, #124704, #35049, #74956, #127918, #75582, #58550, #115498, #38262, #86703, #77522, #27144, #78185, #106969 ),
 ( #25855, #35678, #97807, #65764, #76250, #105710, #116152, #7489, #47435, #16013, #17287, #55948, #36341, #118090, #126638, #28439, #95885, #6192, #46134, #17958, #68349, #37619, #67697, #57906, #86035, #108275, #125971, #117419, #125343, #67038, #18606, #26507, #8132, #87331, #66411, #127287, #106344, #16653, #27772, #56579, #98440, #8765, #36969, #107638, #96500, #76889, #48082, #6822, #116794, #87967, #85413, #46791, #57245, #97169, #81411, #31036, #49380, #10080, #40856, #60490, #89919, #30384, #80112, #78842, #91219, #48727, #51315, #80763, #120682, #41501, #29716, #99113, #128593, #70933, #21850, #50029, #1536, #31654, #89285, #79479, #121317, #70294, #119374, #40190, #71570 ) ),
 .UNSPECIFIED., .F., .F., .F. ) 
 B_SPLINE_SURFACE_WITH_KNOTS ( ( 2, 2 ),
 ( 3, 2, 2, 2, 2, 2, 2, 2, 2, 2, 2, 2, 2, 2, 2, 2, 2, 2, 2, 2, 2, 2, 2, 2, 2, 2, 2, 2, 2, 2, 2, 2, 2, 2, 2, 2, 2, 2, 2, 2, 2, 2, 3 ),
 ( 0.000000000000000000, 1.000000000000000000 ),
 ( 0.000000000000000000, 0.02380952380952380820, 0.04761904761904761640, 0.07142857142857142461, 0.09523809523809523281, 0.1190476190476190410, 0.1428571428571428492, 0.1666666666666666574, 0.1904761904761904656, 0.2142857142857142738, 0.2380952380952380820, 0.2619047619047619180, 0.2857142857142856984, 0.3095238095238095344, 0.3333333333333333148, 0.3571428571428571508, 0.3809523809523809312, 0.4047619047619047672, 0.4285714285714285476, 0.4523809523809523836, 0.4761904761904761640, 0.5000000000000000000, 0.5238095238095238360, 0.5476190476190476719, 0.5714285714285713969, 0.5952380952380952328, 0.6190476190476190688, 0.6428571428571429047, 0.6666666666666666297, 0.6904761904761904656, 0.7142857142857143016, 0.7380952380952381375, 0.7619047619047618625, 0.7857142857142856984, 0.8095238095238095344, 0.8333333333333333703, 0.8571428571428570953, 0.8809523809523809312, 0.9047619047619047672, 0.9285714285714286031, 0.9523809523809523281, 0.9761904761904761640, 1.000000000000000000 ),
 .UNSPECIFIED. ) 
 GEOMETRIC_REPRESENTATION_ITEM ( )  RATIONAL_B_SPLINE_SURFACE ( (
 ( 1.000000000000000000, 0.8660254037844387076, 1.000000000000000000, 0.8660254037844387076, 1.000000000000000000, 0.8660254037844387076, 1.000000000000000000, 0.8660254037844387076, 1.000000000000000000, 0.8660254037844387076, 1.000000000000000000, 0.8660254037844387076, 1.000000000000000000, 0.8660254037844387076, 1.000000000000000000, 0.8660254037844387076, 1.000000000000000000, 0.8660254037844387076, 1.000000000000000000, 0.8660254037844387076, 1.000000000000000000, 0.8660254037844387076, 1.000000000000000000, 0.8660254037844387076, 1.000000000000000000, 0.8660254037844387076, 1.000000000000000000, 0.8660254037844387076, 1.000000000000000000, 0.8660254037844387076, 1.000000000000000000, 0.8660254037844387076, 1.000000000000000000, 0.8660254037844387076, 1.000000000000000000, 0.8660254037844387076, 1.000000000000000000, 0.8660254037844387076, 1.000000000000000000, 0.8660254037844387076, 1.000000000000000000, 0.8660254037844387076, 1.000000000000000000, 0.8660254037844387076, 1.000000000000000000, 0.8660254037844387076, 1.000000000000000000, 0.8660254037844387076, 1.000000000000000000, 0.8660254037844387076, 1.000000000000000000, 0.8660254037844387076, 1.000000000000000000, 0.8660254037844387076, 1.000000000000000000, 0.8660254037844387076, 1.000000000000000000, 0.8660254037844387076, 1.000000000000000000, 0.8660254037844387076, 1.000000000000000000, 0.8660254037844387076, 1.000000000000000000, 0.8660254037844387076, 1.000000000000000000, 0.8660254037844387076, 1.000000000000000000, 0.8660254037844387076, 1.000000000000000000, 0.8660254037844387076, 1.000000000000000000, 0.8660254037844387076, 1.000000000000000000, 0.8660254037844387076, 1.000000000000000000, 0.8660254037844387076, 1.000000000000000000, 0.8660254037844387076, 1.000000000000000000, 0.8660254037844387076, 1.000000000000000000, 0.8660254037844387076, 1.000000000000000000, 0.8660254037844387076, 1.000000000000000000),
 ( 1.000000000000000000, 0.8660254037844387076, 1.000000000000000000, 0.8660254037844387076, 1.000000000000000000, 0.8660254037844387076, 1.000000000000000000, 0.8660254037844387076, 1.000000000000000000, 0.8660254037844387076, 1.000000000000000000, 0.8660254037844387076, 1.000000000000000000, 0.8660254037844387076, 1.000000000000000000, 0.8660254037844387076, 1.000000000000000000, 0.8660254037844387076, 1.000000000000000000, 0.8660254037844387076, 1.000000000000000000, 0.8660254037844387076, 1.000000000000000000, 0.8660254037844387076, 1.000000000000000000, 0.8660254037844387076, 1.000000000000000000, 0.8660254037844387076, 1.000000000000000000, 0.8660254037844387076, 1.000000000000000000, 0.8660254037844387076, 1.000000000000000000, 0.8660254037844387076, 1.000000000000000000, 0.8660254037844387076, 1.000000000000000000, 0.8660254037844387076, 1.000000000000000000, 0.8660254037844387076, 1.000000000000000000, 0.8660254037844387076, 1.000000000000000000, 0.8660254037844387076, 1.000000000000000000, 0.8660254037844387076, 1.000000000000000000, 0.8660254037844387076, 1.000000000000000000, 0.8660254037844387076, 1.000000000000000000, 0.8660254037844387076, 1.000000000000000000, 0.8660254037844387076, 1.000000000000000000, 0.8660254037844387076, 1.000000000000000000, 0.8660254037844387076, 1.000000000000000000, 0.8660254037844387076, 1.000000000000000000, 0.8660254037844387076, 1.000000000000000000, 0.8660254037844387076, 1.000000000000000000, 0.8660254037844387076, 1.000000000000000000, 0.8660254037844387076, 1.000000000000000000, 0.8660254037844387076, 1.000000000000000000, 0.8660254037844387076, 1.000000000000000000, 0.8660254037844387076, 1.000000000000000000, 0.8660254037844387076, 1.000000000000000000, 0.8660254037844387076, 1.000000000000000000, 0.8660254037844387076, 1.000000000000000000, 0.8660254037844387076, 1.000000000000000000, 0.8660254037844387076, 1.000000000000000000) ) ) 
 REPRESENTATION_ITEM ( '' )  SURFACE ( )  );
#76182 = CARTESIAN_POINT ( 'NONE',  ( 10.19999999999991225, 2.500000000000000000, 4.083716857408420609 ) ) ;
#76183 = DIRECTION ( 'NONE',  ( 0.000000000000000000, 0.000000000000000000, 1.000000000000000000 ) ) ;
#76184 = CIRCLE ( 'NONE', #92918, 0.1000000000000000472 ) ;
#76185 = FACE_OUTER_BOUND ( 'NONE', #15633, .T. ) ;
#76186 = VERTEX_POINT ( 'NONE', #104896 ) ;
#76187 = EDGE_LOOP ( 'NONE', ( #97016, #27765 ) ) ;
#76188 = ORIENTED_EDGE ( 'NONE', *, *, #13944, .F. ) ;
#76189 = ORIENTED_EDGE ( 'NONE', *, *, #89742, .F. ) ;
#76190 = CARTESIAN_POINT ( 'NONE',  ( 6.049999999999934097, 2.500000000000000000, -2.611473670974877592 ) ) ;
#76191 = EDGE_LOOP ( 'NONE', ( #109774, #119030 ) ) ;
#76192 = EDGE_CURVE ( 'NONE', #56136, #52780, #87793, .T. ) ;
#76193 = CARTESIAN_POINT ( 'NONE',  ( 10.59999999999990905, 12.50000000000000000, -4.676537180435978769 ) ) ;
#76194 = EDGE_CURVE ( 'NONE', #85461, #116268, #73145, .T. ) ;
#76195 = ORIENTED_EDGE ( 'NONE', *, *, #23880, .F. ) ;
#76196 = ORIENTED_EDGE ( 'NONE', *, *, #5205, .T. ) ;
#76197 = ADVANCED_FACE ( 'NONE', ( #36187 ), #83618, .T. ) ;
#76198 = CARTESIAN_POINT ( 'NONE',  ( -10.65000000000000213, 12.50000000000000000, 2.576566944158910744 ) ) ;
#76199 = AXIS2_PLACEMENT_3D ( 'NONE', #27219, #65193, #115588 ) ;
#76200 = AXIS2_PLACEMENT_3D ( 'NONE', #126861, #26085, #116374 ) ;
#76201 = DIRECTION ( 'NONE',  ( -0.000000000000000000, -1.000000000000000000, -0.000000000000000000 ) ) ;
#76202 = CARTESIAN_POINT ( 'NONE',  ( 3.549999999999942979, 2.500000000000000000, 1.918653347947321564 ) ) ;
#76203 = CARTESIAN_POINT ( 'NONE',  ( 5.399999999999932854, 12.50000000000000000, 3.702399969078682407 ) ) ;
#76204 = EDGE_CURVE ( 'NONE', #18883, #59390, #64816, .T. ) ;
#76205 = DIRECTION ( 'NONE',  ( 0.000000000000000000, -0.000000000000000000, 1.000000000000000000 ) ) ;
#76206 = EDGE_CURVE ( 'NONE', #10596, #15192, #117027, .T. ) ;
#76207 = ORIENTED_EDGE ( 'NONE', *, *, #18954, .T. ) ;
#76208 = ADVANCED_FACE ( 'NONE', ( #86555 ), #17809, .T. ) ;
#76209 = EDGE_CURVE ( 'NONE', #105930, #123334, #15214, .T. ) ;
#76210 = ORIENTED_EDGE ( 'NONE', *, *, #88142, .F. ) ;
#76211 = CIRCLE ( 'NONE', #80321, 0.06509327318403745899 ) ;
#76212 = EDGE_CURVE ( 'NONE', #7922, #108419, #48104, .T. ) ;
#76213 = ORIENTED_EDGE ( 'NONE', *, *, #14245, .T. ) ;
#76214 = ORIENTED_EDGE ( 'NONE', *, *, #67889, .F. ) ;
#76215 = CIRCLE ( 'NONE', #120123, 0.06509327318403745899 ) ;
#76216 = CARTESIAN_POINT ( 'NONE',  ( 13.09999999999990195, 2.500000000000000000, -4.776537180435978414 ) ) ;
#76217 = EDGE_LOOP ( 'NONE', ( #43958, #35643 ) ) ;
#76218 = EDGE_LOOP ( 'NONE', ( #3073, #62594, #120415, #78804 ) ) ;
#76219 = EDGE_CURVE ( 'NONE', #96705, #38043, #33450, .T. ) ;
#76220 = DIRECTION ( 'NONE',  ( 0.000000000000000000, 0.000000000000000000, 1.000000000000000000 ) ) ;
#76222 = VECTOR ( 'NONE', #70662, 1000.000000000000000 ) ;
#76221 = CARTESIAN_POINT ( 'NONE',  ( 11.24999999999990941, 2.500000000000000000, -1.572243186433550211 ) ) ;
#76223 = DIRECTION ( 'NONE',  ( 0.000000000000000000, 0.000000000000000000, 1.000000000000000000 ) ) ;
#76224 = CIRCLE ( 'NONE', #107512, 0.06509327318403745899 ) ;
#76225 = LINE ( 'NONE', #45484, #44198 ) ;
#76226 = DIRECTION ( 'NONE',  ( -4.274815082592931898E-19, -0.9999939076577903929, -0.003490651415223739937 ) ) ;
#76228 = AXIS2_PLACEMENT_3D ( 'NONE', #64881, #84537, #124469 ) ;
#76227 = CARTESIAN_POINT ( 'NONE',  ( -2.100000000000033840, 12.50000000000000000, 5.022947341949748790 ) ) ;
#76229 = ORIENTED_EDGE ( 'NONE', *, *, #2864, .T. ) ;
#76230 = CIRCLE ( 'NONE', #19790, 0.1000000000000002554 ) ;
#76231 = CARTESIAN_POINT ( 'NONE',  ( 187.5000000000000000, 0.000000000000000000, 7.700000000000000178 ) ) ;
#76232 = ORIENTED_EDGE ( 'NONE', *, *, #106890, .T. ) ;
#76233 = DIRECTION ( 'NONE',  ( 0.000000000000000000, 1.000000000000000000, 0.000000000000000000 ) ) ;
#76234 = ORIENTED_EDGE ( 'NONE', *, *, #96889, .T. ) ;
#76235 = FACE_OUTER_BOUND ( 'NONE', #65954, .T. ) ;
#76236 = DIRECTION ( 'NONE',  ( -0.000000000000000000, 1.000000000000000000, -0.000000000000000000 ) ) ;
#76237 = EDGE_LOOP ( 'NONE', ( #11305, #97922, #31907, #472 ) ) ;
#76238 = CARTESIAN_POINT ( 'NONE',  ( 3.749999999999940492, 12.50000000000000000, 5.737276932171707422 ) ) ;
#76239 = LINE ( 'NONE', #106336, #85647 ) ;
#76240 = ORIENTED_EDGE ( 'NONE', *, *, #14547, .T. ) ;
#76241 = AXIS2_PLACEMENT_3D ( 'NONE', #1210, #9746, #11672 ) ;
#76243 = DIRECTION ( 'NONE',  ( 0.000000000000000000, 0.000000000000000000, -1.000000000000000000 ) ) ;
#76242 = CONICAL_SURFACE ( 'NONE', #11482, 0.09999999999999982514, 0.003490658503988666988 ) ;
#76244 = VERTEX_POINT ( 'NONE', #107495 ) ;
#76245 = CONICAL_SURFACE ( 'NONE', #49068, 0.1000000000000002554, 0.003490658503988666988 ) ;
#76246 = VECTOR ( 'NONE', #55420, 1000.000000000000000 ) ;
#76247 = EDGE_LOOP ( 'NONE', ( #126020, #116760, #48057, #31539 ) ) ;
#76248 = DIRECTION ( 'NONE',  ( 0.000000000000000000, 0.000000000000000000, 1.000000000000000000 ) ) ;
#76249 = DIRECTION ( 'NONE',  ( -4.274815082592931898E-19, -0.9999939076577903929, -0.003490651415223739937 ) ) ;
#76250 = CARTESIAN_POINT ( 'NONE',  ( 187.2552083336747444, 6.551208109652275624, -3.782341765624998686 ) ) ;
#76251 = LINE ( 'NONE', #36970, #13616 ) ;
#76252 = VECTOR ( 'NONE', #4380, 1000.000000000000000 ) ;
#76254 = EDGE_CURVE ( 'NONE', #28910, #24882, #94072, .T. ) ;
#76253 = CARTESIAN_POINT ( 'NONE',  ( -10.80000000000000071, 2.500000000000000000, 4.430127018922196847 ) ) ;
#76255 = AXIS2_PLACEMENT_3D ( 'NONE', #62190, #32736, #92263 ) ;
#76256 = CONICAL_SURFACE ( 'NONE', #84651, 0.09999999999999982514, 0.003490658503988666988 ) ;
#76257 = DIRECTION ( 'NONE',  ( 0.000000000000000000, 1.000000000000000000, 0.000000000000000000 ) ) ;
#76258 = VECTOR ( 'NONE', #96844, 1000.000000000000000 ) ;
#76259 = ORIENTED_EDGE ( 'NONE', *, *, #51792, .T. ) ;
#76260 = VECTOR ( 'NONE', #112305, 1000.000000000000000 ) ;
#76261 = CARTESIAN_POINT ( 'NONE',  ( -9.200000000000006395, 2.500000000000000000, 0.09999999999999761857 ) ) ;
#76262 = ORIENTED_EDGE ( 'NONE', *, *, #97036, .F. ) ;
#76263 = AXIS2_PLACEMENT_3D ( 'NONE', #40360, #10851, #101202 ) ;
#76264 = DIRECTION ( 'NONE',  ( 0.000000000000000000, 0.000000000000000000, 1.000000000000000000 ) ) ;
#76265 = CARTESIAN_POINT ( 'NONE',  ( -15.19999999999998153, 12.50000000000000000, -0.3464101615137759604 ) ) ;
#76266 = DIRECTION ( 'NONE',  ( -4.274815082592931898E-19, -0.9999939076577903929, -0.003490651415223739937 ) ) ;
#76267 = ORIENTED_EDGE ( 'NONE', *, *, #112797, .F. ) ;
#76268 = CARTESIAN_POINT ( 'NONE',  ( 14.14999999999989200, 2.500000000000000000, -2.165063509461101710 ) ) ;
#76269 = DIRECTION ( 'NONE',  ( 0.000000000000000000, 0.000000000000000000, 1.000000000000000000 ) ) ;
#76270 = AXIS2_PLACEMENT_3D ( 'NONE', #38849, #20471, #120596 ) ;
#76271 = EDGE_LOOP ( 'NONE', ( #21539, #31042, #49374, #67532 ) ) ;
#76272 = DIRECTION ( 'NONE',  ( -0.000000000000000000, -1.000000000000000000, -0.000000000000000000 ) ) ;
#76273 = EDGE_LOOP ( 'NONE', ( #71256, #39136, #124907, #27990 ) ) ;
#76274 = EDGE_LOOP ( 'NONE', ( #53639, #22618 ) ) ;
#76275 = FACE_OUTER_BOUND ( 'NONE', #15410, .T. ) ;
#76276 = VERTEX_POINT ( 'NONE', #87192 ) ;
#76277 = DIRECTION ( 'NONE',  ( -0.000000000000000000, 1.000000000000000000, -0.000000000000000000 ) ) ;
#76278 = DIRECTION ( 'NONE',  ( 0.000000000000000000, 0.000000000000000000, -1.000000000000000000 ) ) ;
#76279 = AXIS2_PLACEMENT_3D ( 'NONE', #25134, #4836, #123974 ) ;
#76280 = DIRECTION ( 'NONE',  ( 0.000000000000000000, 0.000000000000000000, 1.000000000000000000 ) ) ;
#76281 = AXIS2_PLACEMENT_3D ( 'NONE', #11582, #32542, #63261 ) ;
#76282 = ORIENTED_EDGE ( 'NONE', *, *, #49578, .T. ) ;
#76283 = ADVANCED_FACE ( 'NONE', ( #87834 ), #55814, .T. ) ;
#76284 = FACE_BOUND ( 'NONE', #71033, .T. ) ;
#76286 = EDGE_LOOP ( 'NONE', ( #4658, #94828 ) ) ;
#76285 = DIRECTION ( 'NONE',  ( 0.000000000000000000, 0.000000000000000000, -1.000000000000000000 ) ) ;
#76287 = DIRECTION ( 'NONE',  ( 0.000000000000000000, 0.000000000000000000, 1.000000000000000000 ) ) ;
#76288 = CARTESIAN_POINT ( 'NONE',  ( -9.999999999999969802, 12.50000000000000000, -2.276824562219559311E-15 ) ) ;
#76289 = EDGE_CURVE ( 'NONE', #61621, #56423, #27166, .T. ) ;
#76290 = ORIENTED_EDGE ( 'NONE', *, *, #75410, .T. ) ;
#76291 = ORIENTED_EDGE ( 'NONE', *, *, #85880, .F. ) ;
#76292 = CIRCLE ( 'NONE', #78464, 0.1000000000000002554 ) ;
#76293 = VERTEX_POINT ( 'NONE', #55174 ) ;
#76294 = DIRECTION ( 'NONE',  ( 0.000000000000000000, 1.000000000000000000, 0.000000000000000000 ) ) ;
#76295 = DIRECTION ( 'NONE',  ( -0.000000000000000000, -1.000000000000000000, -0.000000000000000000 ) ) ;
#76296 = EDGE_CURVE ( 'NONE', #109309, #77648, #25106, .T. ) ;
#76297 = ADVANCED_FACE ( 'NONE', ( #116015 ), #27620, .T. ) ;
#76298 = CARTESIAN_POINT ( 'NONE',  ( -11.25000000000000000, 2.500000000000000000, 7.188010851410848723 ) ) ;
#76299 = EDGE_CURVE ( 'NONE', #58714, #34192, #56445, .T. ) ;
#76300 = FACE_BOUND ( 'NONE', #104139, .T. ) ;
#76302 = EDGE_CURVE ( 'NONE', #121670, #57274, #75280, .T. ) ;
#76301 = EDGE_LOOP ( 'NONE', ( #15415, #114626, #35809, #112462 ) ) ;
#76303 = CARTESIAN_POINT ( 'NONE',  ( 185.9010416670080303, -4.367472073101519747, 7.564683531249999149 ) ) ;
#76304 = ADVANCED_FACE ( 'NONE', ( #119240 ), #112856, .T. ) ;
#76305 = DIRECTION ( 'NONE',  ( 0.000000000000000000, 1.000000000000000000, 0.000000000000000000 ) ) ;
#76306 = CARTESIAN_POINT ( 'NONE',  ( 9.799999999999918998, 2.500000000000000000, -0.4464101615137782142 ) ) ;
#76308 = CARTESIAN_POINT ( 'NONE',  ( -3.150000000000030109, 2.500000000000000000, 1.918653347947321564 ) ) ;
#76307 = CIRCLE ( 'NONE', #111905, 0.06509327318403745899 ) ;
#76309 = CIRCLE ( 'NONE', #126489, 0.1000000000000002554 ) ;
#76310 = FACE_OUTER_BOUND ( 'NONE', #12978, .T. ) ;
#76311 = CARTESIAN_POINT ( 'NONE',  ( 7.099999999999926814, 2.500000000000000000, -2.276824562219559311E-15 ) ) ;
#76312 = EDGE_CURVE ( 'NONE', #103846, #87255, #105, .T. ) ;
#76313 = CARTESIAN_POINT ( 'NONE',  ( -8.150000000000012790, 2.500000000000000000, -2.411473670974877859 ) ) ;
#76314 = DIRECTION ( 'NONE',  ( -0.000000000000000000, 1.000000000000000000, -0.000000000000000000 ) ) ;
#76315 = EDGE_CURVE ( 'NONE', #57789, #31107, #119113, .T. ) ;
#76316 = CARTESIAN_POINT ( 'NONE',  ( 14.14999999999989377, 2.500000000000000000, -1.472243186433550122 ) ) ;
#76317 = ORIENTED_EDGE ( 'NONE', *, *, #97136, .T. ) ;
#76318 = EDGE_LOOP ( 'NONE', ( #76920, #27045 ) ) ;
#76319 = ORIENTED_EDGE ( 'NONE', *, *, #10800, .F. ) ;
#76320 = VERTEX_POINT ( 'NONE', #19764 ) ;
#76321 = ORIENTED_EDGE ( 'NONE', *, *, #85629, .T. ) ;
#76322 = PLANE ( 'NONE',  #6621 ) ;
#76323 = CARTESIAN_POINT ( 'NONE',  ( 4.349999999999941025, 2.500000000000000000, -1.918653347947326004 ) ) ;
#76324 = VERTEX_POINT ( 'NONE', #69487 ) ;
#76325 = FACE_BOUND ( 'NONE', #22613, .T. ) ;
#76326 = CIRCLE ( 'NONE', #109871, 0.06509327318403745899 ) ;
#76327 = CARTESIAN_POINT ( 'NONE',  ( -8.100000000000013856, 2.500000000000000000, -3.983716857408426293 ) ) ;
#76328 = AXIS2_PLACEMENT_3D ( 'NONE', #50110, #61200, #89997 ) ;
#76329 = DIRECTION ( 'NONE',  ( -0.000000000000000000, 1.000000000000000000, -0.000000000000000000 ) ) ;
#76330 = AXIS2_PLACEMENT_3D ( 'NONE', #110219, #127288, #87332 ) ;
#76331 = AXIS2_PLACEMENT_3D ( 'NONE', #52517, #92442, #2774 ) ;
#76332 = CARTESIAN_POINT ( 'NONE',  ( -13.34999999999999076, 2.500000000000000000, 2.857883832488652853 ) ) ;
#76333 = DIRECTION ( 'NONE',  ( -0.000000000000000000, -1.000000000000000000, -0.000000000000000000 ) ) ;
#76334 = DIRECTION ( 'NONE',  ( 0.000000000000000000, 0.000000000000000000, 1.000000000000000000 ) ) ;
#76335 = EDGE_LOOP ( 'NONE', ( #110949, #41377, #77410, #11400 ) ) ;
#76336 = CARTESIAN_POINT ( 'NONE',  ( 162.5000000000000000, -0.5000000000000000000, -7.500000000000005329 ) ) ;
#76337 = AXIS2_PLACEMENT_3D ( 'NONE', #56078, #126772, #37108 ) ;
#76338 = EDGE_LOOP ( 'NONE', ( #116866, #47431 ) ) ;
#76339 = CIRCLE ( 'NONE', #24106, 1.000000000000000000 ) ;
#76340 = AXIS2_PLACEMENT_3D ( 'NONE', #111472, #51296, #883 ) ;
#76341 = ORIENTED_EDGE ( 'NONE', *, *, #18242, .T. ) ;
#76342 = ORIENTED_EDGE ( 'NONE', *, *, #67132, .T. ) ;
#76343 = CARTESIAN_POINT ( 'NONE',  ( 5.599999999999934808, 2.500000000000000000, -3.983716857408426293 ) ) ;
#76344 = AXIS2_PLACEMENT_3D ( 'NONE', #37151, #78368, #37785 ) ;
#76345 = DIRECTION ( 'NONE',  ( 0.000000000000000000, 0.000000000000000000, -1.000000000000000000 ) ) ;
#76346 = DIRECTION ( 'NONE',  ( 0.000000000000000000, -0.9999939076577903929, 0.003490651415223739937 ) ) ;
#76347 = ORIENTED_EDGE ( 'NONE', *, *, #56068, .T. ) ;
#76348 = CARTESIAN_POINT ( 'NONE',  ( 15.83209681635555022, 2.499999999999999556, -5.404881881984137770 ) ) ;
#76349 = EDGE_CURVE ( 'NONE', #10759, #28226, #68851, .T. ) ;
#76350 = CONICAL_SURFACE ( 'NONE', #47115, 0.1000000000000000056, 0.003490658503988666988 ) ;
#76351 = AXIS2_PLACEMENT_3D ( 'NONE', #33672, #63784, #21930 ) ;
#76352 = LINE ( 'NONE', #78297, #103430 ) ;
#76353 = ADVANCED_FACE ( 'NONE', ( #100880 ), #129096, .T. ) ;
#76354 = DIRECTION ( 'NONE',  ( 0.000000000000000000, 0.000000000000000000, 1.000000000000000000 ) ) ;
#76355 = CARTESIAN_POINT ( 'NONE',  ( 184.5729166673494603, 4.445597072760120838, -7.699999999999998401 ) ) ;
#76357 = AXIS2_PLACEMENT_3D ( 'NONE', #2325, #24405, #42282 ) ;
#76356 = DIRECTION ( 'NONE',  ( -0.000000000000000000, 1.000000000000000000, -0.000000000000000000 ) ) ;
#76358 = CARTESIAN_POINT ( 'NONE',  ( 12.29999999999990656, 12.50000000000000000, 3.983716857408420964 ) ) ;
#76359 = EDGE_CURVE ( 'NONE', #56076, #126920, #18845, .T. ) ;
#76360 = EDGE_LOOP ( 'NONE', ( #75749, #48760, #64707, #14837 ) ) ;
#76361 = CARTESIAN_POINT ( 'NONE',  ( 1.649999999999951505, 2.500000000000000000, 2.857883832488649301 ) ) ;
#76362 = EDGE_CURVE ( 'NONE', #12477, #79083, #79419, .T. ) ;
#76363 = VERTEX_POINT ( 'NONE', #109425 ) ;
#76364 = ADVANCED_FACE ( 'NONE', ( #91071 ), #22976, .T. ) ;
#76365 = ORIENTED_EDGE ( 'NONE', *, *, #126441, .T. ) ;
#76366 = DIRECTION ( 'NONE',  ( 0.000000000000000000, 1.846105847067148022E-16, -1.000000000000000000 ) ) ;
#76367 = DIRECTION ( 'NONE',  ( 0.000000000000000000, 1.000000000000000000, 0.000000000000000000 ) ) ;
#76368 = PLANE ( 'NONE',  #23763 ) ;
#76369 = CIRCLE ( 'NONE', #47129, 0.1000000000000002554 ) ;
#76370 = EDGE_LOOP ( 'NONE', ( #97623, #106783 ) ) ;
#76371 = EDGE_CURVE ( 'NONE', #44219, #47269, #119888, .T. ) ;
#76372 = EDGE_LOOP ( 'NONE', ( #17024, #8261, #32594, #8657 ) ) ;
#76373 = DIRECTION ( 'NONE',  ( 0.000000000000000000, 1.000000000000000000, 0.000000000000000000 ) ) ;
#76374 = CARTESIAN_POINT ( 'NONE',  ( -7.500000000000015099, 2.500000000000000000, -5.122947341949753763 ) ) ;
#76375 = DIRECTION ( 'NONE',  ( 0.000000000000000000, 0.000000000000000000, 1.000000000000000000 ) ) ;
#76376 = ORIENTED_EDGE ( 'NONE', *, *, #118878, .T. ) ;
#76377 = VERTEX_POINT ( 'NONE', #49238 ) ;
#76378 = DIRECTION ( 'NONE',  ( 0.000000000000000000, 1.000000000000000000, 0.000000000000000000 ) ) ;
#76379 = AXIS2_PLACEMENT_3D ( 'NONE', #54428, #74079, #36094 ) ;
#76380 = CIRCLE ( 'NONE', #53395, 0.09999999999999982514 ) ;
#76381 = ORIENTED_EDGE ( 'NONE', *, *, #62462, .T. ) ;
#76383 = CIRCLE ( 'NONE', #40897, 0.06509327318403745899 ) ;
#76382 = DIRECTION ( 'NONE',  ( -0.000000000000000000, 1.000000000000000000, -0.000000000000000000 ) ) ;
#76384 = CARTESIAN_POINT ( 'NONE',  ( -11.04999999999999893, 2.500000000000000000, 1.718653347947321386 ) ) ;
#76385 = ORIENTED_EDGE ( 'NONE', *, *, #124751, .T. ) ;
#76386 = DIRECTION ( 'NONE',  ( 0.000000000000000000, 0.000000000000000000, -1.000000000000000000 ) ) ;
#76387 = DIRECTION ( 'NONE',  ( 1.000000000000000000, -0.000000000000000000, -0.000000000000000000 ) ) ;
#76388 = CARTESIAN_POINT ( 'NONE',  ( -0.6000000000000323963, 2.500000000000000000, -0.2464101615137759549 ) ) ;
#76389 = EDGE_CURVE ( 'NONE', #64274, #40995, #54356, .T. ) ;
#76390 = DIRECTION ( 'NONE',  ( -0.000000000000000000, 1.000000000000000000, -0.000000000000000000 ) ) ;
#76391 = ORIENTED_EDGE ( 'NONE', *, *, #119909, .T. ) ;
#76392 = CIRCLE ( 'NONE', #3233, 0.1000000000000002554 ) ;
#76393 = DIRECTION ( 'NONE',  ( 0.000000000000000000, 0.000000000000000000, -1.000000000000000000 ) ) ;
#76395 = VECTOR ( 'NONE', #27363, 1000.000000000000000 ) ;
#76394 = DIRECTION ( 'NONE',  ( 0.000000000000000000, 0.000000000000000000, 1.000000000000000000 ) ) ;
#76396 = ORIENTED_EDGE ( 'NONE', *, *, #49037, .T. ) ;
#76397 = ORIENTED_EDGE ( 'NONE', *, *, #54705, .T. ) ;
#76398 = CARTESIAN_POINT ( 'NONE',  ( 185.1302083336747160, -4.367472073101514418, -7.564683531250002702 ) ) ;
#76399 = DIRECTION ( 'NONE',  ( -0.000000000000000000, -1.000000000000000000, -0.000000000000000000 ) ) ;
#76400 = DIRECTION ( 'NONE',  ( 0.000000000000000000, -0.000000000000000000, 1.000000000000000000 ) ) ;
#76401 = CYLINDRICAL_SURFACE ( 'NONE', #62651, 2.749999999999997335 ) ;
#76402 = DIRECTION ( 'NONE',  ( 0.000000000000000000, 0.000000000000000000, 1.000000000000000000 ) ) ;
#76403 = DIRECTION ( 'NONE',  ( 0.000000000000000000, 1.000000000000000000, 0.000000000000000000 ) ) ;
#76404 = AXIS2_PLACEMENT_3D ( 'NONE', #95302, #5605, #125404 ) ;
#76405 = AXIS2_PLACEMENT_3D ( 'NONE', #53959, #44133, #115418 ) ;
#76407 = ADVANCED_FACE ( 'NONE', ( #99616 ), #48191, .T. ) ;
#76406 = CARTESIAN_POINT ( 'NONE',  ( 17.46754056294894752, 1.506946016794848742, -5.249106941592859066 ) ) ;
#76408 = DIRECTION ( 'NONE',  ( 0.000000000000000000, 1.000000000000000000, 0.000000000000000000 ) ) ;
#76409 = CARTESIAN_POINT ( 'NONE',  ( 11.64999999999990798, 2.500000000000000000, -2.757883832488654097 ) ) ;
#76410 = DIRECTION ( 'NONE',  ( 0.000000000000000000, -0.9999939076577903929, 0.003490651415223739937 ) ) ;
#76411 = EDGE_LOOP ( 'NONE', ( #22686, #30975 ) ) ;
#76413 = ORIENTED_EDGE ( 'NONE', *, *, #45277, .F. ) ;
#76412 = AXIS2_PLACEMENT_3D ( 'NONE', #29359, #99383, #19514 ) ;
#76414 = DIRECTION ( 'NONE',  ( 0.000000000000000000, -0.000000000000000000, 1.000000000000000000 ) ) ;
#76415 = EDGE_LOOP ( 'NONE', ( #112722, #94634 ) ) ;
#76416 = EDGE_CURVE ( 'NONE', #56250, #112093, #87877, .T. ) ;
#76417 = LINE ( 'NONE', #105224, #87535 ) ;
#76418 = CONICAL_SURFACE ( 'NONE', #1195, 0.09999999999999982514, 0.003490658503988666988 ) ;
#76419 = CARTESIAN_POINT ( 'NONE',  ( -14.34999999999998543, 2.500000000000000000, 1.818653347947325472 ) ) ;
#76420 = DIRECTION ( 'NONE',  ( -0.000000000000000000, -1.000000000000000000, -0.000000000000000000 ) ) ;
#76421 = ORIENTED_EDGE ( 'NONE', *, *, #14659, .T. ) ;
#76422 = DIRECTION ( 'NONE',  ( 0.000000000000000000, 0.000000000000000000, 1.000000000000000000 ) ) ;
#76423 = CIRCLE ( 'NONE', #5397, 0.1000000000000002554 ) ;
#76424 = PLANE ( 'NONE',  #9447 ) ;
#76426 = ORIENTED_EDGE ( 'NONE', *, *, #64153, .F. ) ;
#76425 = PLANE ( 'NONE',  #27174 ) ;
#76427 = CARTESIAN_POINT ( 'NONE',  ( -10.20000000000000284, 2.500000000000000000, 4.083716857408421497 ) ) ;
#76428 = EDGE_LOOP ( 'NONE', ( #63671, #37105 ) ) ;
#76429 = EDGE_LOOP ( 'NONE', ( #75486, #34905 ) ) ;
#76430 = VERTEX_POINT ( 'NONE', #60343 ) ;
#76431 = VERTEX_POINT ( 'NONE', #128446 ) ;
#76432 = DIRECTION ( 'NONE',  ( -1.000000000000000000, 0.000000000000000000, 0.000000000000000000 ) ) ;
#76433 = AXIS2_PLACEMENT_3D ( 'NONE', #44212, #22668, #112962 ) ;
#76434 = DIRECTION ( 'NONE',  ( 0.000000000000000000, 0.000000000000000000, -1.000000000000000000 ) ) ;
#76435 = DIRECTION ( 'NONE',  ( -0.000000000000000000, -1.000000000000000000, -0.000000000000000000 ) ) ;
#76436 = CARTESIAN_POINT ( 'NONE',  ( -13.94999999999998685, 12.50000000000000000, 1.883746621131362931 ) ) ;
#76437 = AXIS2_PLACEMENT_3D ( 'NONE', #60422, #19838, #50567 ) ;
#76438 = EDGE_LOOP ( 'NONE', ( #118272, #57324 ) ) ;
#76440 = EDGE_CURVE ( 'NONE', #7017, #29011, #110870, .T. ) ;
#76439 = CIRCLE ( 'NONE', #5315, 0.06509327318403745899 ) ;
#76442 = AXIS2_PLACEMENT_3D ( 'NONE', #124392, #73335, #24893 ) ;
#76441 = FACE_OUTER_BOUND ( 'NONE', #14335, .T. ) ;
#76443 = ORIENTED_EDGE ( 'NONE', *, *, #66827, .T. ) ;
#76444 = CARTESIAN_POINT ( 'NONE',  ( 34.93074629423288258, -2.900242961789775809, -4.640733549233234001 ) ) ;
#76445 = CARTESIAN_POINT ( 'NONE',  ( -5.850000000000021849, 2.500000000000000000, -1.472243186433550122 ) ) ;
#76446 = CARTESIAN_POINT ( 'NONE',  ( -3.950000000000026379, 2.500000000000000000, 2.511473670974873507 ) ) ;
#76447 = CARTESIAN_POINT ( 'NONE',  ( 17.88933034088942975, -0.4802206367769106254, 4.999988745079923191 ) ) ;
#76448 = EDGE_CURVE ( 'NONE', #55993, #90336, #62785, .T. ) ;
#76449 = ORIENTED_EDGE ( 'NONE', *, *, #11879, .F. ) ;
#76450 = VERTEX_POINT ( 'NONE', #70154 ) ;
#76451 = ORIENTED_EDGE ( 'NONE', *, *, #112665, .T. ) ;
#76452 = CARTESIAN_POINT ( 'NONE',  ( 10.19999999999991047, 2.500000000000000000, -3.883716857408426648 ) ) ;
#76453 = DIRECTION ( 'NONE',  ( 0.000000000000000000, 1.000000000000000000, 0.000000000000000000 ) ) ;
#76454 = EDGE_CURVE ( 'NONE', #114720, #55263, #35681, .T. ) ;
#76455 = ADVANCED_FACE ( 'NONE', ( #60961 ), #78697, .T. ) ;
#76456 = CARTESIAN_POINT ( 'NONE',  ( -6.250000000000015987, 12.50000000000000000, 1.407149913249508000 ) ) ;
#76457 = EDGE_CURVE ( 'NONE', #108866, #6668, #9292, .T. ) ;
#76458 = FACE_BOUND ( 'NONE', #41573, .T. ) ;
#76459 = EDGE_CURVE ( 'NONE', #58766, #17273, #22352, .T. ) ;
#76460 = DIRECTION ( 'NONE',  ( 0.000000000000000000, 1.000000000000000000, 0.000000000000000000 ) ) ;
#76461 = CIRCLE ( 'NONE', #63849, 0.06509327318403745899 ) ;
#76462 = DIRECTION ( 'NONE',  ( -0.000000000000000000, -1.000000000000000000, -0.000000000000000000 ) ) ;
#76463 = DIRECTION ( 'NONE',  ( 0.000000000000000000, 1.000000000000000000, 0.000000000000000000 ) ) ;
#76464 = DIRECTION ( 'NONE',  ( 0.000000000000000000, 0.000000000000000000, 1.000000000000000000 ) ) ;
#76465 = EDGE_CURVE ( 'NONE', #118978, #12752, #51805, .T. ) ;
#76466 = EDGE_CURVE ( 'NONE', #66361, #74337, #13134, .T. ) ;
#76467 = CARTESIAN_POINT ( 'NONE',  ( 184.6718750003414016, 9.264065473108010111E-16, -7.564683531250000925 ) ) ;
#76468 = AXIS2_PLACEMENT_3D ( 'NONE', #79876, #72647, #101454 ) ;
#76469 = CARTESIAN_POINT ( 'NONE',  ( -2.100000000000033396, 2.500000000000000000, -5.122947341949753763 ) ) ;
#76470 = EDGE_CURVE ( 'NONE', #66532, #62883, #31474, .T. ) ;
#76471 = FACE_OUTER_BOUND ( 'NONE', #27694, .T. ) ;
#76472 = CONICAL_SURFACE ( 'NONE', #128818, 0.1000000000000000056, 0.003490658503988666988 ) ;
#76473 = EDGE_CURVE ( 'NONE', #46102, #86677, #96200, .T. ) ;
#76474 = EDGE_CURVE ( 'NONE', #54885, #119497, #20997, .T. ) ;
#76475 = DIRECTION ( 'NONE',  ( 0.000000000000000000, -0.9999939076577903929, 0.003490651415223739937 ) ) ;
#76476 = AXIS2_PLACEMENT_3D ( 'NONE', #37360, #76633, #67415 ) ;
#76477 = VERTEX_POINT ( 'NONE', #73355 ) ;
#76478 = EDGE_LOOP ( 'NONE', ( #123666, #40745 ) ) ;
#76479 = VERTEX_POINT ( 'NONE', #3970 ) ;
#76480 = ORIENTED_EDGE ( 'NONE', *, *, #13295, .F. ) ;
#76481 = CARTESIAN_POINT ( 'NONE',  ( 2.899999999999943956, 2.500000000000000000, 4.330127018922196314 ) ) ;
#76482 = FACE_BOUND ( 'NONE', #124058, .T. ) ;
#76483 = ADVANCED_FACE ( 'NONE', ( #11856 ), #100423, .T. ) ;
#76484 = FACE_OUTER_BOUND ( 'NONE', #46526, .T. ) ;
#76486 = DIRECTION ( 'NONE',  ( 0.000000000000000000, 0.000000000000000000, 1.000000000000000000 ) ) ;
#76485 = CIRCLE ( 'NONE', #51361, 0.1000000000000002554 ) ;
#76488 = AXIS2_PLACEMENT_3D ( 'NONE', #104187, #11931, #63628 ) ;
#76487 = AXIS2_PLACEMENT_3D ( 'NONE', #108708, #118523, #88411 ) ;
#76489 = VERTEX_POINT ( 'NONE', #52431 ) ;
#76490 = FACE_OUTER_BOUND ( 'NONE', #114361, .T. ) ;
#76491 = DIRECTION ( 'NONE',  ( -0.000000000000000000, 1.000000000000000000, -0.000000000000000000 ) ) ;
#76492 = ORIENTED_EDGE ( 'NONE', *, *, #119742, .T. ) ;
#76493 = CARTESIAN_POINT ( 'NONE',  ( 105.5000000000000142, 0.000000000000000000, 0.000000000000000000 ) ) ;
#76494 = DIRECTION ( 'NONE',  ( 0.000000000000000000, 0.000000000000000000, 1.000000000000000000 ) ) ;
#76495 = VECTOR ( 'NONE', #66320, 1000.000000000000000 ) ;
#76496 = CONICAL_SURFACE ( 'NONE', #97410, 0.1000000000000000472, 0.003490658503988666988 ) ;
#76497 = ORIENTED_EDGE ( 'NONE', *, *, #52122, .T. ) ;
#76498 = LINE ( 'NONE', #96756, #111333 ) ;
#76499 = CARTESIAN_POINT ( 'NONE',  ( -12.49999999999999289, 2.500000000000000000, 4.922947341949748257 ) ) ;
#76500 = ORIENTED_EDGE ( 'NONE', *, *, #37788, .F. ) ;
#76501 = CARTESIAN_POINT ( 'NONE',  ( -1.650000000000035216, 2.500000000000000000, -1.472243186433550122 ) ) ;
#76502 = DIRECTION ( 'NONE',  ( 0.000000000000000000, 1.000000000000000000, 0.000000000000000000 ) ) ;
#76503 = VERTEX_POINT ( 'NONE', #32178 ) ;
#76504 = DIRECTION ( 'NONE',  ( 0.000000000000000000, 0.000000000000000000, -1.000000000000000000 ) ) ;
#76505 = EDGE_LOOP ( 'NONE', ( #19554, #5018 ) ) ;
#76506 = ORIENTED_EDGE ( 'NONE', *, *, #84429, .T. ) ;
#76507 = FACE_OUTER_BOUND ( 'NONE', #82488, .T. ) ;
#76508 = VERTEX_POINT ( 'NONE', #94282 ) ;
#76509 = DIRECTION ( 'NONE',  ( 0.000000000000000000, -0.9999939076577903929, 0.003490651415223739937 ) ) ;
#76510 = CARTESIAN_POINT ( 'NONE',  ( 4.999999999999971578, 2.500000000000000000, -2.276824562219559311E-15 ) ) ;
#76511 = EDGE_CURVE ( 'NONE', #11005, #102405, #41351, .T. ) ;
#76512 = AXIS2_PLACEMENT_3D ( 'NONE', #4676, #85196, #26291 ) ;
#76513 = VERTEX_POINT ( 'NONE', #23619 ) ;
#76514 = AXIS2_PLACEMENT_3D ( 'NONE', #47930, #77380, #9282 ) ;
#76516 = EDGE_CURVE ( 'NONE', #55744, #87232, #89949, .T. ) ;
#76515 = CARTESIAN_POINT ( 'NONE',  ( -1.650000000000034772, 2.500000000000000000, 5.702370205355745014 ) ) ;
#76517 = CARTESIAN_POINT ( 'NONE',  ( -4.350000000000023626, 12.50000000000000000, 6.841600689897072485 ) ) ;
#76518 = DIRECTION ( 'NONE',  ( 0.000000000000000000, 0.000000000000000000, 1.000000000000000000 ) ) ;
#76519 = CARTESIAN_POINT ( 'NONE',  ( -5.600000000000023626, 12.50000000000000000, -3.983716857408426293 ) ) ;
#76520 = CARTESIAN_POINT ( 'NONE',  ( 11.89999999999990443, 12.50000000000000000, 0.3464101615137736845 ) ) ;
#76521 = CARTESIAN_POINT ( 'NONE',  ( 7.699999999999923794, 12.50000000000000000, 4.741630453620009789 ) ) ;
#76522 = ADVANCED_FACE ( 'NONE', ( #61627 ), #12503, .F. ) ;
#76524 = VERTEX_POINT ( 'NONE', #3338 ) ;
#76523 = VECTOR ( 'NONE', #31880, 1000.000000000000000 ) ;
#76525 = VERTEX_POINT ( 'NONE', #104118 ) ;
#76526 = CARTESIAN_POINT ( 'NONE',  ( -7.500000000000015099, 2.500000000000000000, -0.6928203230275541413 ) ) ;
#76527 = FACE_OUTER_BOUND ( 'NONE', #117828, .T. ) ;
#76528 = CARTESIAN_POINT ( 'NONE',  ( 5.399999999999934630, 2.500000000000000000, 0.6928203230275494784 ) ) ;
#76530 = ORIENTED_EDGE ( 'NONE', *, *, #86293, .F. ) ;
#76529 = ORIENTED_EDGE ( 'NONE', *, *, #85061, .F. ) ;
#76531 = VERTEX_POINT ( 'NONE', #121176 ) ;
#76532 = CARTESIAN_POINT ( 'NONE',  ( -6.900000000000019007, 2.500000000000000000, -0.3464101615137783474 ) ) ;
#76533 = CIRCLE ( 'NONE', #89136, 0.1000000000000002554 ) ;
#76534 = LINE ( 'NONE', #85693, #119609 ) ;
#76535 = FACE_OUTER_BOUND ( 'NONE', #114577, .T. ) ;
#76536 = CIRCLE ( 'NONE', #15879, 0.06509327318403745899 ) ;
#76537 = PRODUCT_CONTEXT ( 'NONE', #37995, 'mechanical' ) ;
#76538 = DIRECTION ( 'NONE',  ( -0.000000000000000000, 1.000000000000000000, -0.000000000000000000 ) ) ;
#76539 = CARTESIAN_POINT ( 'NONE',  ( 187.2083333333333712, -4.445597072760123503, -7.699999999999989519 ) ) ;
#76540 = DIRECTION ( 'NONE',  ( 0.000000000000000000, 0.000000000000000000, -1.000000000000000000 ) ) ;
#76541 = DIRECTION ( 'NONE',  ( 0.000000000000000000, 0.000000000000000000, 1.000000000000000000 ) ) ;
#76542 = LINE ( 'NONE', #106633, #44664 ) ;
#76543 = CARTESIAN_POINT ( 'NONE',  ( 184.7812500006828031, 0.000000000000000000, 7.700000000000000178 ) ) ;
#76544 = EDGE_LOOP ( 'NONE', ( #37100, #22827 ) ) ;
#76545 = PLANE ( 'NONE',  #54999 ) ;
#76546 = VERTEX_POINT ( 'NONE', #113939 ) ;
#76547 = ORIENTED_EDGE ( 'NONE', *, *, #112115, .T. ) ;
#76548 = DIRECTION ( 'NONE',  ( 0.000000000000000000, 0.000000000000000000, 1.000000000000000000 ) ) ;
#76549 = CARTESIAN_POINT ( 'NONE',  ( -1.450000000000036371, 2.500000000000000000, 2.611473670974873151 ) ) ;
#76550 = DIRECTION ( 'NONE',  ( 0.000000000000000000, -0.9999939076577903929, 0.003490651415223739937 ) ) ;
#76551 = CARTESIAN_POINT ( 'NONE',  ( -9.400000000000009237, 2.500000000000000000, -4.776537180435973973 ) ) ;
#76552 = DIRECTION ( 'NONE',  ( 0.000000000000000000, 1.000000000000000000, 0.000000000000000000 ) ) ;
#76553 = PLANE ( 'NONE',  #15662 ) ;
#76554 = CIRCLE ( 'NONE', #95617, 0.1000000000000002554 ) ;
#76555 = DIRECTION ( 'NONE',  ( 0.000000000000000000, -0.9999939076577903929, 0.003490651415223739937 ) ) ;
#76556 = VERTEX_POINT ( 'NONE', #63553 ) ;
#76557 = DIRECTION ( 'NONE',  ( -0.000000000000000000, 1.000000000000000000, -0.000000000000000000 ) ) ;
#76558 = CONICAL_SURFACE ( 'NONE', #30603, 0.1000000000000002554, 0.003490658503988666988 ) ;
#76559 = CIRCLE ( 'NONE', #68228, 0.1000000000000002554 ) ;
#76560 = AXIS2_PLACEMENT_3D ( 'NONE', #122525, #62325, #121872 ) ;
#76561 = CARTESIAN_POINT ( 'NONE',  ( 187.5000000000000000, -1.375000000000000000, 7.576237522675751457 ) ) ;
#76562 = ORIENTED_EDGE ( 'NONE', *, *, #106310, .F. ) ;
#76563 = ORIENTED_EDGE ( 'NONE', *, *, #124276, .T. ) ;
#76564 = CIRCLE ( 'NONE', #86920, 0.09999999999999982514 ) ;
#76565 = ORIENTED_EDGE ( 'NONE', *, *, #33479, .T. ) ;
#76566 = ADVANCED_FACE ( 'NONE', ( #121814 ), #50257, .T. ) ;
#76567 = VERTEX_POINT ( 'NONE', #103472 ) ;
#76569 = ORIENTED_EDGE ( 'NONE', *, *, #69574, .F. ) ;
#76568 = EDGE_CURVE ( 'NONE', #109647, #34236, #69113, .T. ) ;
#76570 = DIRECTION ( 'NONE',  ( 0.000000000000000000, 0.000000000000000000, 1.000000000000000000 ) ) ;
#76571 = PLANE ( 'NONE',  #39447 ) ;
#76572 = VECTOR ( 'NONE', #97378, 1000.000000000000000 ) ;
#76573 = EDGE_LOOP ( 'NONE', ( #91359, #20240 ) ) ;
#76574 = DIRECTION ( 'NONE',  ( 0.000000000000000000, 0.000000000000000000, 1.000000000000000000 ) ) ;
#76575 = LINE ( 'NONE', #116481, #80077 ) ;
#76577 = AXIS2_PLACEMENT_3D ( 'NONE', #11122, #82474, #62191 ) ;
#76576 = VECTOR ( 'NONE', #28070, 1000.000000000000000 ) ;
#76578 = DIRECTION ( 'NONE',  ( 0.000000000000000000, 0.000000000000000000, 1.000000000000000000 ) ) ;
#76579 = ORIENTED_EDGE ( 'NONE', *, *, #94154, .T. ) ;
#76580 = ADVANCED_FACE ( 'NONE', ( #72725 ), #33541, .T. ) ;
#76581 = CARTESIAN_POINT ( 'NONE',  ( -5.650000000000023448, 2.500000000000000000, -2.511473670974877948 ) ) ;
#76582 = LINE ( 'NONE', #5248, #12184 ) ;
#76583 = ORIENTED_EDGE ( 'NONE', *, *, #74021, .T. ) ;
#76584 = VERTEX_POINT ( 'NONE', #82557 ) ;
#76585 = ORIENTED_EDGE ( 'NONE', *, *, #10557, .F. ) ;
#76586 = CARTESIAN_POINT ( 'NONE',  ( -2.500000000000031086, 2.500000000000000000, 3.637306695894644726 ) ) ;
#76587 = FACE_OUTER_BOUND ( 'NONE', #30686, .T. ) ;
#76588 = EDGE_CURVE ( 'NONE', #13198, #122791, #112650, .T. ) ;
#76589 = EDGE_LOOP ( 'NONE', ( #43655, #66577 ) ) ;
#76590 = CARTESIAN_POINT ( 'NONE',  ( 1.649999999999949729, 2.500000000000000000, 5.802370205355744659 ) ) ;
#76591 = CARTESIAN_POINT ( 'NONE',  ( -9.150000000000009237, 12.50000000000000000, -2.230156782645139391 ) ) ;
#76592 = DIRECTION ( 'NONE',  ( 0.000000000000000000, 0.000000000000000000, -1.000000000000000000 ) ) ;
#76593 = CARTESIAN_POINT ( 'NONE',  ( -7.500000000000011546, 2.500000000000000000, 3.537306695894645081 ) ) ;
#76594 = EDGE_CURVE ( 'NONE', #25630, #117051, #102806, .T. ) ;
#76595 = VERTEX_POINT ( 'NONE', #115860 ) ;
#76596 = AXIS2_PLACEMENT_3D ( 'NONE', #9865, #89709, #110004 ) ;
#76597 = CARTESIAN_POINT ( 'NONE',  ( 5.399999999999933742, 12.50000000000000000, -2.385244779468109755E-15 ) ) ;
#76598 = CIRCLE ( 'NONE', #114249, 0.06509327318403745899 ) ;
#76599 = ORIENTED_EDGE ( 'NONE', *, *, #58854, .F. ) ;
#76600 = ORIENTED_EDGE ( 'NONE', *, *, #115422, .F. ) ;
#76601 = EDGE_CURVE ( 'NONE', #60131, #66442, #39806, .T. ) ;
#76602 = EDGE_LOOP ( 'NONE', ( #51892, #13007 ) ) ;
#76603 = EDGE_CURVE ( 'NONE', #61095, #110247, #44002, .T. ) ;
#76604 = DIRECTION ( 'NONE',  ( -0.000000000000000000, 1.000000000000000000, -0.000000000000000000 ) ) ;
#76605 = ADVANCED_FACE ( 'NONE', ( #27462 ), #4254, .T. ) ;
#76606 = FACE_BOUND ( 'NONE', #115702, .T. ) ;
#76607 = EDGE_CURVE ( 'NONE', #85332, #110789, #16973, .T. ) ;
#76608 = DIRECTION ( 'NONE',  ( 0.000000000000000000, -0.9999939076577903929, 0.003490651415223739937 ) ) ;
#76609 = DIRECTION ( 'NONE',  ( -0.000000000000000000, -1.000000000000000000, -0.000000000000000000 ) ) ;
#76611 = CONICAL_SURFACE ( 'NONE', #82882, 0.1000000000000000472, 0.003490658503988666988 ) ;
#76610 = CONICAL_SURFACE ( 'NONE', #103798, 0.1000000000000002554, 0.003490658503988666988 ) ;
#76612 = CARTESIAN_POINT ( 'NONE',  ( 10.79999999999991012, 12.50000000000000000, 4.265033745738159077 ) ) ;
#76613 = EDGE_CURVE ( 'NONE', #98705, #57456, #18929, .T. ) ;
#76614 = VERTEX_POINT ( 'NONE', #16348 ) ;
#76615 = CARTESIAN_POINT ( 'NONE',  ( -11.44999999999999751, 2.500000000000000000, -6.841600689897074261 ) ) ;
#76616 = CARTESIAN_POINT ( 'NONE',  ( -5.800000000000018474, 2.500000000000000000, 0.09999999999999772959 ) ) ;
#76617 = EDGE_CURVE ( 'NONE', #81382, #41325, #36021, .T. ) ;
#76618 = CARTESIAN_POINT ( 'NONE',  ( 15.83209681635554666, 2.500000000000000000, 5.404881881984142211 ) ) ;
#76619 = DIRECTION ( 'NONE',  ( 0.000000000000000000, 1.000000000000000000, 0.000000000000000000 ) ) ;
#76620 = ORIENTED_EDGE ( 'NONE', *, *, #105278, .T. ) ;
#76622 = CONICAL_SURFACE ( 'NONE', #9723, 0.1000000000000002554, 0.003490658503988666988 ) ;
#76621 = CONICAL_SURFACE ( 'NONE', #20186, 0.09999999999999982514, 0.003490658503988666988 ) ;
#76623 = CARTESIAN_POINT ( 'NONE',  ( -8.550000000000011369, 12.50000000000000000, -2.511473670974877948 ) ) ;
#76624 = CONICAL_SURFACE ( 'NONE', #97540, 0.1000000000000000472, 0.003490658503988666988 ) ;
#76625 = ADVANCED_FACE ( 'NONE', ( #76587 ), #95587, .T. ) ;
#76626 = DIRECTION ( 'NONE',  ( 0.000000000000000000, 0.000000000000000000, 1.000000000000000000 ) ) ;
#76627 = ORIENTED_EDGE ( 'NONE', *, *, #30411, .F. ) ;
#76628 = CARTESIAN_POINT ( 'NONE',  ( 11.24999999999994493, 12.50000000000000000, 6.495190528383297135 ) ) ;
#76629 = ADVANCED_FACE ( 'NONE', ( #65466 ), #96207, .T. ) ;
#76630 = DIRECTION ( 'NONE',  ( -0.000000000000000000, -1.000000000000000000, -0.000000000000000000 ) ) ;
#76631 = FACE_BOUND ( 'NONE', #5780, .T. ) ;
#76632 = EDGE_CURVE ( 'NONE', #1197, #38017, #77432, .T. ) ;
#76633 = DIRECTION ( 'NONE',  ( 0.000000000000000000, 1.000000000000000000, 0.000000000000000000 ) ) ;
#76634 = ORIENTED_EDGE ( 'NONE', *, *, #53878, .T. ) ;
#76635 = FACE_OUTER_BOUND ( 'NONE', #6427, .T. ) ;
#76636 = VERTEX_POINT ( 'NONE', #66753 ) ;
#76637 = ORIENTED_EDGE ( 'NONE', *, *, #79763, .F. ) ;
#76638 = CARTESIAN_POINT ( 'NONE',  ( 184.0885416670080872, -6.551208109652273848, -3.782341765625003571 ) ) ;
#76639 = AXIS2_PLACEMENT_3D ( 'NONE', #81013, #112411, #41108 ) ;
#76640 = EDGE_LOOP ( 'NONE', ( #125012, #27346, #89508, #87374 ) ) ;
#76641 = CARTESIAN_POINT ( 'NONE',  ( 184.5468750003414300, -8.734944146203032389, -1.604583208406767949E-15 ) ) ;
#76642 = AXIS2_PLACEMENT_3D ( 'NONE', #29028, #10017, #88569 ) ;
#76643 = PLANE ( 'NONE',  #59512 ) ;
#76644 = AXIS2_PLACEMENT_3D ( 'NONE', #125386, #46836, #64521 ) ;
#76645 = CARTESIAN_POINT ( 'NONE',  ( -7.300000000000014921, 12.50000000000000000, 4.676537180435972552 ) ) ;
#76646 = CARTESIAN_POINT ( 'NONE',  ( -4.600000000000028066, 12.50000000000000000, -3.637306695894650055 ) ) ;
#76647 = AXIS2_PLACEMENT_3D ( 'NONE', #79696, #29972, #69888 ) ;
#76648 = VERTEX_POINT ( 'NONE', #55005 ) ;
#76649 = AXIS2_PLACEMENT_3D ( 'NONE', #25420, #55553, #54891 ) ;
#76650 = FACE_OUTER_BOUND ( 'NONE', #67871, .T. ) ;
#76651 = DIRECTION ( 'NONE',  ( 0.000000000000000000, 0.000000000000000000, 1.000000000000000000 ) ) ;
#76652 = DIRECTION ( 'NONE',  ( 0.000000000000000000, 0.000000000000000000, -1.000000000000000000 ) ) ;
#76653 = CARTESIAN_POINT ( 'NONE',  ( 18.46077503350462479, 0.2574728941691944994, -4.048716373199866325 ) ) ;
#76654 = VERTEX_POINT ( 'NONE', #125667 ) ;
#76655 = DIRECTION ( 'NONE',  ( 0.000000000000000000, 1.000000000000000000, 0.000000000000000000 ) ) ;
#76656 = VERTEX_POINT ( 'NONE', #37323 ) ;
#76657 = AXIS2_PLACEMENT_3D ( 'NONE', #98237, #39356, #108706 ) ;
#76658 = CARTESIAN_POINT ( 'NONE',  ( 0.4499999999999552136, 12.50000000000000000, 6.430097255199259010 ) ) ;
#76659 = DIRECTION ( 'NONE',  ( 0.000000000000000000, 0.000000000000000000, 1.000000000000000000 ) ) ;
#76660 = CIRCLE ( 'NONE', #118418, 0.06509327318403743123 ) ;
#76661 = ORIENTED_EDGE ( 'NONE', *, *, #34794, .T. ) ;
#76662 = CARTESIAN_POINT ( 'NONE',  ( -4.150000000000025224, 2.500000000000000000, 2.857883832488649301 ) ) ;
#76663 = CARTESIAN_POINT ( 'NONE',  ( 17.50000000000000000, -2.499999999999999556, -3.333333333333330373 ) ) ;
#76664 = ADVANCED_FACE ( 'NONE', ( #25532 ), #94946, .T. ) ;
#76665 = CARTESIAN_POINT ( 'NONE',  ( -5.650000000000019895, 2.500000000000000000, 1.918653347947321564 ) ) ;
#76667 = AXIS2_PLACEMENT_3D ( 'NONE', #114488, #54919, #85025 ) ;
#76666 = CIRCLE ( 'NONE', #9764, 0.1000000000000002554 ) ;
#76668 = LINE ( 'NONE', #16421, #69562 ) ;
#76669 = ORIENTED_EDGE ( 'NONE', *, *, #86187, .F. ) ;
#76671 = EDGE_CURVE ( 'NONE', #20888, #80635, #117123, .T. ) ;
#76670 = DIRECTION ( 'NONE',  ( 0.000000000000000000, 1.000000000000000000, 0.000000000000000000 ) ) ;
#76672 = CARTESIAN_POINT ( 'NONE',  ( 10.39999999999990976, 12.50000000000000000, 4.265033745738159077 ) ) ;
#76673 = CARTESIAN_POINT ( 'NONE',  ( -4.150000000000024336, 12.50000000000000000, 2.165063509461097713 ) ) ;
#76674 = DIRECTION ( 'NONE',  ( 0.000000000000000000, -0.000000000000000000, 1.000000000000000000 ) ) ;
#76675 = LINE ( 'NONE', #28218, #9700 ) ;
#76676 = ORIENTED_EDGE ( 'NONE', *, *, #116326, .T. ) ;
#76677 = ORIENTED_EDGE ( 'NONE', *, *, #55470, .F. ) ;
#76678 = CARTESIAN_POINT ( 'NONE',  ( -11.24999999999996447, 12.50000000000000000, -2.165063509461097713 ) ) ;
#76679 = ORIENTED_EDGE ( 'NONE', *, *, #8376, .T. ) ;
#76680 = DIRECTION ( 'NONE',  ( -0.000000000000000000, 1.000000000000000000, -0.000000000000000000 ) ) ;
#76682 = VERTEX_POINT ( 'NONE', #86394 ) ;
#76681 = VERTEX_POINT ( 'NONE', #7184 ) ;
#76683 = ORIENTED_EDGE ( 'NONE', *, *, #1078, .T. ) ;
#76684 = AXIS2_PLACEMENT_3D ( 'NONE', #107744, #18061, #58011 ) ;
#76685 = DIRECTION ( 'NONE',  ( 0.000000000000000000, 0.000000000000000000, 1.000000000000000000 ) ) ;
#76686 = CARTESIAN_POINT ( 'NONE',  ( -11.44999999999999751, 12.50000000000000000, 6.148780366869520897 ) ) ;
#76687 = DIRECTION ( 'NONE',  ( 0.000000000000000000, -0.000000000000000000, 1.000000000000000000 ) ) ;
#76688 = CARTESIAN_POINT ( 'NONE',  ( -5.450000000000023270, 12.50000000000000000, -6.560283801567339701 ) ) ;
#76689 = DIRECTION ( 'NONE',  ( 0.000000000000000000, 0.000000000000000000, 1.000000000000000000 ) ) ;
#76690 = CARTESIAN_POINT ( 'NONE',  ( 0.1999999999999567124, 12.50000000000000000, -3.983716857408426293 ) ) ;
#76691 = ORIENTED_EDGE ( 'NONE', *, *, #82868, .F. ) ;
#76692 = DIRECTION ( 'NONE',  ( 0.000000000000000000, 0.000000000000000000, 1.000000000000000000 ) ) ;
#76693 = VERTEX_POINT ( 'NONE', #77229 ) ;
#76695 = ORIENTED_EDGE ( 'NONE', *, *, #25304, .T. ) ;
#76694 = CONICAL_SURFACE ( 'NONE', #120608, 0.09999999999999982514, 0.003490658503988666988 ) ;
#76696 = ORIENTED_EDGE ( 'NONE', *, *, #43569, .T. ) ;
#76697 = ORIENTED_EDGE ( 'NONE', *, *, #105553, .F. ) ;
#76698 = VECTOR ( 'NONE', #46808, 1000.000000000000000 ) ;
#76699 = CARTESIAN_POINT ( 'NONE',  ( -10.60000000000000142, 12.50000000000000000, -0.2813168883297408329 ) ) ;
#76700 = EDGE_LOOP ( 'NONE', ( #127205, #81673, #95908, #114679 ) ) ;
#76701 = ORIENTED_EDGE ( 'NONE', *, *, #39922, .F. ) ;
#76702 = CIRCLE ( 'NONE', #36996, 0.06509327318403745899 ) ;
#76703 = ADVANCED_FACE ( 'NONE', ( #47137 ), #87040, .T. ) ;
#76704 = CARTESIAN_POINT ( 'NONE',  ( -10.40000000000000213, 12.50000000000000000, 0.7579135962115869374 ) ) ;
#76705 = CARTESIAN_POINT ( 'NONE',  ( 6.649999999999928413, 2.500000000000000000, 1.472243186433545459 ) ) ;
#76706 = CARTESIAN_POINT ( 'NONE',  ( 10.44999999999991047, 2.500000000000000000, 2.265063509461097357 ) ) ;
#76707 = CARTESIAN_POINT ( 'NONE',  ( 11.64999999999990798, 2.500000000000000000, 5.802370205355744659 ) ) ;
#76708 = DIRECTION ( 'NONE',  ( -0.000000000000000000, 1.000000000000000000, -0.000000000000000000 ) ) ;
#76709 = ORIENTED_EDGE ( 'NONE', *, *, #34854, .T. ) ;
#76710 = DIRECTION ( 'NONE',  ( 0.000000000000000000, 0.000000000000000000, 1.000000000000000000 ) ) ;
#76711 = CIRCLE ( 'NONE', #101845, 0.09999999999999982514 ) ;
#76712 = ADVANCED_FACE ( 'NONE', ( #44551 ), #74648, .T. ) ;
#76713 = EDGE_LOOP ( 'NONE', ( #57431, #88975, #100138, #48860 ) ) ;
#76714 = DIRECTION ( 'NONE',  ( -0.000000000000000000, 1.000000000000000000, -0.000000000000000000 ) ) ;
#76715 = AXIS2_PLACEMENT_3D ( 'NONE', #83417, #25768, #63114 ) ;
#76716 = EDGE_LOOP ( 'NONE', ( #71368, #15567 ) ) ;
#76717 = DIRECTION ( 'NONE',  ( -0.000000000000000000, 1.000000000000000000, -0.000000000000000000 ) ) ;
#76718 = EDGE_LOOP ( 'NONE', ( #39616, #47697, #89717, #115155 ) ) ;
#76719 = ADVANCED_FACE ( 'NONE', ( #5255 ), #14721, .T. ) ;
#76720 = ADVANCED_FACE ( 'NONE', ( #75292 ), #16769, .T. ) ;
#76721 = VERTEX_POINT ( 'NONE', #98791 ) ;
#76722 = FACE_OUTER_BOUND ( 'NONE', #62329, .T. ) ;
#76723 = DIRECTION ( 'NONE',  ( -0.000000000000000000, 1.000000000000000000, -0.000000000000000000 ) ) ;
#76724 = CARTESIAN_POINT ( 'NONE',  ( 11.24999999999991118, 2.500000000000000000, -2.957883832488653830 ) ) ;
#76725 = DIRECTION ( 'NONE',  ( 0.000000000000000000, 1.000000000000000000, 0.000000000000000000 ) ) ;
#76726 = CARTESIAN_POINT ( 'NONE',  ( -13.34999999999999076, 2.500000000000000000, 2.957883832488652942 ) ) ;
#76727 = ORIENTED_EDGE ( 'NONE', *, *, #31586, .T. ) ;
#76728 = CARTESIAN_POINT ( 'NONE',  ( -13.09999999999999254, 12.50000000000000000, -3.983716857408423628 ) ) ;
#76729 = CARTESIAN_POINT ( 'NONE',  ( 1.249999999999986899, 2.500000000000000000, 6.595190528383296780 ) ) ;
#76730 = EDGE_CURVE ( 'NONE', #121037, #32550, #19604, .T. ) ;
#76731 = CARTESIAN_POINT ( 'NONE',  ( -5.000000000000024869, 2.500000000000000000, -5.022947341949754119 ) ) ;
#76732 = CIRCLE ( 'NONE', #101778, 0.06509327318403745899 ) ;
#76733 = PLANE ( 'NONE',  #88944 ) ;
#76734 = CONICAL_SURFACE ( 'NONE', #103924, 0.1000000000000002554, 0.003490658503988666988 ) ;
#76735 = CONICAL_SURFACE ( 'NONE', #32939, 0.1000000000000000472, 0.003490658503988666988 ) ;
#76736 = DIRECTION ( 'NONE',  ( -0.000000000000000000, 1.000000000000000000, -0.000000000000000000 ) ) ;
#76737 = ORIENTED_EDGE ( 'NONE', *, *, #119651, .T. ) ;
#76738 = CIRCLE ( 'NONE', #124760, 0.06509327318403745899 ) ;
#76739 = ORIENTED_EDGE ( 'NONE', *, *, #122751, .F. ) ;
#76740 = DIRECTION ( 'NONE',  ( 0.000000000000000000, -0.000000000000000000, 1.000000000000000000 ) ) ;
#76741 = CIRCLE ( 'NONE', #24416, 0.1000000000000002554 ) ;
#76742 = EDGE_LOOP ( 'NONE', ( #66719, #63773, #746, #54895 ) ) ;
#76743 = CIRCLE ( 'NONE', #116437, 0.06509327318403745899 ) ;
#76744 = LINE ( 'NONE', #105563, #27796 ) ;
#76745 = DIRECTION ( 'NONE',  ( -0.000000000000000000, -1.000000000000000000, -0.000000000000000000 ) ) ;
#76746 = AXIS2_PLACEMENT_3D ( 'NONE', #121180, #100884, #120541 ) ;
#76747 = VERTEX_POINT ( 'NONE', #8473 ) ;
#76748 = CARTESIAN_POINT ( 'NONE',  ( 184.7916666666666856, 4.445597072760120838, -7.699999999999998401 ) ) ;
#76750 = CONICAL_SURFACE ( 'NONE', #72645, 0.1000000000000002554, 0.003490658503988666988 ) ;
#76749 = CARTESIAN_POINT ( 'NONE',  ( 10.59999999999991260, 2.500000000000000000, 0.3464101615137735735 ) ) ;
#76751 = DIRECTION ( 'NONE',  ( 0.000000000000000000, 0.000000000000000000, 1.000000000000000000 ) ) ;
#76752 = DIRECTION ( 'NONE',  ( 0.000000000000000000, 1.000000000000000000, 0.000000000000000000 ) ) ;
#76753 = LINE ( 'NONE', #95107, #28773 ) ;
#76754 = ORIENTED_EDGE ( 'NONE', *, *, #20042, .T. ) ;
#76755 = CONICAL_SURFACE ( 'NONE', #37053, 0.1000000000000000472, 0.003490658503988666988 ) ;
#76756 = ADVANCED_FACE ( 'NONE', ( #40556 ), #125632, .T. ) ;
#76758 = AXIS2_PLACEMENT_3D ( 'NONE', #43684, #14179, #12882 ) ;
#76757 = AXIS2_PLACEMENT_3D ( 'NONE', #6164, #35025, #4873 ) ;
#76759 = DIRECTION ( 'NONE',  ( 0.000000000000000000, 0.000000000000000000, -1.000000000000000000 ) ) ;
#76760 = FACE_OUTER_BOUND ( 'NONE', #113083, .T. ) ;
#76761 = ORIENTED_EDGE ( 'NONE', *, *, #101131, .F. ) ;
#76762 = EDGE_CURVE ( 'NONE', #120592, #50078, #6390, .T. ) ;
#76763 = CARTESIAN_POINT ( 'NONE',  ( 195.5000000000000000, 0.000000000000000000, 0.000000000000000000 ) ) ;
#76764 = CARTESIAN_POINT ( 'NONE',  ( 0.7999999999999548583, 2.500000000000000000, 4.330127018922196314 ) ) ;
#76765 = ADVANCED_FACE ( 'NONE', ( #39275 ), #128939, .T. ) ;
#76766 = FACE_OUTER_BOUND ( 'NONE', #107296, .T. ) ;
#76767 = EDGE_LOOP ( 'NONE', ( #45575, #92284 ) ) ;
#76768 = LINE ( 'NONE', #38128, #111664 ) ;
#76769 = EDGE_CURVE ( 'NONE', #7349, #89205, #102557, .T. ) ;
#76770 = ADVANCED_FACE ( 'NONE', ( #49726 ), #25275, .T. ) ;
#76771 = EDGE_LOOP ( 'NONE', ( #114936, #61080, #77735, #6471 ) ) ;
#76772 = DIRECTION ( 'NONE',  ( 0.000000000000000000, 1.000000000000000000, 0.000000000000000000 ) ) ;
#76773 = DIRECTION ( 'NONE',  ( 0.000000000000000000, 0.000000000000000000, 1.000000000000000000 ) ) ;
#76774 = EDGE_CURVE ( 'NONE', #116336, #16823, #31561, .T. ) ;
#76775 = VECTOR ( 'NONE', #35917, 1000.000000000000000 ) ;
#76776 = ADVANCED_FACE ( 'NONE', ( #79805 ), #46136, .T. ) ;
#76777 = CARTESIAN_POINT ( 'NONE',  ( 1.849999999999948130, 12.50000000000000000, 6.083687093685482772 ) ) ;
#76778 = EDGE_LOOP ( 'NONE', ( #20029, #29227 ) ) ;
#76779 = CARTESIAN_POINT ( 'NONE',  ( -10.00000000000000355, 2.500000000000000000, -0.6928203230275541413 ) ) ;
#76780 = EDGE_CURVE ( 'NONE', #34168, #121648, #75463, .T. ) ;
#76781 = CARTESIAN_POINT ( 'NONE',  ( 186.6666666666666856, -6.668395609140176816, -3.850000000000003642 ) ) ;
#76782 = ORIENTED_EDGE ( 'NONE', *, *, #80139, .F. ) ;
#76783 = VERTEX_POINT ( 'NONE', #70632 ) ;
#76784 = EDGE_CURVE ( 'NONE', #65382, #59496, #23145, .T. ) ;
#76785 = CARTESIAN_POINT ( 'NONE',  ( -9.150000000000009237, 12.50000000000000000, -1.472243186433550122 ) ) ;
#76786 = AXIS2_PLACEMENT_3D ( 'NONE', #31301, #21457, #89554 ) ;
#76787 = AXIS2_PLACEMENT_3D ( 'NONE', #121333, #123276, #31673 ) ;
#76788 = VERTEX_POINT ( 'NONE', #69998 ) ;
#76789 = LINE ( 'NONE', #98340, #88146 ) ;
#76790 = CARTESIAN_POINT ( 'NONE',  ( -12.09999999999999609, 12.50000000000000000, 0.6928203230275535862 ) ) ;
#76791 = EDGE_LOOP ( 'NONE', ( #16719, #17856 ) ) ;
#76792 = ORIENTED_EDGE ( 'NONE', *, *, #32799, .T. ) ;
#76793 = DIRECTION ( 'NONE',  ( -4.274815082592931898E-19, -0.9999939076577903929, -0.003490651415223739937 ) ) ;
#76794 = DIRECTION ( 'NONE',  ( 0.000000000000000000, 1.000000000000000000, 0.000000000000000000 ) ) ;
#76795 = EDGE_LOOP ( 'NONE', ( #122909, #37743 ) ) ;
#76797 = CIRCLE ( 'NONE', #116490, 0.06509327318403745899 ) ;
#76796 = AXIS2_PLACEMENT_3D ( 'NONE', #49571, #70481, #18795 ) ;
#76798 = DIRECTION ( 'NONE',  ( 0.000000000000000000, 0.000000000000000000, 1.000000000000000000 ) ) ;
#76799 = CARTESIAN_POINT ( 'NONE',  ( 12.89999999999990266, 12.50000000000000000, 5.022947341949748790 ) ) ;
#76800 = AXIS2_PLACEMENT_3D ( 'NONE', #119193, #9241, #18410 ) ;
#76801 = CARTESIAN_POINT ( 'NONE',  ( 16.80832070732106232, -1.716026667539209516, -5.822501722885366604 ) ) ;
#76802 = DIRECTION ( 'NONE',  ( 0.000000000000000000, 0.000000000000000000, 1.000000000000000000 ) ) ;
#76803 = FACE_OUTER_BOUND ( 'NONE', #117386, .T. ) ;
#76804 = CARTESIAN_POINT ( 'NONE',  ( 87.50000000000001421, -3.975350567648449740, -6.360562287258772152 ) ) ;
#76806 = CIRCLE ( 'NONE', #89324, 0.06509327318403745899 ) ;
#76805 = AXIS2_PLACEMENT_3D ( 'NONE', #78856, #87984, #87345 ) ;
#76807 = CIRCLE ( 'NONE', #91466, 0.09999999999999982514 ) ;
#76808 = ORIENTED_EDGE ( 'NONE', *, *, #106634, .T. ) ;
#76809 = VERTEX_POINT ( 'NONE', #68049 ) ;
#76810 = VERTEX_POINT ( 'NONE', #109925 ) ;
#76811 = EDGE_LOOP ( 'NONE', ( #84428, #94916 ) ) ;
#76812 = CARTESIAN_POINT ( 'NONE',  ( -0.8500000000000382805, 12.50000000000000000, -7.188010851410854052 ) ) ;
#76813 = DIRECTION ( 'NONE',  ( 0.000000000000000000, 1.000000000000000000, 0.000000000000000000 ) ) ;
#76814 = DIRECTION ( 'NONE',  ( 0.000000000000000000, 1.000000000000000000, 0.000000000000000000 ) ) ;
#76815 = EDGE_LOOP ( 'NONE', ( #37940, #6852 ) ) ;
#76816 = FACE_BOUND ( 'NONE', #85957, .T. ) ;
#76817 = CARTESIAN_POINT ( 'NONE',  ( 4.149999999999939959, 2.500000000000000000, -2.065063509461102065 ) ) ;
#76818 = DIRECTION ( 'NONE',  ( 0.000000000000000000, 0.000000000000000000, 1.000000000000000000 ) ) ;
#76819 = DIRECTION ( 'NONE',  ( 0.000000000000000000, 1.000000000000000000, 0.000000000000000000 ) ) ;
#76820 = CONICAL_SURFACE ( 'NONE', #120722, 0.09999999999999999167, 0.003490658503988666988 ) ;
#76821 = ADVANCED_FACE ( 'NONE', ( #20248 ), #33620, .T. ) ;
#76822 = CARTESIAN_POINT ( 'NONE',  ( -9.600000000000008527, 2.500000000000000000, 4.230127018922196669 ) ) ;
#76823 = CARTESIAN_POINT ( 'NONE',  ( -3.150000000000029665, 12.50000000000000000, 6.841600689897072485 ) ) ;
#76824 = AXIS2_PLACEMENT_3D ( 'NONE', #129341, #39673, #107739 ) ;
#76825 = CARTESIAN_POINT ( 'NONE',  ( 0.4499999999999552136, 2.500000000000000000, 6.595190528383296780 ) ) ;
#76826 = CARTESIAN_POINT ( 'NONE',  ( 4.349999999999940137, 12.50000000000000000, -6.841600689897078702 ) ) ;
#76827 = FACE_OUTER_BOUND ( 'NONE', #77545, .T. ) ;
#76828 = CARTESIAN_POINT ( 'NONE',  ( -11.84999999999999787, 2.500000000000000000, -2.611473670974873595 ) ) ;
#76829 = CIRCLE ( 'NONE', #5785, 0.09999999999999982514 ) ;
#76830 = LINE ( 'NONE', #116733, #27234 ) ;
#76831 = EDGE_CURVE ( 'NONE', #105454, #47303, #8549, .T. ) ;
#76832 = ORIENTED_EDGE ( 'NONE', *, *, #125365, .T. ) ;
#76834 = EDGE_LOOP ( 'NONE', ( #5156, #52423, #36392, #28026 ) ) ;
#76833 = CIRCLE ( 'NONE', #81041, 0.06509327318403743123 ) ;
#76835 = ORIENTED_EDGE ( 'NONE', *, *, #42018, .T. ) ;
#76836 = ORIENTED_EDGE ( 'NONE', *, *, #38288, .F. ) ;
#76837 = DIRECTION ( 'NONE',  ( 0.000000000000000000, -0.000000000000000000, 1.000000000000000000 ) ) ;
#76838 = DIRECTION ( 'NONE',  ( -0.000000000000000000, 1.000000000000000000, -0.000000000000000000 ) ) ;
#76840 = ORIENTED_EDGE ( 'NONE', *, *, #56398, .T. ) ;
#76839 = EDGE_LOOP ( 'NONE', ( #89035, #110130 ) ) ;
#76842 = EDGE_LOOP ( 'NONE', ( #7378, #6687 ) ) ;
#76841 = CONICAL_SURFACE ( 'NONE', #51705, 0.1000000000000000472, 0.003490658503988666988 ) ;
#76844 = AXIS2_PLACEMENT_3D ( 'NONE', #37700, #9527, #118829 ) ;
#76843 = DIRECTION ( 'NONE',  ( 0.000000000000000000, 0.000000000000000000, -1.000000000000000000 ) ) ;
#76845 = CIRCLE ( 'NONE', #104025, 0.09999999999999982514 ) ;
#76846 = CIRCLE ( 'NONE', #41253, 0.1000000000000002554 ) ;
#76847 = CARTESIAN_POINT ( 'NONE',  ( 3.709550432145070076, -2.499999999998979483, 9.999999999913205428 ) ) ;
#76848 = CARTESIAN_POINT ( 'NONE',  ( -9.600000000000008527, 2.500000000000000000, -3.637306695894645614 ) ) ;
#76849 = CARTESIAN_POINT ( 'NONE',  ( 5.199999999999935341, 2.500000000000000000, -0.3464101615137783474 ) ) ;
#76850 = CARTESIAN_POINT ( 'NONE',  ( 187.2395833340161460, 4.445597072760117285, 7.700000000000001066 ) ) ;
#76851 = CIRCLE ( 'NONE', #45551, 0.06509327318403745899 ) ;
#76852 = EDGE_LOOP ( 'NONE', ( #112181, #5747, #67823, #108447 ) ) ;
#76853 = ORIENTED_EDGE ( 'NONE', *, *, #36681, .T. ) ;
#76855 = CIRCLE ( 'NONE', #81064, 0.1000000000000002554 ) ;
#76854 = AXIS2_PLACEMENT_3D ( 'NONE', #28410, #98411, #8738 ) ;
#76856 = VERTEX_POINT ( 'NONE', #589 ) ;
#76857 = VERTEX_POINT ( 'NONE', #20891 ) ;
#76858 = CARTESIAN_POINT ( 'NONE',  ( 8.549999999999918998, 2.500000000000000000, -1.818653347947326138 ) ) ;
#76859 = ORIENTED_EDGE ( 'NONE', *, *, #54007, .F. ) ;
#76860 = EDGE_LOOP ( 'NONE', ( #37094, #33859, #67030, #49410 ) ) ;
#76861 = DIRECTION ( 'NONE',  ( 0.000000000000000000, -0.000000000000000000, 1.000000000000000000 ) ) ;
#76862 = EDGE_CURVE ( 'NONE', #122612, #79666, #100506, .T. ) ;
#76863 = DIRECTION ( 'NONE',  ( 0.000000000000000000, 0.000000000000000000, 1.000000000000000000 ) ) ;
#76864 = DIRECTION ( 'NONE',  ( -0.000000000000000000, -1.000000000000000000, -0.000000000000000000 ) ) ;
#76865 = DIRECTION ( 'NONE',  ( 0.000000000000000000, 0.000000000000000000, 1.000000000000000000 ) ) ;
#76866 = DIRECTION ( 'NONE',  ( -0.000000000000000000, 1.000000000000000000, -0.000000000000000000 ) ) ;
#76867 = AXIS2_PLACEMENT_3D ( 'NONE', #68595, #28041, #37849 ) ;
#76868 = ORIENTED_EDGE ( 'NONE', *, *, #46519, .T. ) ;
#76869 = DIRECTION ( 'NONE',  ( 0.000000000000000000, 0.000000000000000000, 1.000000000000000000 ) ) ;
#76870 = EDGE_CURVE ( 'NONE', #99802, #3837, #38619, .T. ) ;
#76871 = ORIENTED_EDGE ( 'NONE', *, *, #70434, .T. ) ;
#76872 = DIRECTION ( 'NONE',  ( 0.000000000000000000, 0.000000000000000000, 1.000000000000000000 ) ) ;
#76873 = ORIENTED_EDGE ( 'NONE', *, *, #1862, .T. ) ;
#76874 = DIRECTION ( 'NONE',  ( 0.000000000000000000, 0.000000000000000000, 1.000000000000000000 ) ) ;
#76875 = CARTESIAN_POINT ( 'NONE',  ( -8.750000000000008882, 2.500000000000000000, 1.372243186433545370 ) ) ;
#76876 = VERTEX_POINT ( 'NONE', #108618 ) ;
#76878 = EDGE_CURVE ( 'NONE', #12513, #3855, #127698, .T. ) ;
#76877 = CARTESIAN_POINT ( 'NONE',  ( 14.14999999999989733, 12.50000000000000000, 2.857883832488649301 ) ) ;
#76879 = DIRECTION ( 'NONE',  ( 0.000000000000000000, 0.000000000000000000, 1.000000000000000000 ) ) ;
#76880 = EDGE_CURVE ( 'NONE', #128103, #53498, #44078, .T. ) ;
#76881 = EDGE_LOOP ( 'NONE', ( #72433, #86687, #81658, #94302 ) ) ;
#76882 = EDGE_CURVE ( 'NONE', #28690, #2868, #81730, .T. ) ;
#76883 = CARTESIAN_POINT ( 'NONE',  ( 11.24999999999994316, 2.500000000000000000, 2.065063509461097624 ) ) ;
#76884 = ORIENTED_EDGE ( 'NONE', *, *, #21936, .F. ) ;
#76885 = VERTEX_POINT ( 'NONE', #72578 ) ;
#76886 = DIRECTION ( 'NONE',  ( 0.000000000000000000, 0.000000000000000000, -1.000000000000000000 ) ) ;
#76887 = FACE_OUTER_BOUND ( 'NONE', #104819, .T. ) ;
#76888 = EDGE_CURVE ( 'NONE', #110798, #9926, #106760, .T. ) ;
#76889 = CARTESIAN_POINT ( 'NONE',  ( 185.5468750003414300, -8.734944146203032389, -1.604583208406768146E-15 ) ) ;
#76890 = DIRECTION ( 'NONE',  ( -0.000000000000000000, -1.000000000000000000, -0.000000000000000000 ) ) ;
#76891 = AXIS2_PLACEMENT_3D ( 'NONE', #118715, #123074, #52392 ) ;
#76892 = VECTOR ( 'NONE', #21639, 1000.000000000000000 ) ;
#76893 = DIRECTION ( 'NONE',  ( 0.000000000000000000, 1.000000000000000000, 0.000000000000000000 ) ) ;
#76894 = DIRECTION ( 'NONE',  ( -1.000000000000000000, 0.000000000000000000, 0.000000000000000000 ) ) ;
#76895 = ORIENTED_EDGE ( 'NONE', *, *, #50637, .F. ) ;
#76896 = FACE_OUTER_BOUND ( 'NONE', #61046, .T. ) ;
#76897 = CIRCLE ( 'NONE', #20465, 0.06509327318403745899 ) ;
#76898 = ORIENTED_EDGE ( 'NONE', *, *, #46411, .F. ) ;
#76899 = AXIS2_PLACEMENT_3D ( 'NONE', #63846, #54025, #44190 ) ;
#76900 = CARTESIAN_POINT ( 'NONE',  ( 7.299999999999926104, 12.50000000000000000, -0.3464101615137782364 ) ) ;
#76901 = LINE ( 'NONE', #88653, #105399 ) ;
#76902 = DIRECTION ( 'NONE',  ( 0.000000000000000000, 0.000000000000000000, 1.000000000000000000 ) ) ;
#76903 = DIRECTION ( 'NONE',  ( 0.000000000000000000, 1.000000000000000000, 0.000000000000000000 ) ) ;
#76904 = DIRECTION ( 'NONE',  ( 0.000000000000000000, 0.000000000000000000, 1.000000000000000000 ) ) ;
#76905 = ORIENTED_EDGE ( 'NONE', *, *, #127941, .F. ) ;
#76906 = CIRCLE ( 'NONE', #3739, 0.06509327318403745899 ) ;
#76907 = CARTESIAN_POINT ( 'NONE',  ( 1.049999999999954525, 12.50000000000000000, -2.446380397790840266 ) ) ;
#76908 = CIRCLE ( 'NONE', #20486, 0.09999999999999982514 ) ;
#76909 = CONICAL_SURFACE ( 'NONE', #72811, 0.09999999999999982514, 0.003490658503988666988 ) ;
#76910 = EDGE_LOOP ( 'NONE', ( #104280, #72537, #83494, #71173 ) ) ;
#76911 = AXIS2_PLACEMENT_3D ( 'NONE', #32765, #111271, #22297 ) ;
#76912 = CARTESIAN_POINT ( 'NONE',  ( -9.150000000000005684, 2.500000000000000000, 5.802370205355744659 ) ) ;
#76913 = VECTOR ( 'NONE', #15230, 1000.000000000000000 ) ;
#76914 = ORIENTED_EDGE ( 'NONE', *, *, #25909, .F. ) ;
#76915 = EDGE_LOOP ( 'NONE', ( #48763, #77786, #9790, #28407 ) ) ;
#76916 = CARTESIAN_POINT ( 'NONE',  ( 21.34481565588190577, 0.7053969147712814136, -2.184679923000765189 ) ) ;
#76917 = EDGE_CURVE ( 'NONE', #75562, #96223, #12666, .T. ) ;
#76918 = ADVANCED_FACE ( 'NONE', ( #51014 ), #71260, .T. ) ;
#76919 = AXIS2_PLACEMENT_3D ( 'NONE', #89216, #68275, #39503 ) ;
#76920 = ORIENTED_EDGE ( 'NONE', *, *, #96847, .T. ) ;
#76921 = FACE_OUTER_BOUND ( 'NONE', #85044, .T. ) ;
#76923 = EDGE_CURVE ( 'NONE', #118375, #73740, #84826, .T. ) ;
#76922 = CARTESIAN_POINT ( 'NONE',  ( 127.5000000000000000, -2.000000000000000000, -1.999999999999998224 ) ) ;
#76924 = CIRCLE ( 'NONE', #53942, 0.1000000000000002554 ) ;
#76925 = EDGE_CURVE ( 'NONE', #117196, #17735, #123487, .T. ) ;
#76926 = CARTESIAN_POINT ( 'NONE',  ( 1.849999999999951017, 12.50000000000000000, -6.148780366869526226 ) ) ;
#76927 = ORIENTED_EDGE ( 'NONE', *, *, #53814, .T. ) ;
#76928 = AXIS2_PLACEMENT_3D ( 'NONE', #35243, #84323, #123596 ) ;
#76929 = FACE_BOUND ( 'NONE', #71653, .T. ) ;
#76930 = EDGE_CURVE ( 'NONE', #51911, #16954, #83784, .T. ) ;
#76932 = EDGE_LOOP ( 'NONE', ( #116397, #86467, #40527, #82805 ) ) ;
#76931 = CARTESIAN_POINT ( 'NONE',  ( 7.049999999999928768, 2.500000000000000000, 6.395190528383296602 ) ) ;
#76933 = DIRECTION ( 'NONE',  ( 0.000000000000000000, 0.000000000000000000, 1.000000000000000000 ) ) ;
#76934 = VECTOR ( 'NONE', #31307, 1000.000000000000000 ) ;
#76935 = FACE_OUTER_BOUND ( 'NONE', #23722, .T. ) ;
#76936 = VERTEX_POINT ( 'NONE', #111857 ) ;
#76937 = EDGE_CURVE ( 'NONE', #107629, #121502, #108903, .T. ) ;
#76940 = EDGE_CURVE ( 'NONE', #2654, #101787, #51655, .T. ) ;
#76939 = CIRCLE ( 'NONE', #3782, 0.1000000000000000472 ) ;
#76938 = AXIS2_PLACEMENT_3D ( 'NONE', #40510, #57046, #7952 ) ;
#76941 = VERTEX_POINT ( 'NONE', #33931 ) ;
#76942 = ORIENTED_EDGE ( 'NONE', *, *, #26549, .T. ) ;
#76943 = PLANE ( 'NONE',  #121517 ) ;
#76944 = DIRECTION ( 'NONE',  ( -4.274815082592931898E-19, -0.9999939076577903929, -0.003490651415223739937 ) ) ;
#76945 =( BOUNDED_CURVE ( )  B_SPLINE_CURVE ( 2, ( #39664, #27881, #49479 ),
 .UNSPECIFIED., .F., .F. ) 
 B_SPLINE_CURVE_WITH_KNOTS ( ( 3, 3 ),
 ( 0.0008083180696977302617, 0.0008883710667521953468 ),
 .UNSPECIFIED. ) 
 CURVE ( )  GEOMETRIC_REPRESENTATION_ITEM ( )  RATIONAL_B_SPLINE_CURVE ( ( 0.9944676636816576210, 0.9972072019273532373, 1.000000000000000000 ) ) 
 REPRESENTATION_ITEM ( '' )  );
#76946 = LINE ( 'NONE', #19291, #83966 ) ;
#76947 = FACE_BOUND ( 'NONE', #5896, .T. ) ;
#76948 = ORIENTED_EDGE ( 'NONE', *, *, #112115, .F. ) ;
#76949 = CARTESIAN_POINT ( 'NONE',  ( 1.849999999999950573, 12.50000000000000000, 2.511473670974873507 ) ) ;
#76950 = PLANE ( 'NONE',  #116982 ) ;
#76951 = DIRECTION ( 'NONE',  ( -0.000000000000000000, 1.000000000000000000, -0.000000000000000000 ) ) ;
#76952 = DIRECTION ( 'NONE',  ( -0.000000000000000000, -1.000000000000000000, -0.000000000000000000 ) ) ;
#76953 = FACE_OUTER_BOUND ( 'NONE', #50449, .T. ) ;
#76954 = LINE ( 'NONE', #35741, #122358 ) ;
#76955 = CARTESIAN_POINT ( 'NONE',  ( 9.399999999999915090, 12.50000000000000000, -3.918623584224389056 ) ) ;
#76956 = ORIENTED_EDGE ( 'NONE', *, *, #125765, .F. ) ;
#76957 = ORIENTED_EDGE ( 'NONE', *, *, #71993, .T. ) ;
#76958 = EDGE_LOOP ( 'NONE', ( #107001, #33238, #89556, #68532 ) ) ;
#76959 = AXIS2_PLACEMENT_3D ( 'NONE', #47214, #51089, #101465 ) ;
#76960 = CIRCLE ( 'NONE', #91622, 0.1000000000000000472 ) ;
#76961 = VERTEX_POINT ( 'NONE', #21535 ) ;
#76962 = EDGE_LOOP ( 'NONE', ( #100300, #46988 ) ) ;
#76963 = CARTESIAN_POINT ( 'NONE',  ( 0.5999999999999612310, 2.500000000000000000, -0.4464101615137760493 ) ) ;
#76964 = AXIS2_PLACEMENT_3D ( 'NONE', #59457, #49628, #107235 ) ;
#76965 = PLANE ( 'NONE',  #6955 ) ;
#76966 = ORIENTED_EDGE ( 'NONE', *, *, #83456, .F. ) ;
#76967 = FACE_BOUND ( 'NONE', #99618, .T. ) ;
#76968 = DIRECTION ( 'NONE',  ( -0.000000000000000000, -1.000000000000000000, -0.000000000000000000 ) ) ;
#76969 = CIRCLE ( 'NONE', #22612, 0.1000000000000002554 ) ;
#76970 = AXIS2_PLACEMENT_3D ( 'NONE', #13572, #52233, #21476 ) ;
#76971 = DIRECTION ( 'NONE',  ( -4.274815082592931898E-19, -0.9999939076577903929, -0.003490651415223739937 ) ) ;
#76972 = DIRECTION ( 'NONE',  ( 0.000000000000000000, 0.000000000000000000, -1.000000000000000000 ) ) ;
#76973 = DIRECTION ( 'NONE',  ( 0.000000000000000000, 1.000000000000000000, 0.000000000000000000 ) ) ;
#76974 = DIRECTION ( 'NONE',  ( 0.000000000000000000, 1.000000000000000000, 0.000000000000000000 ) ) ;
#76975 = ORIENTED_EDGE ( 'NONE', *, *, #89005, .F. ) ;
#76976 = DIRECTION ( 'NONE',  ( -0.000000000000000000, 1.000000000000000000, -0.000000000000000000 ) ) ;
#76977 = VERTEX_POINT ( 'NONE', #122961 ) ;
#76978 = EDGE_CURVE ( 'NONE', #118395, #67119, #91563, .T. ) ;
#76979 = AXIS2_PLACEMENT_3D ( 'NONE', #28802, #68708, #108633 ) ;
#76980 = ORIENTED_EDGE ( 'NONE', *, *, #75394, .F. ) ;
#76981 = ORIENTED_EDGE ( 'NONE', *, *, #58926, .T. ) ;
#76982 = DIRECTION ( 'NONE',  ( -0.000000000000000000, 1.000000000000000000, -0.000000000000000000 ) ) ;
#76983 = CARTESIAN_POINT ( 'NONE',  ( 13.12246079422102341, 2.499999999999999112, 7.156134183588167552 ) ) ;
#76984 = DIRECTION ( 'NONE',  ( -0.000000000000000000, 1.000000000000000000, -0.000000000000000000 ) ) ;
#76985 = ORIENTED_EDGE ( 'NONE', *, *, #62963, .F. ) ;
#76986 = CARTESIAN_POINT ( 'NONE',  ( 16.56576425165006228, 2.499999999999999556, -6.084390597445810123 ) ) ;
#76987 = CIRCLE ( 'NONE', #20559, 0.06509327318403745899 ) ;
#76988 = CARTESIAN_POINT ( 'NONE',  ( -1.322875655532295136, -1.500000000000000222, 6.000000000000005329 ) ) ;
#76989 = CARTESIAN_POINT ( 'NONE',  ( 3.749999999999942268, 12.50000000000000000, -1.472243186433550122 ) ) ;
#76990 = CARTESIAN_POINT ( 'NONE',  ( 186.5677083336747160, -4.367472073101514418, -7.564683531250002702 ) ) ;
#76991 = CARTESIAN_POINT ( 'NONE',  ( -4.600000000000024514, 12.50000000000000000, 4.957854068765711553 ) ) ;
#76992 = CARTESIAN_POINT ( 'NONE',  ( 15.39999999999989022, 12.50000000000000000, 0.06509327318403504425 ) ) ;
#76993 = CIRCLE ( 'NONE', #72793, 0.06509327318403745899 ) ;
#76994 = FACE_OUTER_BOUND ( 'NONE', #27436, .T. ) ;
#76995 = ORIENTED_EDGE ( 'NONE', *, *, #3542, .F. ) ;
#76996 = DIRECTION ( 'NONE',  ( 0.000000000000000000, 0.000000000000000000, 1.000000000000000000 ) ) ;
#76997 = CIRCLE ( 'NONE', #127188, 0.06509327318403745899 ) ;
#76998 = VERTEX_POINT ( 'NONE', #81112 ) ;
#76999 = ORIENTED_EDGE ( 'NONE', *, *, #45037, .T. ) ;
#77000 = COLOUR_RGB ( '', 0.66274510, 0.83137255, 0.94901961) ;
#77001 = CARTESIAN_POINT ( 'NONE',  ( -7.100000000000017408, 2.500000000000000000, -5.022947341949754119 ) ) ;
#77002 = CARTESIAN_POINT ( 'NONE',  ( 1.849999999999950573, 2.500000000000000000, 2.511473670974873507 ) ) ;
#77003 = CARTESIAN_POINT ( 'NONE',  ( -4.150000000000024336, 2.500000000000000000, 1.372243186433545370 ) ) ;
#77004 = ORIENTED_EDGE ( 'NONE', *, *, #35316, .F. ) ;
#77005 = CONICAL_SURFACE ( 'NONE', #83279, 0.09999999999999982514, 0.003490658503988666988 ) ;
#77006 = ORIENTED_EDGE ( 'NONE', *, *, #115091, .T. ) ;
#77007 = CARTESIAN_POINT ( 'NONE',  ( 11.84999999999990372, 2.500000000000000000, -6.148780366869526226 ) ) ;
#77008 = AXIS2_PLACEMENT_3D ( 'NONE', #112018, #21046, #72100 ) ;
#77009 = DIRECTION ( 'NONE',  ( -0.000000000000000000, 1.000000000000000000, -0.000000000000000000 ) ) ;
#77010 = DIRECTION ( 'NONE',  ( 0.000000000000000000, 1.000000000000000000, 0.000000000000000000 ) ) ;
#77011 = ORIENTED_EDGE ( 'NONE', *, *, #9097, .F. ) ;
#77012 = ORIENTED_EDGE ( 'NONE', *, *, #41648, .T. ) ;
#77013 = LINE ( 'NONE', #37741, #6337 ) ;
#77014 = AXIS2_PLACEMENT_3D ( 'NONE', #35457, #104806, #96930 ) ;
#77015 = VERTEX_POINT ( 'NONE', #121022 ) ;
#77016 = FACE_OUTER_BOUND ( 'NONE', #116434, .T. ) ;
#77017 = EDGE_CURVE ( 'NONE', #104132, #73436, #4336, .T. ) ;
#77018 = CARTESIAN_POINT ( 'NONE',  ( 3.349999999999943689, 12.50000000000000000, 1.472243186433545459 ) ) ;
#77019 = ORIENTED_EDGE ( 'NONE', *, *, #67291, .F. ) ;
#77020 = DIRECTION ( 'NONE',  ( -0.000000000000000000, 1.000000000000000000, -0.000000000000000000 ) ) ;
#77021 = CARTESIAN_POINT ( 'NONE',  ( 11.84999999999990372, 12.50000000000000000, 2.511473670974873507 ) ) ;
#77022 = LINE ( 'NONE', #17436, #115745 ) ;
#77023 = CIRCLE ( 'NONE', #20592, 0.09999999999999982514 ) ;
#77024 = EDGE_CURVE ( 'NONE', #38979, #26349, #104701, .T. ) ;
#77025 = DIRECTION ( 'NONE',  ( -4.274815082592931898E-19, -0.9999939076577903929, -0.003490651415223739937 ) ) ;
#77026 = EDGE_CURVE ( 'NONE', #39885, #127091, #21084, .T. ) ;
#77027 = VERTEX_POINT ( 'NONE', #52929 ) ;
#77028 = DIRECTION ( 'NONE',  ( 0.000000000000000000, 0.000000000000000000, -1.000000000000000000 ) ) ;
#77030 = AXIS2_PLACEMENT_3D ( 'NONE', #65304, #67895, #45693 ) ;
#77029 = CONICAL_SURFACE ( 'NONE', #29019, 0.1000000000000000472, 0.003490658503988666988 ) ;
#77031 = DIRECTION ( 'NONE',  ( -0.000000000000000000, -1.000000000000000000, -0.000000000000000000 ) ) ;
#77032 = ADVANCED_FACE ( 'NONE', ( #113788 ), #58756, .T. ) ;
#77033 = VERTEX_POINT ( 'NONE', #13632 ) ;
#77034 = EDGE_CURVE ( 'NONE', #62185, #15358, #121432, .T. ) ;
#77035 = ORIENTED_EDGE ( 'NONE', *, *, #104223, .F. ) ;
#77036 = EDGE_CURVE ( 'NONE', #128073, #78150, #32673, .T. ) ;
#77037 = CARTESIAN_POINT ( 'NONE',  ( 185.7968750003414300, 8.734944146203032389, 5.348610694689227483E-16 ) ) ;
#77039 = EDGE_CURVE ( 'NONE', #36055, #54722, #2294, .T. ) ;
#77038 = DIRECTION ( 'NONE',  ( 0.000000000000000000, 1.000000000000000000, 0.000000000000000000 ) ) ;
#77040 = DIRECTION ( 'NONE',  ( 0.000000000000000000, -0.000000000000000000, 1.000000000000000000 ) ) ;
#77041 = EDGE_CURVE ( 'NONE', #29442, #67610, #52474, .T. ) ;
#77042 = LINE ( 'NONE', #126134, #43876 ) ;
#77043 = DIRECTION ( 'NONE',  ( -4.274815082592931898E-19, -0.9999939076577903929, -0.003490651415223739937 ) ) ;
#77044 = DIRECTION ( 'NONE',  ( -0.000000000000000000, -1.000000000000000000, -0.000000000000000000 ) ) ;
#77045 = FACE_OUTER_BOUND ( 'NONE', #25788, .T. ) ;
#77046 = CARTESIAN_POINT ( 'NONE',  ( 8.549999999999920774, 2.500000000000000000, 6.148780366869520897 ) ) ;
#77047 = DIRECTION ( 'NONE',  ( 0.000000000000000000, 0.000000000000000000, 1.000000000000000000 ) ) ;
#77048 = AXIS2_PLACEMENT_3D ( 'NONE', #11259, #92397, #81304 ) ;
#77049 = ADVANCED_FACE ( 'NONE', ( #126175 ), #123576, .T. ) ;
#77050 = FACE_OUTER_BOUND ( 'NONE', #3143, .T. ) ;
#77051 = CIRCLE ( 'NONE', #37352, 0.06509327318403745899 ) ;
#77052 = VECTOR ( 'NONE', #110207, 1000.000000000000000 ) ;
#77053 = VERTEX_POINT ( 'NONE', #16827 ) ;
#77054 = CIRCLE ( 'NONE', #108433, 0.06509327318403745899 ) ;
#77055 = DIRECTION ( 'NONE',  ( 0.000000000000000000, 0.000000000000000000, 1.000000000000000000 ) ) ;
#77056 = CARTESIAN_POINT ( 'NONE',  ( 8.149999999999920419, 2.500000000000000000, -1.918653347947325782 ) ) ;
#77057 = CARTESIAN_POINT ( 'NONE',  ( 2.049999999999950084, 2.500000000000000000, -2.265063509461101798 ) ) ;
#77058 = CARTESIAN_POINT ( 'NONE',  ( -5.850000000000018296, 12.50000000000000000, 2.857883832488649301 ) ) ;
#77059 = CONICAL_SURFACE ( 'NONE', #5926, 0.09999999999999982514, 0.003490658503988666988 ) ;
#77060 = ORIENTED_EDGE ( 'NONE', *, *, #55883, .T. ) ;
#77061 = AXIS2_PLACEMENT_3D ( 'NONE', #126447, #36783, #76692 ) ;
#77062 = DIRECTION ( 'NONE',  ( 0.000000000000000000, 1.000000000000000000, 0.000000000000000000 ) ) ;
#77063 = AXIS2_PLACEMENT_3D ( 'NONE', #9571, #80252, #87466 ) ;
#77064 = CIRCLE ( 'NONE', #47832, 0.06509327318403745899 ) ;
#77065 = DIRECTION ( 'NONE',  ( 0.000000000000000000, 1.000000000000000000, 0.000000000000000000 ) ) ;
#77067 = VERTEX_POINT ( 'NONE', #75774 ) ;
#77066 = CARTESIAN_POINT ( 'NONE',  ( 8.349999999999923261, 12.50000000000000000, -7.188010851410854052 ) ) ;
#77068 = AXIS2_PLACEMENT_3D ( 'NONE', #108952, #29146, #116848 ) ;
#77069 = ORIENTED_EDGE ( 'NONE', *, *, #25911, .T. ) ;
#77070 = CONICAL_SURFACE ( 'NONE', #37377, 0.1000000000000002554, 0.003490658503988666988 ) ;
#77071 = ORIENTED_EDGE ( 'NONE', *, *, #19772, .F. ) ;
#77072 = ORIENTED_EDGE ( 'NONE', *, *, #122180, .T. ) ;
#77073 = VERTEX_POINT ( 'NONE', #96065 ) ;
#77074 = DIRECTION ( 'NONE',  ( 0.000000000000000000, 0.000000000000000000, 1.000000000000000000 ) ) ;
#77075 = EDGE_CURVE ( 'NONE', #31468, #53805, #52577, .T. ) ;
#77076 = CARTESIAN_POINT ( 'NONE',  ( -1.650000000000035216, 2.500000000000000000, -5.802370205355749988 ) ) ;
#77078 = EDGE_CURVE ( 'NONE', #58403, #38961, #46222, .T. ) ;
#77077 = FACE_OUTER_BOUND ( 'NONE', #123066, .T. ) ;
#77079 = CARTESIAN_POINT ( 'NONE',  ( -13.94999999999998863, 2.500000000000000000, -1.918653347947324006 ) ) ;
#77080 = CIRCLE ( 'NONE', #79235, 0.1000000000000002554 ) ;
#77081 = ORIENTED_EDGE ( 'NONE', *, *, #120506, .F. ) ;
#77082 = ADVANCED_FACE ( 'NONE', ( #24762 ), #69286, .T. ) ;
#77083 = FACE_OUTER_BOUND ( 'NONE', #103152, .T. ) ;
#77084 = ORIENTED_EDGE ( 'NONE', *, *, #112938, .F. ) ;
#77085 = AXIS2_PLACEMENT_3D ( 'NONE', #110688, #91705, #12490 ) ;
#77086 = CARTESIAN_POINT ( 'NONE',  ( 76.45351065619851738, -3.568406926262015944, -6.085611129014742993 ) ) ;
#77087 = DIRECTION ( 'NONE',  ( 0.000000000000000000, 1.000000000000000000, 0.000000000000000000 ) ) ;
#77088 = CARTESIAN_POINT ( 'NONE',  ( 4.999999999999971578, 2.500000000000000000, 0.09999999999999772959 ) ) ;
#77089 = CARTESIAN_POINT ( 'NONE',  ( 21.23528140090950700, -2.699413673072311948, 2.293764360948884473 ) ) ;
#77090 = ADVANCED_FACE ( 'NONE', ( #77077 ), #10694, .T. ) ;
#77091 = EDGE_CURVE ( 'NONE', #72485, #117365, #14886, .T. ) ;
#77092 = EDGE_LOOP ( 'NONE', ( #60387, #123249, #46225, #20097 ) ) ;
#77093 = EDGE_CURVE ( 'NONE', #25527, #122087, #35856, .T. ) ;
#77094 = ADVANCED_FACE ( 'NONE', ( #36527 ), #54221, .T. ) ;
#77095 = ORIENTED_EDGE ( 'NONE', *, *, #111776, .F. ) ;
#77096 = ORIENTED_EDGE ( 'NONE', *, *, #42936, .T. ) ;
#77097 = ORIENTED_EDGE ( 'NONE', *, *, #127317, .T. ) ;
#77098 = DIRECTION ( 'NONE',  ( 0.000000000000000000, 1.000000000000000000, 0.000000000000000000 ) ) ;
#77099 = CARTESIAN_POINT ( 'NONE',  ( 1.649999999999949729, 2.500000000000000000, 7.288010851410849256 ) ) ;
#77100 = FACE_OUTER_BOUND ( 'NONE', #81189, .T. ) ;
#77101 = FACE_BOUND ( 'NONE', #64440, .T. ) ;
#77102 = LINE ( 'NONE', #35255, #15909 ) ;
#77103 = DIRECTION ( 'NONE',  ( 0.000000000000000000, 0.000000000000000000, 1.000000000000000000 ) ) ;
#77104 = AXIS2_PLACEMENT_3D ( 'NONE', #128570, #38902, #78812 ) ;
#77105 = EDGE_CURVE ( 'NONE', #53767, #76087, #29589, .T. ) ;
#77106 = FACE_OUTER_BOUND ( 'NONE', #119344, .T. ) ;
#77107 = LINE ( 'NONE', #28003, #70944 ) ;
#77108 = CARTESIAN_POINT ( 'NONE',  ( 184.4218750003414016, 0.000000000000000000, 7.564683531250000925 ) ) ;
#77109 = DIRECTION ( 'NONE',  ( 0.000000000000000000, 0.000000000000000000, 1.000000000000000000 ) ) ;
#77110 = CIRCLE ( 'NONE', #104297, 0.06509327318403745899 ) ;
#77111 = CARTESIAN_POINT ( 'NONE',  ( -11.64999999999999680, 12.50000000000000000, 7.188010851410848723 ) ) ;
#77112 = DIRECTION ( 'NONE',  ( -0.000000000000000000, 1.000000000000000000, -0.000000000000000000 ) ) ;
#77113 = CONICAL_SURFACE ( 'NONE', #52082, 0.1000000000000000472, 0.003490658503988666988 ) ;
#77114 = ORIENTED_EDGE ( 'NONE', *, *, #28397, .F. ) ;
#77115 = ORIENTED_EDGE ( 'NONE', *, *, #12042, .T. ) ;
#77116 = ORIENTED_EDGE ( 'NONE', *, *, #33180, .F. ) ;
#77117 = EDGE_LOOP ( 'NONE', ( #61527, #92922, #9084, #14465 ) ) ;
#77118 = AXIS2_PLACEMENT_3D ( 'NONE', #95321, #24646, #44936 ) ;
#77119 = DIRECTION ( 'NONE',  ( 0.000000000000000000, 1.000000000000000000, 0.000000000000000000 ) ) ;
#77120 = ADVANCED_FACE ( 'NONE', ( #84957 ), #124890, .T. ) ;
#77121 = FACE_BOUND ( 'NONE', #8820, .T. ) ;
#77122 = CARTESIAN_POINT ( 'NONE',  ( -7.500000000000016875, 12.50000000000000000, 0.6928203230275494784 ) ) ;
#77123 = DIRECTION ( 'NONE',  ( 0.000000000000000000, 1.000000000000000000, 0.000000000000000000 ) ) ;
#77125 = VECTOR ( 'NONE', #3036, 1000.000000000000000 ) ;
#77124 = AXIS2_PLACEMENT_3D ( 'NONE', #92825, #73805, #24077 ) ;
#77126 = ORIENTED_EDGE ( 'NONE', *, *, #107776, .F. ) ;
#77127 = DIRECTION ( 'NONE',  ( -0.000000000000000000, -1.000000000000000000, -0.000000000000000000 ) ) ;
#77128 = DIRECTION ( 'NONE',  ( 0.000000000000000000, 1.000000000000000000, 0.000000000000000000 ) ) ;
#77129 = ORIENTED_EDGE ( 'NONE', *, *, #76044, .F. ) ;
#77130 = CARTESIAN_POINT ( 'NONE',  ( 12.89999999999990266, 2.500000000000000000, -5.122947341949753763 ) ) ;
#77131 = DIRECTION ( 'NONE',  ( -0.000000000000000000, -1.000000000000000000, -0.000000000000000000 ) ) ;
#77132 = EDGE_CURVE ( 'NONE', #123357, #56703, #75550, .T. ) ;
#77133 = ORIENTED_EDGE ( 'NONE', *, *, #53991, .T. ) ;
#77134 = AXIS2_PLACEMENT_3D ( 'NONE', #2253, #62500, #98681 ) ;
#77135 = CARTESIAN_POINT ( 'NONE',  ( -7.499999999999976907, 12.50000000000000000, 4.330127018922196314 ) ) ;
#77136 = CARTESIAN_POINT ( 'NONE',  ( 3.349999999999944578, 2.500000000000000000, -1.372243186433550033 ) ) ;
#77137 = EDGE_LOOP ( 'NONE', ( #126305, #4900, #110934, #72087 ) ) ;
#77138 = CIRCLE ( 'NONE', #68724, 0.1000000000000000472 ) ;
#77139 = CARTESIAN_POINT ( 'NONE',  ( 9.399999999999915090, 2.500000000000000000, -4.676537180435977881 ) ) ;
#77140 = VECTOR ( 'NONE', #50322, 1000.000000000000000 ) ;
#77141 = DIRECTION ( 'NONE',  ( 0.000000000000000000, 0.000000000000000000, 1.000000000000000000 ) ) ;
#77142 = ORIENTED_EDGE ( 'NONE', *, *, #114763, .F. ) ;
#77143 = PLANE ( 'NONE',  #93273 ) ;
#77144 = ORIENTED_EDGE ( 'NONE', *, *, #81081, .T. ) ;
#77145 = ORIENTED_EDGE ( 'NONE', *, *, #71021, .T. ) ;
#77146 = EDGE_CURVE ( 'NONE', #44219, #38932, #106528, .T. ) ;
#77147 = CARTESIAN_POINT ( 'NONE',  ( 7.899999999999924860, 2.500000000000000000, 3.637306695894644726 ) ) ;
#77148 = EDGE_LOOP ( 'NONE', ( #115038, #111109 ) ) ;
#77149 = DIRECTION ( 'NONE',  ( 0.000000000000000000, 1.000000000000000000, 0.000000000000000000 ) ) ;
#77150 = FACE_BOUND ( 'NONE', #61922, .T. ) ;
#77151 = CONICAL_SURFACE ( 'NONE', #54176, 0.09999999999999982514, 0.003490658503988666988 ) ;
#77152 = VECTOR ( 'NONE', #126435, 1000.000000000000000 ) ;
#77153 = VERTEX_POINT ( 'NONE', #46985 ) ;
#77154 = LINE ( 'NONE', #94860, #45528 ) ;
#77155 = VERTEX_POINT ( 'NONE', #65961 ) ;
#77156 = CARTESIAN_POINT ( 'NONE',  ( -4.150000000000025224, 2.500000000000000000, 2.957883832488649389 ) ) ;
#77157 = DIRECTION ( 'NONE',  ( 0.000000000000000000, 1.000000000000000000, 0.000000000000000000 ) ) ;
#77158 = DIRECTION ( 'NONE',  ( 0.000000000000000000, 0.000000000000000000, 1.000000000000000000 ) ) ;
#77159 = DIRECTION ( 'NONE',  ( 0.000000000000000000, -0.9999939076577903929, 0.003490651415223739937 ) ) ;
#77160 = CARTESIAN_POINT ( 'NONE',  ( 7.099999999999926814, 2.500000000000000000, -0.1000000000000022815 ) ) ;
#77161 = CIRCLE ( 'NONE', #75109, 0.06509327318403745899 ) ;
#77162 = ORIENTED_EDGE ( 'NONE', *, *, #20632, .F. ) ;
#77164 = VERTEX_POINT ( 'NONE', #86886 ) ;
#77163 = AXIS2_PLACEMENT_3D ( 'NONE', #112481, #30714, #110534 ) ;
#77165 = DIRECTION ( 'NONE',  ( -0.000000000000000000, 1.000000000000000000, -0.000000000000000000 ) ) ;
#77166 = DIRECTION ( 'NONE',  ( 0.000000000000000000, 1.000000000000000000, 0.000000000000000000 ) ) ;
#77167 = FACE_OUTER_BOUND ( 'NONE', #117568, .T. ) ;
#77169 = ORIENTED_EDGE ( 'NONE', *, *, #31744, .T. ) ;
#77168 = ORIENTED_EDGE ( 'NONE', *, *, #4218, .T. ) ;
#77170 = ORIENTED_EDGE ( 'NONE', *, *, #40470, .T. ) ;
#77171 = CARTESIAN_POINT ( 'NONE',  ( -5.450000000000019718, 2.500000000000000000, 6.395190528383296602 ) ) ;
#77172 = DIRECTION ( 'NONE',  ( -4.274815082592931898E-19, -0.9999939076577903929, -0.003490651415223739937 ) ) ;
#77173 = LINE ( 'NONE', #112284, #5976 ) ;
#77174 = EDGE_CURVE ( 'NONE', #28403, #31157, #54841, .T. ) ;
#77175 = SHAPE_DEFINITION_REPRESENTATION ( #87007, #125483 ) ;
#77176 = DIRECTION ( 'NONE',  ( 0.000000000000000000, 0.000000000000000000, 1.000000000000000000 ) ) ;
#77177 = CARTESIAN_POINT ( 'NONE',  ( -12.69999999999999396, 2.500000000000000000, 0.4464101615137776591 ) ) ;
#77178 = DIRECTION ( 'NONE',  ( -0.000000000000000000, 1.000000000000000000, -0.000000000000000000 ) ) ;
#77179 = DIRECTION ( 'NONE',  ( -0.000000000000000000, 1.000000000000000000, -0.000000000000000000 ) ) ;
#77180 = CIRCLE ( 'NONE', #127361, 0.06509327318403745899 ) ;
#77181 = DIRECTION ( 'NONE',  ( -0.000000000000000000, 1.000000000000000000, -0.000000000000000000 ) ) ;
#77182 = DIRECTION ( 'NONE',  ( 0.000000000000000000, 1.000000000000000000, 0.000000000000000000 ) ) ;
#77183 = ADVANCED_FACE ( 'NONE', ( #94782 ), #75146, .T. ) ;
#77184 = VERTEX_POINT ( 'NONE', #55508 ) ;
#77185 = VERTEX_POINT ( 'NONE', #67214 ) ;
#77186 = PLANE ( 'NONE',  #65363 ) ;
#77187 = EDGE_CURVE ( 'NONE', #83854, #6221, #97356, .T. ) ;
#77188 = ORIENTED_EDGE ( 'NONE', *, *, #95663, .T. ) ;
#77189 = ADVANCED_FACE ( 'NONE', ( #109764 ), #39114, .T. ) ;
#77190 = ORIENTED_EDGE ( 'NONE', *, *, #65340, .T. ) ;
#77191 = EDGE_CURVE ( 'NONE', #67175, #63506, #8322, .T. ) ;
#77192 = DIRECTION ( 'NONE',  ( 0.000000000000000000, 0.000000000000000000, 1.000000000000000000 ) ) ;
#77194 = ADVANCED_FACE ( 'NONE', ( #29276 ), #17491, .T. ) ;
#77193 = CARTESIAN_POINT ( 'NONE',  ( 97.50000000000000000, 0.000000000000000000, 0.000000000000000000 ) ) ;
#77195 = AXIS2_PLACEMENT_3D ( 'NONE', #37439, #77349, #117239 ) ;
#77196 = LINE ( 'NONE', #117094, #67542 ) ;
#77197 = CARTESIAN_POINT ( 'NONE',  ( 195.0000000000000000, 0.000000000000000000, 0.000000000000000000 ) ) ;
#77198 = LINE ( 'NONE', #115824, #2607 ) ;
#77199 = CARTESIAN_POINT ( 'NONE',  ( 10.79999999999991012, 2.500000000000000000, -4.330127018922201643 ) ) ;
#77200 = DIRECTION ( 'NONE',  ( 0.000000000000000000, 0.000000000000000000, -1.000000000000000000 ) ) ;
#77201 = ORIENTED_EDGE ( 'NONE', *, *, #21058, .T. ) ;
#77202 = DIRECTION ( 'NONE',  ( -4.274815082592931898E-19, -0.9999939076577903929, -0.003490651415223739937 ) ) ;
#77203 = ADVANCED_FACE ( 'NONE', ( #57441 ), #8963, .T. ) ;
#77205 = EDGE_CURVE ( 'NONE', #58364, #88434, #12840, .T. ) ;
#77204 = DIRECTION ( 'NONE',  ( -0.000000000000000000, -1.000000000000000000, -0.000000000000000000 ) ) ;
#77206 = EDGE_CURVE ( 'NONE', #112593, #10182, #33705, .T. ) ;
#77207 = ORIENTED_EDGE ( 'NONE', *, *, #69047, .T. ) ;
#77209 = CIRCLE ( 'NONE', #93934, 0.1000000000000002554 ) ;
#77208 = CIRCLE ( 'NONE', #14480, 0.1000000000000000472 ) ;
#77210 = ORIENTED_EDGE ( 'NONE', *, *, #34808, .F. ) ;
#77211 = AXIS2_PLACEMENT_3D ( 'NONE', #14008, #53955, #122059 ) ;
#77212 = ORIENTED_EDGE ( 'NONE', *, *, #116223, .T. ) ;
#77213 = EDGE_LOOP ( 'NONE', ( #116592, #84251 ) ) ;
#77214 = DIRECTION ( 'NONE',  ( -0.000000000000000000, 1.000000000000000000, -0.000000000000000000 ) ) ;
#77215 = CARTESIAN_POINT ( 'NONE',  ( 5.649999999999934630, 2.500000000000000000, 6.841600689897072485 ) ) ;
#77218 = VERTEX_POINT ( 'NONE', #47621 ) ;
#77217 = AXIS2_PLACEMENT_3D ( 'NONE', #62606, #54676, #81581 ) ;
#77216 = VECTOR ( 'NONE', #97324, 1000.000000000000000 ) ;
#77219 = DIRECTION ( 'NONE',  ( 0.000000000000000000, 0.000000000000000000, -1.000000000000000000 ) ) ;
#77220 = CARTESIAN_POINT ( 'NONE',  ( 17.50000000000000000, 2.749999999999999556, -9.999999999999998224 ) ) ;
#77221 = CARTESIAN_POINT ( 'NONE',  ( -9.150000000000005684, 12.50000000000000000, 7.253104124594885960 ) ) ;
#77222 = ORIENTED_EDGE ( 'NONE', *, *, #106424, .F. ) ;
#77223 = DIRECTION ( 'NONE',  ( 0.000000000000000000, 0.000000000000000000, 1.000000000000000000 ) ) ;
#77224 = DIRECTION ( 'NONE',  ( -0.000000000000000000, -1.000000000000000000, -0.000000000000000000 ) ) ;
#77225 = VERTEX_POINT ( 'NONE', #28630 ) ;
#77226 = EDGE_LOOP ( 'NONE', ( #119622, #41907, #107734, #64328 ) ) ;
#77227 = ORIENTED_EDGE ( 'NONE', *, *, #21441, .T. ) ;
#77228 = CARTESIAN_POINT ( 'NONE',  ( 12.93920187831545299, -1.499999999999998446, 10.00000000000000178 ) ) ;
#77229 = CARTESIAN_POINT ( 'NONE',  ( 1.649999999999951505, 2.500000000000000000, -1.572243186433550211 ) ) ;
#77230 = CONICAL_SURFACE ( 'NONE', #66847, 0.1000000000000002554, 0.003490658503988666988 ) ;
#77231 = VECTOR ( 'NONE', #46286, 1000.000000000000000 ) ;
#77232 = ORIENTED_EDGE ( 'NONE', *, *, #15703, .F. ) ;
#77233 = PLANE ( 'NONE',  #11942 ) ;
#77234 = CARTESIAN_POINT ( 'NONE',  ( -6.250000000000017764, 12.50000000000000000, 2.857883832488649301 ) ) ;
#77235 = DIRECTION ( 'NONE',  ( 0.000000000000000000, 0.000000000000000000, -1.000000000000000000 ) ) ;
#77236 = CARTESIAN_POINT ( 'NONE',  ( -5.000000000000026645, 2.500000000000000000, -3.637306695894650055 ) ) ;
#77237 = EDGE_CURVE ( 'NONE', #104608, #75247, #29508, .T. ) ;
#77238 = AXIS2_PLACEMENT_3D ( 'NONE', #127138, #126485, #86548 ) ;
#77239 = CONICAL_SURFACE ( 'NONE', #62587, 0.1000000000000002554, 0.003490658503988666988 ) ;
#77240 = EDGE_CURVE ( 'NONE', #13780, #100057, #99302, .T. ) ;
#77241 = ORIENTED_EDGE ( 'NONE', *, *, #19986, .F. ) ;
#77242 = AXIS2_PLACEMENT_3D ( 'NONE', #102749, #43863, #81199 ) ;
#77243 = CARTESIAN_POINT ( 'NONE',  ( 12.09999999999990550, 2.500000000000000000, -4.430127018922202176 ) ) ;
#77244 = ADVANCED_FACE ( 'NONE', ( #118932 ), #6475, .T. ) ;
#77245 = ORIENTED_EDGE ( 'NONE', *, *, #101497, .F. ) ;
#77246 = EDGE_LOOP ( 'NONE', ( #120721, #29660 ) ) ;
#77247 = CARTESIAN_POINT ( 'NONE',  ( 3.149999999999946176, 12.50000000000000000, -6.841600689897077814 ) ) ;
#77248 = VERTEX_POINT ( 'NONE', #48256 ) ;
#77249 = CARTESIAN_POINT ( 'NONE',  ( 4.999999999999935163, 2.500000000000000000, 0.5928203230275495006 ) ) ;
#77250 = FACE_BOUND ( 'NONE', #70593, .T. ) ;
#77251 = VECTOR ( 'NONE', #104777, 1000.000000000000000 ) ;
#77252 = DIRECTION ( 'NONE',  ( 0.000000000000000000, 0.000000000000000000, 1.000000000000000000 ) ) ;
#77253 = CARTESIAN_POINT ( 'NONE',  ( -3.150000000000032330, 12.50000000000000000, -6.148780366869526226 ) ) ;
#77254 = EDGE_CURVE ( 'NONE', #28344, #102426, #106846, .T. ) ;
#77255 = DIRECTION ( 'NONE',  ( 0.000000000000000000, 0.000000000000000000, -1.000000000000000000 ) ) ;
#77256 = CIRCLE ( 'NONE', #79332, 0.06509327318403745899 ) ;
#77257 = AXIS2_PLACEMENT_3D ( 'NONE', #78718, #78052, #49258 ) ;
#77258 = ORIENTED_EDGE ( 'NONE', *, *, #38222, .F. ) ;
#77259 = DIRECTION ( 'NONE',  ( 0.000000000000000000, -0.9999939076577903929, 0.003490651415223739937 ) ) ;
#77260 = FACE_OUTER_BOUND ( 'NONE', #41036, .T. ) ;
#77261 = CARTESIAN_POINT ( 'NONE',  ( 6.849999999999929479, 2.500000000000000000, -2.611473670974877592 ) ) ;
#77262 = CARTESIAN_POINT ( 'NONE',  ( 12.94999999999990337, 2.500000000000000000, 2.265063509461097357 ) ) ;
#77263 = ORIENTED_EDGE ( 'NONE', *, *, #112585, .T. ) ;
#77264 = DIRECTION ( 'NONE',  ( 0.000000000000000000, 1.000000000000000000, 0.000000000000000000 ) ) ;
#77265 = DIRECTION ( 'NONE',  ( -4.274815082592931898E-19, -0.9999939076577903929, -0.003490651415223739937 ) ) ;
#77266 = AXIS2_PLACEMENT_3D ( 'NONE', #53815, #21799, #93749 ) ;
#77267 = ORIENTED_EDGE ( 'NONE', *, *, #6202, .F. ) ;
#77268 = DIRECTION ( 'NONE',  ( 0.000000000000000000, 0.000000000000000000, -1.000000000000000000 ) ) ;
#77269 = DIRECTION ( 'NONE',  ( 0.000000000000000000, 1.000000000000000000, 0.000000000000000000 ) ) ;
#77270 = EDGE_CURVE ( 'NONE', #42494, #43342, #44166, .T. ) ;
#77271 = FACE_BOUND ( 'NONE', #107243, .T. ) ;
#77272 = CARTESIAN_POINT ( 'NONE',  ( -15.59999999999998010, 2.500000000000000000, 0.2464101615137759549 ) ) ;
#77273 = ORIENTED_EDGE ( 'NONE', *, *, #74083, .F. ) ;
#77274 = DIRECTION ( 'NONE',  ( 0.000000000000000000, 0.000000000000000000, 1.000000000000000000 ) ) ;
#77275 = ORIENTED_EDGE ( 'NONE', *, *, #47964, .F. ) ;
#77276 = ORIENTED_EDGE ( 'NONE', *, *, #29246, .F. ) ;
#77277 = CARTESIAN_POINT ( 'NONE',  ( 11.64999999999990443, 2.500000000000000000, -5.802370205355749988 ) ) ;
#77278 = CARTESIAN_POINT ( 'NONE',  ( 187.3750000000000000, 8.891194145520236347, 5.444286225454521982E-16 ) ) ;
#77279 = ORIENTED_EDGE ( 'NONE', *, *, #118124, .F. ) ;
#77280 = CARTESIAN_POINT ( 'NONE',  ( 11.84999999999990727, 2.500000000000000000, -1.718653347947326049 ) ) ;
#77281 = CARTESIAN_POINT ( 'NONE',  ( 11.84999999999990372, 12.50000000000000000, 1.753560074763284016 ) ) ;
#77282 = EDGE_CURVE ( 'NONE', #98143, #63986, #119376, .T. ) ;
#77283 = PLANE ( 'NONE',  #119668 ) ;
#77284 = CIRCLE ( 'NONE', #33482, 5.000000000000004441 ) ;
#77285 = ORIENTED_EDGE ( 'NONE', *, *, #86837, .T. ) ;
#77286 = CARTESIAN_POINT ( 'NONE',  ( -7.900000000000014566, 12.50000000000000000, 0.6928203230275494784 ) ) ;
#77288 = AXIS2_PLACEMENT_3D ( 'NONE', #25918, #116854, #67765 ) ;
#77287 = VECTOR ( 'NONE', #93967, 1000.000000000000000 ) ;
#77289 = CARTESIAN_POINT ( 'NONE',  ( -5.650000000000023448, 2.500000000000000000, -6.048780366869526581 ) ) ;
#77290 = DIRECTION ( 'NONE',  ( -0.000000000000000000, -1.000000000000000000, -0.000000000000000000 ) ) ;
#77291 = CARTESIAN_POINT ( 'NONE',  ( 16.55712575656180618, -0.2764121571830139845, -6.093697237267636346 ) ) ;
#77292 = AXIS2_PLACEMENT_3D ( 'NONE', #88557, #99034, #99688 ) ;
#77293 = EDGE_LOOP ( 'NONE', ( #91783, #98055 ) ) ;
#77294 = FACE_OUTER_BOUND ( 'NONE', #115526, .T. ) ;
#77295 = ORIENTED_EDGE ( 'NONE', *, *, #95769, .F. ) ;
#77296 = EDGE_CURVE ( 'NONE', #91497, #50580, #116978, .T. ) ;
#77297 = CARTESIAN_POINT ( 'NONE',  ( 3.549999999999944755, 2.500000000000000000, -2.511473670974877948 ) ) ;
#77298 = CARTESIAN_POINT ( 'NONE',  ( 10.84999999999991260, 2.500000000000000000, 7.188010851410848723 ) ) ;
#77299 = ORIENTED_EDGE ( 'NONE', *, *, #43622, .F. ) ;
#77300 = CARTESIAN_POINT ( 'NONE',  ( -3.150000000000030109, 2.500000000000000000, -2.611473670974877592 ) ) ;
#77303 = DIRECTION ( 'NONE',  ( 0.000000000000000000, -0.000000000000000000, 1.000000000000000000 ) ) ;
#77302 = VECTOR ( 'NONE', #52446, 1000.000000000000000 ) ;
#77301 = VECTOR ( 'NONE', #100397, 1000.000000000000000 ) ;
#77304 = LINE ( 'NONE', #97583, #66343 ) ;
#77305 = DIRECTION ( 'NONE',  ( 0.000000000000000000, 1.000000000000000000, 0.000000000000000000 ) ) ;
#77306 = ORIENTED_EDGE ( 'NONE', *, *, #37633, .T. ) ;
#77307 = CARTESIAN_POINT ( 'NONE',  ( 5.649999999999934630, 2.500000000000000000, 6.841600689897072485 ) ) ;
#77308 = CARTESIAN_POINT ( 'NONE',  ( -4.600000000000028066, 2.500000000000000000, -4.922947341949753586 ) ) ;
#77309 = ADVANCED_FACE ( 'NONE', ( #49564 ), #79675, .T. ) ;
#77310 = DIRECTION ( 'NONE',  ( -0.000000000000000000, 1.000000000000000000, -0.000000000000000000 ) ) ;
#77311 = CARTESIAN_POINT ( 'NONE',  ( 1.649999999999949729, 2.500000000000000000, 7.188010851410848723 ) ) ;
#77312 = CARTESIAN_POINT ( 'NONE',  ( -11.64999999999999680, 2.500000000000000000, 6.495190528383297135 ) ) ;
#77313 = VERTEX_POINT ( 'NONE', #18145 ) ;
#77314 = ORIENTED_EDGE ( 'NONE', *, *, #54206, .F. ) ;
#77315 = DIRECTION ( 'NONE',  ( -0.000000000000000000, 1.000000000000000000, -0.000000000000000000 ) ) ;
#77316 = ORIENTED_EDGE ( 'NONE', *, *, #16994, .T. ) ;
#77317 = PLANE ( 'NONE',  #97979 ) ;
#77319 = EDGE_LOOP ( 'NONE', ( #75200, #123005, #71835, #43835 ) ) ;
#77318 = ORIENTED_EDGE ( 'NONE', *, *, #2770, .F. ) ;
#77320 = ORIENTED_EDGE ( 'NONE', *, *, #80922, .T. ) ;
#77321 = CARTESIAN_POINT ( 'NONE',  ( -10.65000000000000391, 12.50000000000000000, -2.511473670974873951 ) ) ;
#77322 = CONICAL_SURFACE ( 'NONE', #98148, 0.1000000000000002554, 0.003490658503988666988 ) ;
#77323 = CARTESIAN_POINT ( 'NONE',  ( 1.649999999999951505, 2.500000000000000000, -2.757883832488654097 ) ) ;
#77324 = AXIS2_PLACEMENT_3D ( 'NONE', #24504, #95177, #53965 ) ;
#77325 = CARTESIAN_POINT ( 'NONE',  ( -4.400000000000025224, 2.500000000000000000, 4.576537180435972019 ) ) ;
#77326 = EDGE_CURVE ( 'NONE', #33696, #116195, #58091, .T. ) ;
#77327 = SURFACE_STYLE_USAGE ( .BOTH. , #9238 ) ;
#77328 = DIRECTION ( 'NONE',  ( 0.000000000000000000, 0.000000000000000000, 1.000000000000000000 ) ) ;
#77329 = CARTESIAN_POINT ( 'NONE',  ( 1.449999999999952216, 12.50000000000000000, -2.511473670974877948 ) ) ;
#77330 = DIRECTION ( 'NONE',  ( 0.000000000000000000, 1.000000000000000000, 0.000000000000000000 ) ) ;
#77331 = DIRECTION ( 'NONE',  ( 0.000000000000000000, 0.000000000000000000, -1.000000000000000000 ) ) ;
#77332 = ORIENTED_EDGE ( 'NONE', *, *, #72486, .F. ) ;
#77334 = AXIS2_PLACEMENT_3D ( 'NONE', #20986, #41291, #80565 ) ;
#77333 = DIRECTION ( 'NONE',  ( 0.000000000000000000, 0.000000000000000000, -1.000000000000000000 ) ) ;
#77335 = ORIENTED_EDGE ( 'NONE', *, *, #48388, .T. ) ;
#77336 = EDGE_CURVE ( 'NONE', #116085, #31429, #19099, .T. ) ;
#77337 = ORIENTED_EDGE ( 'NONE', *, *, #68048, .T. ) ;
#77338 = EDGE_LOOP ( 'NONE', ( #59322, #127813 ) ) ;
#77339 = ORIENTED_EDGE ( 'NONE', *, *, #60532, .F. ) ;
#77340 = CARTESIAN_POINT ( 'NONE',  ( -4.200000000000025935, 12.50000000000000000, 4.330127018922196314 ) ) ;
#77341 = ADVANCED_FACE ( 'NONE', ( #30575 ), #37908, .T. ) ;
#77342 = ORIENTED_EDGE ( 'NONE', *, *, #75812, .F. ) ;
#77343 = ADVANCED_FACE ( 'NONE', ( #61954 ), #96383, .T. ) ;
#77344 = VERTEX_POINT ( 'NONE', #82888 ) ;
#77345 = EDGE_CURVE ( 'NONE', #47774, #110068, #127790, .T. ) ;
#77347 = EDGE_CURVE ( 'NONE', #42074, #55928, #52764, .T. ) ;
#77346 = CIRCLE ( 'NONE', #127520, 0.1000000000000000472 ) ;
#77348 = DIRECTION ( 'NONE',  ( -0.000000000000000000, 1.000000000000000000, -0.000000000000000000 ) ) ;
#77349 = DIRECTION ( 'NONE',  ( -0.000000000000000000, 1.000000000000000000, -0.000000000000000000 ) ) ;
#77350 = CIRCLE ( 'NONE', #18846, 0.06509327318403745899 ) ;
#77352 = DIRECTION ( 'NONE',  ( 0.000000000000000000, 0.000000000000000000, 1.000000000000000000 ) ) ;
#77351 = PRODUCT_DEFINITION_SHAPE ( 'NONE', 'NONE',  #98041 ) ;
#77353 = CARTESIAN_POINT ( 'NONE',  ( 4.999999999999938716, 2.500000000000000000, -5.122947341949753763 ) ) ;
#77354 = EDGE_CURVE ( 'NONE', #77248, #55502, #23295, .T. ) ;
#77355 = DIRECTION ( 'NONE',  ( 0.000000000000000000, 0.000000000000000000, 1.000000000000000000 ) ) ;
#77356 = VERTEX_POINT ( 'NONE', #20736 ) ;
#77357 = EDGE_CURVE ( 'NONE', #53692, #12100, #2478, .T. ) ;
#77358 = AXIS2_PLACEMENT_3D ( 'NONE', #27542, #98230, #107412 ) ;
#77359 = CARTESIAN_POINT ( 'NONE',  ( 6.649999999999931077, 12.50000000000000000, -6.495190528383302464 ) ) ;
#77360 = AXIS2_PLACEMENT_3D ( 'NONE', #54375, #56305, #104747 ) ;
#77361 = EDGE_CURVE ( 'NONE', #74772, #113119, #81580, .T. ) ;
#77362 = ORIENTED_EDGE ( 'NONE', *, *, #77036, .F. ) ;
#77363 = CARTESIAN_POINT ( 'NONE',  ( 8.749999999999921840, 12.50000000000000000, -5.802370205355749988 ) ) ;
#77364 = EDGE_CURVE ( 'NONE', #4623, #125419, #121489, .T. ) ;
#77365 = EDGE_LOOP ( 'NONE', ( #59052, #21160 ) ) ;
#77366 = CARTESIAN_POINT ( 'NONE',  ( 2.699999999999946443, 2.500000000000000000, 0.2464101615137735679 ) ) ;
#77367 = CIRCLE ( 'NONE', #98277, 0.06509327318403745899 ) ;
#77368 = VERTEX_POINT ( 'NONE', #111019 ) ;
#77369 = ORIENTED_EDGE ( 'NONE', *, *, #16609, .T. ) ;
#77370 = EDGE_CURVE ( 'NONE', #33550, #100266, #50842, .T. ) ;
#77371 = DIRECTION ( 'NONE',  ( 0.000000000000000000, 0.000000000000000000, -1.000000000000000000 ) ) ;
#77372 = CARTESIAN_POINT ( 'NONE',  ( 6.699999999999930012, 12.50000000000000000, -4.330127018922201643 ) ) ;
#77373 = DIRECTION ( 'NONE',  ( -1.000000000000000000, 0.000000000000000000, 0.000000000000000000 ) ) ;
#77374 = CARTESIAN_POINT ( 'NONE',  ( 13.54999999999989591, 12.50000000000000000, -1.818653347947326138 ) ) ;
#77375 = DIRECTION ( 'NONE',  ( -0.000000000000000000, -1.000000000000000000, -0.000000000000000000 ) ) ;
#77376 = VERTEX_POINT ( 'NONE', #72420 ) ;
#77377 = DIRECTION ( 'NONE',  ( 0.000000000000000000, -0.9999939076577903929, 0.003490651415223739937 ) ) ;
#77378 = DIRECTION ( 'NONE',  ( 0.000000000000000000, 0.000000000000000000, -1.000000000000000000 ) ) ;
#77379 = DIRECTION ( 'NONE',  ( -1.000000000000000000, -0.000000000000000000, -0.000000000000000000 ) ) ;
#77380 = DIRECTION ( 'NONE',  ( 0.000000000000000000, 1.000000000000000000, 0.000000000000000000 ) ) ;
#77381 = LINE ( 'NONE', #15205, #70977 ) ;
#77382 = EDGE_LOOP ( 'NONE', ( #96348, #61239, #5035, #57690 ) ) ;
#77383 = ORIENTED_EDGE ( 'NONE', *, *, #42840, .F. ) ;
#77384 = VECTOR ( 'NONE', #40981, 1000.000000000000000 ) ;
#77385 = DIRECTION ( 'NONE',  ( 0.000000000000000000, 1.000000000000000000, 0.000000000000000000 ) ) ;
#77386 = CIRCLE ( 'NONE', #92042, 0.1000000000000000472 ) ;
#77387 = ORIENTED_EDGE ( 'NONE', *, *, #117414, .F. ) ;
#77388 = DIRECTION ( 'NONE',  ( 0.000000000000000000, 0.000000000000000000, 1.000000000000000000 ) ) ;
#77389 = CARTESIAN_POINT ( 'NONE',  ( -11.25000000000000000, 2.500000000000000000, 2.857883832488649301 ) ) ;
#77391 = CIRCLE ( 'NONE', #20951, 0.06509327318403745899 ) ;
#77390 = CONICAL_SURFACE ( 'NONE', #16807, 0.1000000000000000472, 0.003490658503988666988 ) ;
#77392 = ORIENTED_EDGE ( 'NONE', *, *, #26473, .T. ) ;
#77393 = CARTESIAN_POINT ( 'NONE',  ( 186.0416666666666856, -4.445597072760122614, 7.699999999999998401 ) ) ;
#77394 = DIRECTION ( 'NONE',  ( 0.000000000000000000, 0.000000000000000000, 1.000000000000000000 ) ) ;
#77395 = FACE_OUTER_BOUND ( 'NONE', #105733, .T. ) ;
#77396 = DIRECTION ( 'NONE',  ( 0.000000000000000000, 1.000000000000000000, 0.000000000000000000 ) ) ;
#77397 = ORIENTED_EDGE ( 'NONE', *, *, #50922, .F. ) ;
#77398 = AXIS2_PLACEMENT_3D ( 'NONE', #6661, #67529, #126483 ) ;
#77399 = EDGE_CURVE ( 'NONE', #61052, #29513, #52135, .T. ) ;
#77400 = DIRECTION ( 'NONE',  ( 0.000000000000000000, 0.000000000000000000, 1.000000000000000000 ) ) ;
#77401 = FACE_OUTER_BOUND ( 'NONE', #85778, .T. ) ;
#77402 = ADVANCED_FACE ( 'NONE', ( #1723 ), #82239, .T. ) ;
#77403 = ORIENTED_EDGE ( 'NONE', *, *, #76206, .T. ) ;
#77404 = DIRECTION ( 'NONE',  ( 0.000000000000000000, -0.000000000000000000, 1.000000000000000000 ) ) ;
#77405 = DIRECTION ( 'NONE',  ( 0.000000000000000000, 0.000000000000000000, -1.000000000000000000 ) ) ;
#77406 = CARTESIAN_POINT ( 'NONE',  ( -1.850000000000033840, 2.500000000000000000, 1.718653347947321386 ) ) ;
#77407 = EDGE_CURVE ( 'NONE', #96594, #60331, #81900, .T. ) ;
#77408 = VERTEX_POINT ( 'NONE', #60673 ) ;
#77409 = CARTESIAN_POINT ( 'NONE',  ( -7.100000000000013856, 12.50000000000000000, 5.022947341949748790 ) ) ;
#77410 = ORIENTED_EDGE ( 'NONE', *, *, #81342, .T. ) ;
#77411 = DIRECTION ( 'NONE',  ( 0.000000000000000000, -0.9999939076577903929, 0.003490651415223739937 ) ) ;
#77412 = DIRECTION ( 'NONE',  ( 0.000000000000000000, 1.000000000000000000, 0.000000000000000000 ) ) ;
#77413 = PLANE ( 'NONE',  #24539 ) ;
#77414 = ORIENTED_EDGE ( 'NONE', *, *, #114150, .F. ) ;
#77415 = CIRCLE ( 'NONE', #52289, 0.1000000000000000472 ) ;
#77416 = DIRECTION ( 'NONE',  ( -0.000000000000000000, -1.000000000000000000, -0.000000000000000000 ) ) ;
#77417 = AXIS2_PLACEMENT_3D ( 'NONE', #14217, #113736, #3772 ) ;
#77418 = DIRECTION ( 'NONE',  ( 0.000000000000000000, 0.000000000000000000, -1.000000000000000000 ) ) ;
#77419 = ORIENTED_EDGE ( 'NONE', *, *, #9592, .T. ) ;
#77420 = LINE ( 'NONE', #27654, #21748 ) ;
#77421 = ORIENTED_EDGE ( 'NONE', *, *, #122553, .F. ) ;
#77422 = CONICAL_SURFACE ( 'NONE', #12569, 0.1000000000000000472, 0.003490658503988666988 ) ;
#77423 = DIRECTION ( 'NONE',  ( 0.000000000000000000, -0.9999939076577903929, 0.003490651415223739937 ) ) ;
#77424 = VERTEX_POINT ( 'NONE', #122169 ) ;
#77425 = DIRECTION ( 'NONE',  ( 0.000000000000000000, 0.000000000000000000, -1.000000000000000000 ) ) ;
#77426 = DIRECTION ( 'NONE',  ( 0.000000000000000000, 0.000000000000000000, -1.000000000000000000 ) ) ;
#77427 = ORIENTED_EDGE ( 'NONE', *, *, #106971, .F. ) ;
#77428 = EDGE_LOOP ( 'NONE', ( #107988, #60282 ) ) ;
#77429 = DIRECTION ( 'NONE',  ( 0.000000000000000000, 1.000000000000000000, 0.000000000000000000 ) ) ;
#77430 = DIRECTION ( 'NONE',  ( -0.000000000000000000, 1.000000000000000000, -0.000000000000000000 ) ) ;
#77431 = VERTEX_POINT ( 'NONE', #71772 ) ;
#77434 = EDGE_CURVE ( 'NONE', #50498, #102801, #111695, .T. ) ;
#77433 = CARTESIAN_POINT ( 'NONE',  ( 4.149999999999939959, 12.50000000000000000, 1.472243186433545459 ) ) ;
#77432 = CIRCLE ( 'NONE', #104617, 0.06509327318403745899 ) ;
#77435 = CARTESIAN_POINT ( 'NONE',  ( 5.799999999999931433, 2.500000000000000000, 4.330127018922196314 ) ) ;
#77436 = VECTOR ( 'NONE', #95450, 1000.000000000000000 ) ;
#77437 = DIRECTION ( 'NONE',  ( 0.000000000000000000, -0.9999939076577903929, 0.003490651415223739937 ) ) ;
#77438 = CYLINDRICAL_SURFACE ( 'NONE', #38459, 5.000000000000004441 ) ;
#77439 = CARTESIAN_POINT ( 'NONE',  ( -4.400000000000028777, 2.500000000000000000, -4.676537180435978769 ) ) ;
#77440 = DIRECTION ( 'NONE',  ( -4.274815082592931898E-19, -0.9999939076577903929, -0.003490651415223739937 ) ) ;
#77441 = AXIS2_PLACEMENT_3D ( 'NONE', #93517, #41216, #102051 ) ;
#77442 = ORIENTED_EDGE ( 'NONE', *, *, #65948, .F. ) ;
#77443 = EDGE_LOOP ( 'NONE', ( #31440, #21695 ) ) ;
#77444 = EDGE_LOOP ( 'NONE', ( #107313, #18190 ) ) ;
#77445 = ORIENTED_EDGE ( 'NONE', *, *, #43491, .F. ) ;
#77446 = CONICAL_SURFACE ( 'NONE', #27269, 0.1000000000000002554, 0.003490658503988666988 ) ;
#77447 = DIRECTION ( 'NONE',  ( 0.000000000000000000, 0.000000000000000000, -1.000000000000000000 ) ) ;
#77448 = DIRECTION ( 'NONE',  ( 0.000000000000000000, 0.000000000000000000, -1.000000000000000000 ) ) ;
#77449 = ADVANCED_FACE ( 'NONE', ( #112339 ), #62604, .T. ) ;
#77450 = DIRECTION ( 'NONE',  ( 0.000000000000000000, 1.000000000000000000, 0.000000000000000000 ) ) ;
#77451 = VERTEX_POINT ( 'NONE', #102513 ) ;
#77452 = FACE_BOUND ( 'NONE', #57335, .T. ) ;
#77453 = ORIENTED_EDGE ( 'NONE', *, *, #5057, .T. ) ;
#77454 = DIRECTION ( 'NONE',  ( -0.000000000000000000, -1.000000000000000000, -0.000000000000000000 ) ) ;
#77455 = LINE ( 'NONE', #117342, #96075 ) ;
#77456 = CARTESIAN_POINT ( 'NONE',  ( -4.400000000000025224, 2.500000000000000000, 3.983716857408420076 ) ) ;
#77457 = CARTESIAN_POINT ( 'NONE',  ( 12.69999999999989804, 2.500000000000000000, 0.4464101615137735513 ) ) ;
#77458 = CARTESIAN_POINT ( 'NONE',  ( -13.54999999999998828, 2.500000000000000000, -2.611473670974875372 ) ) ;
#77459 = LINE ( 'NONE', #127848, #97759 ) ;
#77460 = CARTESIAN_POINT ( 'NONE',  ( -5.400000000000020783, 12.50000000000000000, 0.6928203230275494784 ) ) ;
#77461 = CARTESIAN_POINT ( 'NONE',  ( 4.149999999999941735, 2.500000000000000000, -7.188010851410854052 ) ) ;
#77462 = ADVANCED_FACE ( 'NONE', ( #12816 ), #35946, .T. ) ;
#77463 = CARTESIAN_POINT ( 'NONE',  ( 11.44999999999991047, 12.50000000000000000, 6.148780366869520009 ) ) ;
#77464 = FACE_OUTER_BOUND ( 'NONE', #70721, .T. ) ;
#77465 = ORIENTED_EDGE ( 'NONE', *, *, #23607, .F. ) ;
#77466 = VERTEX_POINT ( 'NONE', #112976 ) ;
#77467 = ORIENTED_EDGE ( 'NONE', *, *, #807, .T. ) ;
#77468 = ORIENTED_EDGE ( 'NONE', *, *, #117163, .F. ) ;
#77469 = CARTESIAN_POINT ( 'NONE',  ( 0.4499999999999569344, 12.50000000000000000, -2.230156782645139391 ) ) ;
#77470 = CIRCLE ( 'NONE', #98385, 0.1000000000000000472 ) ;
#77471 = CARTESIAN_POINT ( 'NONE',  ( -2.100000000000033396, 12.50000000000000000, -3.572213422710612374 ) ) ;
#77472 = CIRCLE ( 'NONE', #6421, 0.1000000000000002554 ) ;
#77474 = ORIENTED_EDGE ( 'NONE', *, *, #15834, .T. ) ;
#77473 = EDGE_LOOP ( 'NONE', ( #19002, #109536 ) ) ;
#77475 = VERTEX_POINT ( 'NONE', #13474 ) ;
#77476 = CARTESIAN_POINT ( 'NONE',  ( 2.099999999999950351, 2.500000000000000000, -0.1000000000000022815 ) ) ;
#77477 = VECTOR ( 'NONE', #47298, 1000.000000000000000 ) ;
#77478 = CARTESIAN_POINT ( 'NONE',  ( -10.60000000000000142, 2.500000000000000000, 0.2464101615137736789 ) ) ;
#77479 = DIRECTION ( 'NONE',  ( 0.000000000000000000, 0.000000000000000000, 1.000000000000000000 ) ) ;
#77480 = FACE_OUTER_BOUND ( 'NONE', #98787, .T. ) ;
#77481 = DIRECTION ( 'NONE',  ( 0.000000000000000000, 1.000000000000000000, 0.000000000000000000 ) ) ;
#77482 = CARTESIAN_POINT ( 'NONE',  ( 129.5000000000000000, -1.500000000000000000, -6.000000000000000000 ) ) ;
#77483 = ORIENTED_EDGE ( 'NONE', *, *, #121679, .T. ) ;
#77484 = CARTESIAN_POINT ( 'NONE',  ( 2.949999999999943334, 2.500000000000000000, 6.595190528383296780 ) ) ;
#77485 = VERTEX_POINT ( 'NONE', #53427 ) ;
#77486 = ADVANCED_FACE ( 'NONE', ( #90756 ), #6223, .T. ) ;
#77487 = ORIENTED_EDGE ( 'NONE', *, *, #93046, .F. ) ;
#77488 = VERTEX_POINT ( 'NONE', #66448 ) ;
#77489 = DIRECTION ( 'NONE',  ( 0.000000000000000000, 0.000000000000000000, 1.000000000000000000 ) ) ;
#77490 = VERTEX_POINT ( 'NONE', #65800 ) ;
#77491 = EDGE_CURVE ( 'NONE', #67278, #17990, #103808, .T. ) ;
#77492 = VERTEX_POINT ( 'NONE', #5579 ) ;
#77493 = ADVANCED_FACE ( 'NONE', ( #96536 ), #44227, .T. ) ;
#77494 = CARTESIAN_POINT ( 'NONE',  ( -6.850000000000017408, 2.500000000000000000, -1.818653347947325916 ) ) ;
#77495 = CARTESIAN_POINT ( 'NONE',  ( 3.549999999999940314, 2.500000000000000000, 6.941600689897073018 ) ) ;
#77496 = CARTESIAN_POINT ( 'NONE',  ( 97.50000000000000000, 0.000000000000000000, 2.000000000000000000 ) ) ;
#77497 = DIRECTION ( 'NONE',  ( -1.000000000000000000, 0.000000000000000000, 1.224646799147352221E-16 ) ) ;
#77498 = EDGE_CURVE ( 'NONE', #80574, #63617, #86068, .T. ) ;
#77499 = ADVANCED_FACE ( 'NONE', ( #43612 ), #73498, .T. ) ;
#77500 = FACE_OUTER_BOUND ( 'NONE', #50767, .T. ) ;
#77501 = EDGE_CURVE ( 'NONE', #7606, #115280, #55350, .T. ) ;
#77502 = ORIENTED_EDGE ( 'NONE', *, *, #58258, .F. ) ;
#77503 = DIRECTION ( 'NONE',  ( -4.274815082592931898E-19, -0.9999939076577903929, -0.003490651415223739937 ) ) ;
#77504 = AXIS2_PLACEMENT_3D ( 'NONE', #2647, #90383, #70133 ) ;
#77505 = AXIS2_PLACEMENT_3D ( 'NONE', #10216, #109035, #91348 ) ;
#77506 = VERTEX_POINT ( 'NONE', #45540 ) ;
#77507 = CARTESIAN_POINT ( 'NONE',  ( -6.850000000000017408, 2.500000000000000000, -6.841600689897077814 ) ) ;
#77508 = EDGE_CURVE ( 'NONE', #114987, #21308, #113202, .T. ) ;
#77509 = ORIENTED_EDGE ( 'NONE', *, *, #64227, .F. ) ;
#77510 = CARTESIAN_POINT ( 'NONE',  ( 7.049999999999926992, 2.500000000000000000, 2.065063509461097624 ) ) ;
#77511 = CARTESIAN_POINT ( 'NONE',  ( -4.150000000000025224, 2.500000000000000000, 2.857883832488649301 ) ) ;
#77512 = ORIENTED_EDGE ( 'NONE', *, *, #87571, .T. ) ;
#77513 = CARTESIAN_POINT ( 'NONE',  ( -8.350000000000012079, 12.50000000000000000, -1.472243186433550122 ) ) ;
#77514 = CARTESIAN_POINT ( 'NONE',  ( -6.450000000000016165, 2.500000000000000000, 6.741600689897071952 ) ) ;
#77515 = ORIENTED_EDGE ( 'NONE', *, *, #26084, .T. ) ;
#77516 = EDGE_CURVE ( 'NONE', #121748, #28676, #56751, .T. ) ;
#77517 = CARTESIAN_POINT ( 'NONE',  ( -9.550000000000006040, 12.50000000000000000, -2.230156782645139391 ) ) ;
#77518 = ORIENTED_EDGE ( 'NONE', *, *, #44534, .F. ) ;
#77519 = ORIENTED_EDGE ( 'NONE', *, *, #103062, .F. ) ;
#77520 = CARTESIAN_POINT ( 'NONE',  ( 5.599999999999933031, 2.500000000000000000, -0.2464101615137783419 ) ) ;
#77521 = CARTESIAN_POINT ( 'NONE',  ( -8.100000000000013856, 2.500000000000000000, -3.983716857408426293 ) ) ;
#77522 = CARTESIAN_POINT ( 'NONE',  ( 183.9843750003414016, -8.734944146203032389, -1.604583208406768146E-15 ) ) ;
#77523 = CARTESIAN_POINT ( 'NONE',  ( -13.74999999999998757, 12.50000000000000000, 1.472243186433549456 ) ) ;
#77524 = AXIS2_PLACEMENT_3D ( 'NONE', #52287, #41200, #102661 ) ;
#77525 = DIRECTION ( 'NONE',  ( 0.000000000000000000, 0.000000000000000000, 1.000000000000000000 ) ) ;
#77526 = CARTESIAN_POINT ( 'NONE',  ( 4.399999999999937295, 2.500000000000000000, 4.576537180435972019 ) ) ;
#77527 = VECTOR ( 'NONE', #74524, 1000.000000000000000 ) ;
#77528 = EDGE_LOOP ( 'NONE', ( #51385, #43480 ) ) ;
#77529 = DIRECTION ( 'NONE',  ( 0.000000000000000000, 0.000000000000000000, 1.000000000000000000 ) ) ;
#77530 = LINE ( 'NONE', #14256, #66774 ) ;
#77531 = ORIENTED_EDGE ( 'NONE', *, *, #118642, .F. ) ;
#77532 = CIRCLE ( 'NONE', #25289, 0.06509327318403741736 ) ;
#77533 = DIRECTION ( 'NONE',  ( -0.000000000000000000, 1.000000000000000000, -0.000000000000000000 ) ) ;
#77534 = CARTESIAN_POINT ( 'NONE',  ( -13.14999999999999147, 2.500000000000000000, 2.411473670974877415 ) ) ;
#77535 = CARTESIAN_POINT ( 'NONE',  ( 11.24999999999991118, 2.500000000000000000, 5.702370205355745014 ) ) ;
#77536 = DIRECTION ( 'NONE',  ( 0.000000000000000000, 0.000000000000000000, 1.000000000000000000 ) ) ;
#77537 = DIRECTION ( 'NONE',  ( 0.000000000000000000, 0.000000000000000000, 1.000000000000000000 ) ) ;
#77538 = ORIENTED_EDGE ( 'NONE', *, *, #83548, .T. ) ;
#77539 = ADVANCED_FACE ( 'NONE', ( #126008 ), #79769, .T. ) ;
#77540 = FACE_OUTER_BOUND ( 'NONE', #11394, .T. ) ;
#77541 = DIRECTION ( 'NONE',  ( 0.000000000000000000, 0.000000000000000000, 1.000000000000000000 ) ) ;
#77542 = EDGE_LOOP ( 'NONE', ( #25958, #26235 ) ) ;
#77543 = CARTESIAN_POINT ( 'NONE',  ( 9.149999999999920419, 2.500000000000000000, -7.288010851410854585 ) ) ;
#77544 = EDGE_CURVE ( 'NONE', #94583, #111170, #23959, .T. ) ;
#77545 = EDGE_LOOP ( 'NONE', ( #109459, #117821, #52803, #4573 ) ) ;
#77546 = ORIENTED_EDGE ( 'NONE', *, *, #40403, .T. ) ;
#77547 = CARTESIAN_POINT ( 'NONE',  ( -14.99999999999998224, 2.500000000000000000, -0.6928203230275519209 ) ) ;
#77548 = VECTOR ( 'NONE', #1353, 1000.000000000000000 ) ;
#77549 = VECTOR ( 'NONE', #20536, 1000.000000000000000 ) ;
#77550 = CIRCLE ( 'NONE', #77644, 0.06509327318403745899 ) ;
#77551 = EDGE_LOOP ( 'NONE', ( #64618, #116606, #27008, #47479 ) ) ;
#77552 = CARTESIAN_POINT ( 'NONE',  ( -1.650000000000034328, 12.50000000000000000, -2.165063509461101710 ) ) ;
#77553 = CARTESIAN_POINT ( 'NONE',  ( -4.150000000000024336, 2.500000000000000000, 1.372243186433545370 ) ) ;
#77554 = DIRECTION ( 'NONE',  ( 0.000000000000000000, 0.000000000000000000, -1.000000000000000000 ) ) ;
#77555 = VERTEX_POINT ( 'NONE', #74342 ) ;
#77557 = FACE_BOUND ( 'NONE', #77603, .T. ) ;
#77556 = CIRCLE ( 'NONE', #113162, 0.1000000000000002554 ) ;
#77559 = ORIENTED_EDGE ( 'NONE', *, *, #125149, .F. ) ;
#77558 = CARTESIAN_POINT ( 'NONE',  ( 3.749999999999944045, 2.500000000000000000, -7.188010851410854052 ) ) ;
#77560 = DIRECTION ( 'NONE',  ( 0.000000000000000000, 1.000000000000000000, 0.000000000000000000 ) ) ;
#77561 = CARTESIAN_POINT ( 'NONE',  ( -2.500000000000032863, 12.50000000000000000, 5.022947341949748790 ) ) ;
#77562 = ORIENTED_EDGE ( 'NONE', *, *, #22355, .T. ) ;
#77563 = EDGE_LOOP ( 'NONE', ( #77502, #37609 ) ) ;
#77564 = ORIENTED_EDGE ( 'NONE', *, *, #111943, .F. ) ;
#77565 = CARTESIAN_POINT ( 'NONE',  ( -4.150000000000025224, 12.50000000000000000, 2.857883832488649301 ) ) ;
#77566 = DIRECTION ( 'NONE',  ( 0.000000000000000000, 1.000000000000000000, 0.000000000000000000 ) ) ;
#77567 = CARTESIAN_POINT ( 'NONE',  ( -11.04999999999999893, 2.500000000000000000, 1.818653347947321475 ) ) ;
#77568 = FACE_BOUND ( 'NONE', #116652, .T. ) ;
#77569 = ORIENTED_EDGE ( 'NONE', *, *, #53888, .F. ) ;
#77570 = DIRECTION ( 'NONE',  ( -0.000000000000000000, -1.000000000000000000, -0.000000000000000000 ) ) ;
#77571 = DIRECTION ( 'NONE',  ( 0.000000000000000000, 1.000000000000000000, 0.000000000000000000 ) ) ;
#77572 = ORIENTED_EDGE ( 'NONE', *, *, #120116, .T. ) ;
#77573 = EDGE_CURVE ( 'NONE', #102540, #72001, #48465, .T. ) ;
#77574 = CIRCLE ( 'NONE', #37880, 0.1000000000000000472 ) ;
#77575 = DIRECTION ( 'NONE',  ( -0.000000000000000000, -1.000000000000000000, -0.000000000000000000 ) ) ;
#77576 = FACE_OUTER_BOUND ( 'NONE', #85618, .T. ) ;
#77577 = CARTESIAN_POINT ( 'NONE',  ( -14.54999999999998472, 2.500000000000000000, 2.265063509461101354 ) ) ;
#77578 = CARTESIAN_POINT ( 'NONE',  ( 12.29999999999990656, 2.500000000000000000, -4.676537180435977881 ) ) ;
#77579 = DIRECTION ( 'NONE',  ( -1.000000000000000000, -0.000000000000000000, -0.000000000000000000 ) ) ;
#77580 = AXIS2_PLACEMENT_3D ( 'NONE', #116474, #58233, #26825 ) ;
#77581 = ADVANCED_FACE ( 'NONE', ( #93986 ), #114262, .T. ) ;
#77582 = AXIS2_PLACEMENT_3D ( 'NONE', #17434, #86168, #66545 ) ;
#77583 = EDGE_LOOP ( 'NONE', ( #113598, #113060, #75892, #99101 ) ) ;
#77584 = ORIENTED_EDGE ( 'NONE', *, *, #28330, .T. ) ;
#77585 = EDGE_LOOP ( 'NONE', ( #106814, #122957 ) ) ;
#77586 = ORIENTED_EDGE ( 'NONE', *, *, #41212, .F. ) ;
#77587 = ORIENTED_EDGE ( 'NONE', *, *, #74212, .F. ) ;
#77588 = CARTESIAN_POINT ( 'NONE',  ( 9.799999999999917222, 2.500000000000000000, 0.3464101615137735735 ) ) ;
#77589 = ADVANCED_FACE ( 'NONE', ( #104445 ), #105740, .F. ) ;
#77590 = DIRECTION ( 'NONE',  ( 0.000000000000000000, 1.000000000000000000, 0.000000000000000000 ) ) ;
#77591 = ORIENTED_EDGE ( 'NONE', *, *, #76473, .F. ) ;
#77592 = FACE_BOUND ( 'NONE', #70564, .T. ) ;
#77593 = EDGE_CURVE ( 'NONE', #104181, #99447, #119462, .T. ) ;
#77594 = VECTOR ( 'NONE', #90542, 1000.000000000000000 ) ;
#77595 = DIRECTION ( 'NONE',  ( -4.274815082592931898E-19, -0.9999939076577903929, -0.003490651415223739937 ) ) ;
#77596 = AXIS2_PLACEMENT_3D ( 'NONE', #82521, #64144, #41949 ) ;
#77597 = EDGE_CURVE ( 'NONE', #84209, #1733, #74989, .T. ) ;
#77598 = FACE_OUTER_BOUND ( 'NONE', #87562, .T. ) ;
#77599 = CARTESIAN_POINT ( 'NONE',  ( 184.5000000000000000, -4.107493067966395017, 6.449889041236108511 ) ) ;
#77600 = DIRECTION ( 'NONE',  ( -4.274815082592931898E-19, -0.9999939076577903929, -0.003490651415223739937 ) ) ;
#77601 = EDGE_CURVE ( 'NONE', #69877, #66637, #21270, .T. ) ;
#77602 = DIRECTION ( 'NONE',  ( 0.000000000000000000, 0.000000000000000000, 1.000000000000000000 ) ) ;
#77603 = EDGE_LOOP ( 'NONE', ( #94037, #52189 ) ) ;
#77604 = CARTESIAN_POINT ( 'NONE',  ( -5.200000000000020606, 2.500000000000000000, 3.883716857408421319 ) ) ;
#77605 = VECTOR ( 'NONE', #9621, 1000.000000000000000 ) ;
#77606 = VERTEX_POINT ( 'NONE', #115535 ) ;
#77607 = CONICAL_SURFACE ( 'NONE', #21184, 0.1000000000000000472, 0.003490658503988666988 ) ;
#77608 = ORIENTED_EDGE ( 'NONE', *, *, #59422, .T. ) ;
#77609 = VERTEX_POINT ( 'NONE', #55979 ) ;
#77610 = AXIS2_PLACEMENT_3D ( 'NONE', #82877, #31832, #103141 ) ;
#77611 = FACE_OUTER_BOUND ( 'NONE', #128851, .T. ) ;
#77612 = CARTESIAN_POINT ( 'NONE',  ( -5.650000000000019895, 2.500000000000000000, 6.741600689897071952 ) ) ;
#77613 = DIRECTION ( 'NONE',  ( 0.000000000000000000, 0.000000000000000000, 1.000000000000000000 ) ) ;
#77614 = ORIENTED_EDGE ( 'NONE', *, *, #90354, .T. ) ;
#77615 = CARTESIAN_POINT ( 'NONE',  ( 8.328334241103805269, 2.499999999999999556, -8.539519493613809686 ) ) ;
#77616 = CIRCLE ( 'NONE', #21189, 0.1000000000000002554 ) ;
#77617 = CARTESIAN_POINT ( 'NONE',  ( 0.1999999999999636513, 12.50000000000000000, -0.3464101615137760715 ) ) ;
#77618 = DIRECTION ( 'NONE',  ( 0.000000000000000000, 1.000000000000000000, 0.000000000000000000 ) ) ;
#77619 = EDGE_CURVE ( 'NONE', #38510, #115027, #47464, .T. ) ;
#77620 = AXIS2_PLACEMENT_3D ( 'NONE', #15274, #55234, #46698 ) ;
#77621 = CARTESIAN_POINT ( 'NONE',  ( 187.3593750003414016, 0.000000000000000000, 7.564683531250000925 ) ) ;
#77622 = CARTESIAN_POINT ( 'NONE',  ( 13.74999999999989519, 2.500000000000000000, -2.957883832488653830 ) ) ;
#77623 = LINE ( 'NONE', #69096, #111518 ) ;
#77624 = LINE ( 'NONE', #65879, #34931 ) ;
#77625 = ORIENTED_EDGE ( 'NONE', *, *, #55666, .T. ) ;
#77626 = DIRECTION ( 'NONE',  ( -0.000000000000000000, 1.000000000000000000, -0.000000000000000000 ) ) ;
#77627 = VERTEX_POINT ( 'NONE', #118128 ) ;
#77628 = ADVANCED_FACE ( 'NONE', ( #38968 ), #108308, .T. ) ;
#77629 = EDGE_LOOP ( 'NONE', ( #44094, #22077 ) ) ;
#77630 = DIRECTION ( 'NONE',  ( 0.000000000000000000, 0.000000000000000000, 1.000000000000000000 ) ) ;
#77631 = PLANE ( 'NONE',  #78086 ) ;
#77632 = LINE ( 'NONE', #78314, #16893 ) ;
#77633 = ORIENTED_EDGE ( 'NONE', *, *, #61581, .T. ) ;
#77635 = ADVANCED_FACE ( 'NONE', ( #88676 ), #19200, .T. ) ;
#77634 = ORIENTED_EDGE ( 'NONE', *, *, #23727, .T. ) ;
#77636 = CARTESIAN_POINT ( 'NONE',  ( -6.650000000000015454, 2.500000000000000000, 7.188010851410848723 ) ) ;
#77637 = DIRECTION ( 'NONE',  ( -0.000000000000000000, 1.000000000000000000, -0.000000000000000000 ) ) ;
#77639 = PLANE ( 'NONE',  #14742 ) ;
#77638 = VECTOR ( 'NONE', #17612, 1000.000000000000000 ) ;
#77640 = ORIENTED_EDGE ( 'NONE', *, *, #74094, .T. ) ;
#77641 = ORIENTED_EDGE ( 'NONE', *, *, #114151, .F. ) ;
#77642 = CONICAL_SURFACE ( 'NONE', #56701, 0.09999999999999999167, 0.003490658503988666988 ) ;
#77643 = EDGE_CURVE ( 'NONE', #45115, #11906, #7524, .T. ) ;
#77644 = AXIS2_PLACEMENT_3D ( 'NONE', #58528, #108879, #36944 ) ;
#77645 = DIRECTION ( 'NONE',  ( 0.000000000000000000, 0.000000000000000000, 1.000000000000000000 ) ) ;
#77646 = EDGE_CURVE ( 'NONE', #98829, #64904, #67203, .T. ) ;
#77647 = ADVANCED_FACE ( 'NONE', ( #18637 ), #4516, .T. ) ;
#77648 = VERTEX_POINT ( 'NONE', #108938 ) ;
#77649 = DIRECTION ( 'NONE',  ( 0.000000000000000000, 0.000000000000000000, 1.000000000000000000 ) ) ;
#77650 = AXIS2_PLACEMENT_3D ( 'NONE', #1258, #58895, #88995 ) ;
#77651 = CARTESIAN_POINT ( 'NONE',  ( 8.549999999999920774, 2.500000000000000000, 6.148780366869520897 ) ) ;
#77652 = VERTEX_POINT ( 'NONE', #19269 ) ;
#77653 = CARTESIAN_POINT ( 'NONE',  ( 7.499999999999925393, 12.50000000000000000, -3.637306695894650055 ) ) ;
#77654 = AXIS2_PLACEMENT_3D ( 'NONE', #86147, #104515, #54764 ) ;
#77655 = ADVANCED_FACE ( 'NONE', ( #127320 ), #111140, .T. ) ;
#77656 = DIRECTION ( 'NONE',  ( 0.000000000000000000, 1.000000000000000000, 0.000000000000000000 ) ) ;
#77657 = CARTESIAN_POINT ( 'NONE',  ( -10.80000000000000249, 2.500000000000000000, -4.230127018922197557 ) ) ;
#77658 = AXIS2_PLACEMENT_3D ( 'NONE', #112910, #63158, #65073 ) ;
#77659 = LINE ( 'NONE', #66549, #10340 ) ;
#77660 = ORIENTED_EDGE ( 'NONE', *, *, #30915, .T. ) ;
#77661 = EDGE_CURVE ( 'NONE', #107053, #49010, #37004, .T. ) ;
#77662 = DIRECTION ( 'NONE',  ( 0.000000000000000000, 0.000000000000000000, -1.000000000000000000 ) ) ;
#77663 = EDGE_CURVE ( 'NONE', #62516, #104677, #92366, .T. ) ;
#77664 = ORIENTED_EDGE ( 'NONE', *, *, #72402, .F. ) ;
#77665 = VERTEX_POINT ( 'NONE', #17330 ) ;
#77666 = DIRECTION ( 'NONE',  ( -0.000000000000000000, 1.000000000000000000, -0.000000000000000000 ) ) ;
#77667 = CARTESIAN_POINT ( 'NONE',  ( -11.64999999999999680, 12.50000000000000000, -6.560283801567336148 ) ) ;
#77668 = CARTESIAN_POINT ( 'NONE',  ( -6.249999999999984901, 12.50000000000000000, -2.099970236277064473 ) ) ;
#77669 = CARTESIAN_POINT ( 'NONE',  ( -0.4000000000000331624, 12.50000000000000000, -0.6928203230275519209 ) ) ;
#77670 = DIRECTION ( 'NONE',  ( -0.000000000000000000, -1.000000000000000000, -0.000000000000000000 ) ) ;
#77671 = CARTESIAN_POINT ( 'NONE',  ( -0.6500000000000389910, 2.500000000000000000, -1.818653347947326138 ) ) ;
#77672 = DIRECTION ( 'NONE',  ( 0.000000000000000000, 1.000000000000000000, 0.000000000000000000 ) ) ;
#77673 = CARTESIAN_POINT ( 'NONE',  ( 9.599999999999914380, 2.500000000000000000, 3.637306695894644726 ) ) ;
#77674 = DIRECTION ( 'NONE',  ( -0.000000000000000000, -1.000000000000000000, -0.000000000000000000 ) ) ;
#77675 = CARTESIAN_POINT ( 'NONE',  ( 3.749999999999942268, 2.500000000000000000, -5.702370205355749455 ) ) ;
#77676 = AXIS2_PLACEMENT_3D ( 'NONE', #75123, #3168, #53556 ) ;
#77677 = AXIS2_PLACEMENT_3D ( 'NONE', #5534, #87316, #44842 ) ;
#77678 = VERTEX_POINT ( 'NONE', #57285 ) ;
#77679 = CARTESIAN_POINT ( 'NONE',  ( 8.349999999999923261, 2.500000000000000000, -6.495190528383302464 ) ) ;
#77680 = CARTESIAN_POINT ( 'NONE',  ( 12.09999999999990195, 2.500000000000000000, -0.1000000000000022815 ) ) ;
#77681 = DIRECTION ( 'NONE',  ( 0.000000000000000000, 0.000000000000000000, -1.000000000000000000 ) ) ;
#77682 = PLANE ( 'NONE',  #6541 ) ;
#77683 = CARTESIAN_POINT ( 'NONE',  ( 15.39999999999989200, 2.500000000000000000, -0.7928203230275543412 ) ) ;
#77684 = AXIS2_PLACEMENT_3D ( 'NONE', #61487, #82420, #81119 ) ;
#77685 = ORIENTED_EDGE ( 'NONE', *, *, #45111, .T. ) ;
#77686 = CARTESIAN_POINT ( 'NONE',  ( 14.79999999999989413, 12.50000000000000000, -0.2813168883297408329 ) ) ;
#77687 = AXIS2_PLACEMENT_3D ( 'NONE', #42287, #10246, #99279 ) ;
#77688 = CARTESIAN_POINT ( 'NONE',  ( -4.600000000000028066, 2.500000000000000000, -5.122947341949753763 ) ) ;
#77690 = EDGE_LOOP ( 'NONE', ( #90599, #102144, #50801, #83884 ) ) ;
#77689 = DIRECTION ( 'NONE',  ( -0.000000000000000000, 1.000000000000000000, -0.000000000000000000 ) ) ;
#77691 =( BOUNDED_CURVE ( )  B_SPLINE_CURVE ( 2, ( #52962, #43162, #42511, #101416, #102062, #121046, #92896 ),
 .UNSPECIFIED., .F., .F. ) 
 B_SPLINE_CURVE_WITH_KNOTS ( ( 3, 2, 2, 3 ),
 ( 0.9285714285714292693, 0.9523809523809527722, 0.9761904761904763861, 1.000000000000000000 ),
 .UNSPECIFIED. ) 
 CURVE ( )  GEOMETRIC_REPRESENTATION_ITEM ( )  RATIONAL_B_SPLINE_CURVE ( ( 0.9999999999999962252, 0.8660254037844424824, 1.000000000000000000, 0.8660254037844387076, 1.000000000000000000, 0.8660254037844387076, 1.000000000000000000 ) ) 
 REPRESENTATION_ITEM ( '' )  );
#77692 = AXIS2_PLACEMENT_3D ( 'NONE', #116190, #54675, #16043 ) ;
#77693 = EDGE_LOOP ( 'NONE', ( #4001, #51774 ) ) ;
#77694 = PRODUCT_DEFINITION_FORMATION_WITH_SPECIFIED_SOURCE ( 'ANY', '', #95331, .NOT_KNOWN. ) ;
#77695 = EDGE_CURVE ( 'NONE', #28244, #68741, #117390, .T. ) ;
#77696 = ORIENTED_EDGE ( 'NONE', *, *, #99648, .F. ) ;
#77697 = EDGE_LOOP ( 'NONE', ( #26248, #72719, #71551, #64550 ) ) ;
#77698 = ORIENTED_EDGE ( 'NONE', *, *, #24438, .F. ) ;
#77699 = AXIS2_PLACEMENT_3D ( 'NONE', #61710, #102270, #41432 ) ;
#77700 = CARTESIAN_POINT ( 'NONE',  ( -7.100000000000017408, 12.50000000000000000, -3.637306695894650055 ) ) ;
#77701 = AXIS2_PLACEMENT_3D ( 'NONE', #107693, #27187, #57305 ) ;
#77702 = FACE_OUTER_BOUND ( 'NONE', #68159, .T. ) ;
#77703 = DIRECTION ( 'NONE',  ( 0.000000000000000000, 0.000000000000000000, 1.000000000000000000 ) ) ;
#77704 = DIRECTION ( 'NONE',  ( 0.000000000000000000, 0.000000000000000000, -1.000000000000000000 ) ) ;
#77705 = ORIENTED_EDGE ( 'NONE', *, *, #62618, .T. ) ;
#77706 = AXIS2_PLACEMENT_3D ( 'NONE', #103534, #102245, #32235 ) ;
#77707 = CARTESIAN_POINT ( 'NONE',  ( -0.8500000000000386136, 2.500000000000000000, 1.372243186433545370 ) ) ;
#77708 = ORIENTED_EDGE ( 'NONE', *, *, #98084, .F. ) ;
#77709 = CARTESIAN_POINT ( 'NONE',  ( 65.40459994267393995, -3.824478557797811984, -5.306485876524377865 ) ) ;
#77710 = CARTESIAN_POINT ( 'NONE',  ( 15.50772381592132021, -1.500000000000031752, -6.996973294590719483 ) ) ;
#77711 = CARTESIAN_POINT ( 'NONE',  ( 3.949999999999941558, 2.500000000000000000, -6.048780366869526581 ) ) ;
#77712 = DIRECTION ( 'NONE',  ( 0.000000000000000000, -0.000000000000000000, 1.000000000000000000 ) ) ;
#77713 = CARTESIAN_POINT ( 'NONE',  ( 7.099999999999926814, 2.500000000000000000, -0.6928203230275541413 ) ) ;
#77714 = VERTEX_POINT ( 'NONE', #129274 ) ;
#77715 = ORIENTED_EDGE ( 'NONE', *, *, #109079, .T. ) ;
#77716 = ORIENTED_EDGE ( 'NONE', *, *, #48588, .T. ) ;
#77717 = ORIENTED_EDGE ( 'NONE', *, *, #87681, .F. ) ;
#77718 = DIRECTION ( 'NONE',  ( 0.000000000000000000, 0.000000000000000000, 1.000000000000000000 ) ) ;
#77719 = CARTESIAN_POINT ( 'NONE',  ( -3.950000000000024603, 2.500000000000000000, 1.818653347947321475 ) ) ;
#77720 = DIRECTION ( 'NONE',  ( -0.000000000000000000, -1.000000000000000000, -0.000000000000000000 ) ) ;
#77721 = FACE_BOUND ( 'NONE', #108722, .T. ) ;
#77722 = DIRECTION ( 'NONE',  ( 0.000000000000000000, 1.000000000000000000, 0.000000000000000000 ) ) ;
#77723 = CARTESIAN_POINT ( 'NONE',  ( -7.050000000000016698, 2.500000000000000000, -6.395190528383301931 ) ) ;
#77724 = DIRECTION ( 'NONE',  ( 0.000000000000000000, 1.000000000000000000, 0.000000000000000000 ) ) ;
#77725 = DIRECTION ( 'NONE',  ( 0.000000000000000000, 1.000000000000000000, 0.000000000000000000 ) ) ;
#77726 = VECTOR ( 'NONE', #73651, 1000.000000000000000 ) ;
#77728 = VECTOR ( 'NONE', #90538, 1000.000000000000000 ) ;
#77727 = CARTESIAN_POINT ( 'NONE',  ( 184.5885416670080872, -6.551208109652273848, -3.782341765625003571 ) ) ;
#77729 = CARTESIAN_POINT ( 'NONE',  ( 7.299999999999927880, 12.50000000000000000, -4.611443907251939756 ) ) ;
#77730 = CARTESIAN_POINT ( 'NONE',  ( -2.900000000000029665, 2.500000000000000000, 4.430127018922196847 ) ) ;
#77731 = EDGE_CURVE ( 'NONE', #69690, #73131, #127887, .T. ) ;
#77732 = DIRECTION ( 'NONE',  ( 0.000000000000000000, 0.000000000000000000, 1.000000000000000000 ) ) ;
#77733 = AXIS2_PLACEMENT_3D ( 'NONE', #126438, #3590, #66848 ) ;
#77734 = ORIENTED_EDGE ( 'NONE', *, *, #81404, .T. ) ;
#77735 = ORIENTED_EDGE ( 'NONE', *, *, #17085, .T. ) ;
#77736 = VERTEX_POINT ( 'NONE', #77553 ) ;
#77737 = EDGE_LOOP ( 'NONE', ( #116906, #15145, #116198, #53464 ) ) ;
#77738 = AXIS2_PLACEMENT_3D ( 'NONE', #82145, #59950, #81502 ) ;
#77739 = AXIS2_PLACEMENT_3D ( 'NONE', #101715, #121337, #93821 ) ;
#77740 = EDGE_CURVE ( 'NONE', #38932, #1889, #125814, .T. ) ;
#77741 = FACE_OUTER_BOUND ( 'NONE', #60585, .T. ) ;
#77742 = FACE_BOUND ( 'NONE', #32265, .T. ) ;
#77743 = ADVANCED_FACE ( 'NONE', ( #49414 ), #25551, .T. ) ;
#77744 = CONICAL_SURFACE ( 'NONE', #31706, 0.1000000000000002554, 0.003490658503988666988 ) ;
#77745 = DIRECTION ( 'NONE',  ( -0.000000000000000000, -1.000000000000000000, -0.000000000000000000 ) ) ;
#77746 = EDGE_CURVE ( 'NONE', #41444, #47582, #116831, .T. ) ;
#77747 = EDGE_CURVE ( 'NONE', #101182, #55738, #77785, .T. ) ;
#77748 = EDGE_LOOP ( 'NONE', ( #87868, #81328, #46778, #80461 ) ) ;
#77749 = DIRECTION ( 'NONE',  ( 0.000000000000000000, -0.9999939076577903929, 0.003490651415223739937 ) ) ;
#77750 = EDGE_CURVE ( 'NONE', #850, #43290, #42303, .T. ) ;
#77751 = CARTESIAN_POINT ( 'NONE',  ( -10.84999999999999964, 2.500000000000000000, 2.957883832488649389 ) ) ;
#77752 = EDGE_CURVE ( 'NONE', #72018, #87403, #46829, .T. ) ;
#77753 = DIRECTION ( 'NONE',  ( 0.000000000000000000, 0.000000000000000000, 1.000000000000000000 ) ) ;
#77754 = ORIENTED_EDGE ( 'NONE', *, *, #60721, .F. ) ;
#77755 = DIRECTION ( 'NONE',  ( 0.000000000000000000, 0.000000000000000000, 1.000000000000000000 ) ) ;
#77756 = DIRECTION ( 'NONE',  ( 0.000000000000000000, 0.000000000000000000, 1.000000000000000000 ) ) ;
#77757 = VERTEX_POINT ( 'NONE', #100430 ) ;
#77758 = ORIENTED_EDGE ( 'NONE', *, *, #106885, .F. ) ;
#77759 = PLANE ( 'NONE',  #34095 ) ;
#77760 = DIRECTION ( 'NONE',  ( 0.000000000000000000, 0.000000000000000000, 1.000000000000000000 ) ) ;
#77761 = AXIS2_PLACEMENT_3D ( 'NONE', #46294, #36508, #90079 ) ;
#77762 = AXIS2_PLACEMENT_3D ( 'NONE', #117249, #86527, #76074 ) ;
#77763 = DIRECTION ( 'NONE',  ( 0.000000000000000000, 1.000000000000000000, 0.000000000000000000 ) ) ;
#77764 = DIRECTION ( 'NONE',  ( -0.000000000000000000, -1.000000000000000000, -0.000000000000000000 ) ) ;
#77765 = ORIENTED_EDGE ( 'NONE', *, *, #106933, .F. ) ;
#77766 = DIRECTION ( 'NONE',  ( 0.000000000000000000, 1.000000000000000000, 0.000000000000000000 ) ) ;
#77767 = ORIENTED_EDGE ( 'NONE', *, *, #84572, .F. ) ;
#77768 = VERTEX_POINT ( 'NONE', #93670 ) ;
#77769 = CARTESIAN_POINT ( 'NONE',  ( -13.09999999999999076, 2.500000000000000000, 3.983716857408420964 ) ) ;
#77770 = ORIENTED_EDGE ( 'NONE', *, *, #15603, .T. ) ;
#77771 = CARTESIAN_POINT ( 'NONE',  ( -3.100000000000028511, 12.50000000000000000, -4.676537180435977881 ) ) ;
#77772 = AXIS2_PLACEMENT_3D ( 'NONE', #25167, #6162, #103743 ) ;
#77773 = FACE_BOUND ( 'NONE', #91934, .T. ) ;
#77774 = CIRCLE ( 'NONE', #84042, 0.06509327318403745899 ) ;
#77775 = EDGE_LOOP ( 'NONE', ( #29910, #12729 ) ) ;
#77776 = AXIS2_PLACEMENT_3D ( 'NONE', #43590, #113599, #63857 ) ;
#77777 = DIRECTION ( 'NONE',  ( 0.000000000000000000, 1.000000000000000000, 0.000000000000000000 ) ) ;
#77778 = EDGE_LOOP ( 'NONE', ( #126538, #68127, #114533, #109959 ) ) ;
#77779 = FACE_OUTER_BOUND ( 'NONE', #11609, .T. ) ;
#77780 = CARTESIAN_POINT ( 'NONE',  ( -3.350000000000031619, 2.500000000000000000, -5.802370205355749988 ) ) ;
#77781 = PLANE ( 'NONE',  #25757 ) ;
#77782 = ADVANCED_FACE ( 'NONE', ( #123751 ), #21362, .T. ) ;
#77783 = DIRECTION ( 'NONE',  ( -0.000000000000000000, -1.000000000000000000, -0.000000000000000000 ) ) ;
#77784 = DIRECTION ( 'NONE',  ( 0.000000000000000000, 1.000000000000000000, 0.000000000000000000 ) ) ;
#77785 = CIRCLE ( 'NONE', #109178, 0.06509327318403745899 ) ;
#77786 = ORIENTED_EDGE ( 'NONE', *, *, #33326, .T. ) ;
#77787 = AXIS2_PLACEMENT_3D ( 'NONE', #23663, #4635, #123156 ) ;
#77788 = ORIENTED_EDGE ( 'NONE', *, *, #118023, .F. ) ;
#77789 = CARTESIAN_POINT ( 'NONE',  ( -15.59999999999998010, 12.50000000000000000, -0.3464101615137759604 ) ) ;
#77791 = CONICAL_SURFACE ( 'NONE', #66548, 0.1000000000000000056, 0.003490658503988666988 ) ;
#77790 = FACE_OUTER_BOUND ( 'NONE', #7556, .T. ) ;
#77792 = CONICAL_SURFACE ( 'NONE', #21368, 0.09999999999999982514, 0.003490658503988666988 ) ;
#77793 = VECTOR ( 'NONE', #42729, 1000.000000000000000 ) ;
#77795 = EDGE_CURVE ( 'NONE', #48968, #27815, #54378, .T. ) ;
#77794 = LINE ( 'NONE', #38558, #23007 ) ;
#77797 = EDGE_LOOP ( 'NONE', ( #16260, #85180 ) ) ;
#77796 = ORIENTED_EDGE ( 'NONE', *, *, #58298, .T. ) ;
#77798 = ORIENTED_EDGE ( 'NONE', *, *, #64631, .T. ) ;
#77799 = ADVANCED_FACE ( 'NONE', ( #110249 ), #48568, .T. ) ;
#77800 = DIRECTION ( 'NONE',  ( -0.000000000000000000, 1.000000000000000000, -0.000000000000000000 ) ) ;
#77801 = EDGE_CURVE ( 'NONE', #80231, #24379, #119649, .T. ) ;
#77802 = CARTESIAN_POINT ( 'NONE',  ( 142.3152275665817115, 2.500000000000000000, 4.152444035927816302 ) ) ;
#77803 = FACE_OUTER_BOUND ( 'NONE', #128877, .T. ) ;
#77804 = CIRCLE ( 'NONE', #84154, 0.06509327318403745899 ) ;
#77805 = CARTESIAN_POINT ( 'NONE',  ( 187.1249999999999716, -8.891194145520236347, -1.633285867636356299E-15 ) ) ;
#77806 = DIRECTION ( 'NONE',  ( -4.274815082592931898E-19, -0.9999939076577903929, -0.003490651415223739937 ) ) ;
#77807 = LINE ( 'NONE', #10369, #9517 ) ;
#77808 = CARTESIAN_POINT ( 'NONE',  ( -10.60000000000000142, 2.500000000000000000, 4.576537180435972019 ) ) ;
#77809 = EDGE_CURVE ( 'NONE', #91689, #110749, #10120, .T. ) ;
#77810 = EDGE_CURVE ( 'NONE', #98606, #68058, #29775, .T. ) ;
#77811 = CARTESIAN_POINT ( 'NONE',  ( 184.5729166673494888, 4.445597072760062218, -7.700000000000102318 ) ) ;
#77812 = ADVANCED_FACE ( 'NONE', ( #3355 ), #23415, .T. ) ;
#77813 = ORIENTED_EDGE ( 'NONE', *, *, #3738, .T. ) ;
#77815 = ORIENTED_EDGE ( 'NONE', *, *, #102200, .F. ) ;
#77814 = EDGE_CURVE ( 'NONE', #119917, #129137, #121707, .T. ) ;
#77816 = FACE_OUTER_BOUND ( 'NONE', #7447, .T. ) ;
#77817 = EDGE_CURVE ( 'NONE', #46788, #79361, #67301, .T. ) ;
#77818 = DIRECTION ( 'NONE',  ( 0.000000000000000000, 0.000000000000000000, 1.000000000000000000 ) ) ;
#77819 = ORIENTED_EDGE ( 'NONE', *, *, #86045, .F. ) ;
#77820 = ORIENTED_EDGE ( 'NONE', *, *, #73274, .T. ) ;
#77821 = CARTESIAN_POINT ( 'NONE',  ( 187.1510416670080303, 4.367472073101518859, -7.564683531249999149 ) ) ;
#77822 = CARTESIAN_POINT ( 'NONE',  ( 3.299999999999944755, 12.50000000000000000, -4.330127018922201643 ) ) ;
#77823 = CARTESIAN_POINT ( 'NONE',  ( -5.450000000000019718, 2.500000000000000000, 2.165063509461097713 ) ) ;
#77824 = EDGE_CURVE ( 'NONE', #49033, #11990, #99791, .T. ) ;
#77825 = CARTESIAN_POINT ( 'NONE',  ( 2.899999999999945732, 2.500000000000000000, -2.385244779468109755E-15 ) ) ;
#77826 = DIRECTION ( 'NONE',  ( 0.000000000000000000, -0.9999939076577903929, 0.003490651415223739937 ) ) ;
#77827 = CARTESIAN_POINT ( 'NONE',  ( -7.500000000000016875, 12.50000000000000000, 0.7579135962115869374 ) ) ;
#77828 = AXIS2_PLACEMENT_3D ( 'NONE', #95303, #36398, #16709 ) ;
#77829 = DIRECTION ( 'NONE',  ( 0.000000000000000000, 1.000000000000000000, 0.000000000000000000 ) ) ;
#77830 = EDGE_LOOP ( 'NONE', ( #76095, #55302, #116761, #128443 ) ) ;
#77831 = DIRECTION ( 'NONE',  ( 0.000000000000000000, 1.000000000000000000, 0.000000000000000000 ) ) ;
#77832 = VECTOR ( 'NONE', #39972, 1000.000000000000000 ) ;
#77833 = CONICAL_SURFACE ( 'NONE', #19240, 0.1000000000000002554, 0.003490658503988666988 ) ;
#77834 = DIRECTION ( 'NONE',  ( -0.000000000000000000, 1.000000000000000000, -0.000000000000000000 ) ) ;
#77835 = AXIS2_PLACEMENT_3D ( 'NONE', #52393, #91678, #2630 ) ;
#77836 = ORIENTED_EDGE ( 'NONE', *, *, #106635, .F. ) ;
#77837 = CONICAL_SURFACE ( 'NONE', #8872, 0.1000000000000000056, 0.003490658503988666988 ) ;
#77838 = AXIS2_PLACEMENT_3D ( 'NONE', #120473, #51107, #60293 ) ;
#77839 = ORIENTED_EDGE ( 'NONE', *, *, #85172, .F. ) ;
#77840 = AXIS2_PLACEMENT_3D ( 'NONE', #88582, #47376, #68938 ) ;
#77841 = CIRCLE ( 'NONE', #21413, 0.06509327318403745899 ) ;
#77842 = ORIENTED_EDGE ( 'NONE', *, *, #79261, .F. ) ;
#77843 = VERTEX_POINT ( 'NONE', #21218 ) ;
#77844 = FACE_OUTER_BOUND ( 'NONE', #118426, .T. ) ;
#77845 = CARTESIAN_POINT ( 'NONE',  ( -7.500000000000015099, 12.50000000000000000, -0.6928203230275541413 ) ) ;
#77846 = ORIENTED_EDGE ( 'NONE', *, *, #69202, .F. ) ;
#77847 = DIRECTION ( 'NONE',  ( -0.000000000000000000, -1.000000000000000000, -0.000000000000000000 ) ) ;
#77848 = CARTESIAN_POINT ( 'NONE',  ( 2.500000000000002220, -2.750000000000000444, -9.999999999999998224 ) ) ;
#77849 = CARTESIAN_POINT ( 'NONE',  ( 6.899999999999928413, 2.500000000000000000, -3.883716857408426648 ) ) ;
#77851 = ORIENTED_EDGE ( 'NONE', *, *, #55525, .T. ) ;
#77850 = CARTESIAN_POINT ( 'NONE',  ( -8.550000000000011369, 12.50000000000000000, 1.753560074763284016 ) ) ;
#77852 = LINE ( 'NONE', #7821, #116293 ) ;
#77854 = CARTESIAN_POINT ( 'NONE',  ( -0.4000000000000401013, 12.50000000000000000, -3.637306695894650055 ) ) ;
#77853 = CIRCLE ( 'NONE', #65332, 0.1000000000000002554 ) ;
#77855 = ORIENTED_EDGE ( 'NONE', *, *, #61610, .T. ) ;
#77856 = ADVANCED_FACE ( 'NONE', ( #10729 ), #19296, .T. ) ;
#77857 = ORIENTED_EDGE ( 'NONE', *, *, #72073, .T. ) ;
#77858 = ORIENTED_EDGE ( 'NONE', *, *, #18339, .F. ) ;
#77859 = CARTESIAN_POINT ( 'NONE',  ( -3.550000000000028688, 12.50000000000000000, 6.841600689897072485 ) ) ;
#77860 = CIRCLE ( 'NONE', #33967, 0.06509327318403745899 ) ;
#77861 = DIRECTION ( 'NONE',  ( 0.000000000000000000, 0.000000000000000000, -1.000000000000000000 ) ) ;
#77862 = CIRCLE ( 'NONE', #591, 0.06509327318403745899 ) ;
#77863 = ORIENTED_EDGE ( 'NONE', *, *, #126983, .T. ) ;
#77864 = DIRECTION ( 'NONE',  ( -0.000000000000000000, 1.000000000000000000, -0.000000000000000000 ) ) ;
#77865 = CARTESIAN_POINT ( 'NONE',  ( 7.699999999999925571, 2.500000000000000000, -4.676537180435978769 ) ) ;
#77866 = ADVANCED_FACE ( 'NONE', ( #34768 ), #88241, .T. ) ;
#77867 = DIRECTION ( 'NONE',  ( 0.000000000000000000, 0.000000000000000000, 1.000000000000000000 ) ) ;
#77868 = FACE_OUTER_BOUND ( 'NONE', #41943, .T. ) ;
#77869 = CIRCLE ( 'NONE', #111305, 7.700000000000000178 ) ;
#77870 = AXIS2_PLACEMENT_3D ( 'NONE', #111415, #169, #29654 ) ;
#77871 = VERTEX_POINT ( 'NONE', #276 ) ;
#77872 = CARTESIAN_POINT ( 'NONE',  ( 9.399999999999918643, 2.500000000000000000, 0.3464101615137736845 ) ) ;
#77873 = AXIS2_PLACEMENT_3D ( 'NONE', #24419, #32338, #114725 ) ;
#77874 = ORIENTED_EDGE ( 'NONE', *, *, #100470, .T. ) ;
#77875 = ORIENTED_EDGE ( 'NONE', *, *, #4436, .T. ) ;
#77876 = DIRECTION ( 'NONE',  ( -0.000000000000000000, -1.000000000000000000, -0.000000000000000000 ) ) ;
#77877 = DIRECTION ( 'NONE',  ( 0.000000000000000000, 0.000000000000000000, 1.000000000000000000 ) ) ;
#77878 = FACE_BOUND ( 'NONE', #5287, .T. ) ;
#77879 = DIRECTION ( 'NONE',  ( 0.000000000000000000, 1.000000000000000000, 0.000000000000000000 ) ) ;
#77881 = DIRECTION ( 'NONE',  ( 0.000000000000000000, 0.000000000000000000, -1.000000000000000000 ) ) ;
#77880 = CONICAL_SURFACE ( 'NONE', #115521, 0.09999999999999999167, 0.003490658503988666988 ) ;
#77882 = CARTESIAN_POINT ( 'NONE',  ( 4.149999999999936406, 12.50000000000000000, 6.495190528383297135 ) ) ;
#77883 = CIRCLE ( 'NONE', #73678, 0.1000000000000002554 ) ;
#77884 = AXIS2_PLACEMENT_3D ( 'NONE', #676, #23536, #62202 ) ;
#77885 = EDGE_LOOP ( 'NONE', ( #14764, #8028, #49055, #127140 ) ) ;
#77886 = PLANE ( 'NONE',  #17646 ) ;
#77887 = CARTESIAN_POINT ( 'NONE',  ( -7.100000000000018296, 2.500000000000000000, -2.385244779468109755E-15 ) ) ;
#77888 = DIRECTION ( 'NONE',  ( 0.000000000000000000, -0.9999939076577903929, 0.003490651415223739937 ) ) ;
#77889 = AXIS2_PLACEMENT_3D ( 'NONE', #115082, #36569, #104632 ) ;
#77890 = FACE_OUTER_BOUND ( 'NONE', #124926, .T. ) ;
#77891 = ORIENTED_EDGE ( 'NONE', *, *, #55211, .F. ) ;
#77892 = CARTESIAN_POINT ( 'NONE',  ( -1.450000000000036371, 12.50000000000000000, 6.841600689897072485 ) ) ;
#77893 = EDGE_CURVE ( 'NONE', #70298, #76682, #46490, .T. ) ;
#77894 = FACE_OUTER_BOUND ( 'NONE', #32936, .T. ) ;
#77895 = AXIS2_PLACEMENT_3D ( 'NONE', #110455, #1778, #120289 ) ;
#77896 = ORIENTED_EDGE ( 'NONE', *, *, #98847, .F. ) ;
#77897 = ORIENTED_EDGE ( 'NONE', *, *, #6979, .T. ) ;
#77898 = FACE_OUTER_BOUND ( 'NONE', #48851, .T. ) ;
#77899 = CARTESIAN_POINT ( 'NONE',  ( -0.6500000000000389910, 2.500000000000000000, -6.248780366869526759 ) ) ;
#77900 = FACE_BOUND ( 'NONE', #117534, .T. ) ;
#77901 = EDGE_CURVE ( 'NONE', #113533, #97281, #6665, .T. ) ;
#77902 = CARTESIAN_POINT ( 'NONE',  ( -0.8500000000000382805, 2.500000000000000000, -1.472243186433550122 ) ) ;
#77903 = ORIENTED_EDGE ( 'NONE', *, *, #92153, .T. ) ;
#77904 = LINE ( 'NONE', #87080, #56940 ) ;
#77905 = EDGE_CURVE ( 'NONE', #73152, #19309, #80804, .T. ) ;
#77906 = EDGE_LOOP ( 'NONE', ( #109034, #63246 ) ) ;
#77907 = ADVANCED_FACE ( 'NONE', ( #113955 ), #33475, .T. ) ;
#77908 = EDGE_LOOP ( 'NONE', ( #122078, #24235 ) ) ;
#77910 = AXIS2_PLACEMENT_3D ( 'NONE', #90390, #729, #40694 ) ;
#77909 = CARTESIAN_POINT ( 'NONE',  ( -8.950000000000006395, 2.500000000000000000, 6.741600689897071952 ) ) ;
#77911 = ADVANCED_FACE ( 'NONE', ( #53741 ), #38101, .T. ) ;
#77912 = EDGE_CURVE ( 'NONE', #88678, #119766, #6756, .T. ) ;
#77913 = CARTESIAN_POINT ( 'NONE',  ( 186.7083333333333428, -4.445597072760115509, -7.700000000000001954 ) ) ;
#77914 = EDGE_CURVE ( 'NONE', #24096, #19955, #63133, .T. ) ;
#77915 = ORIENTED_EDGE ( 'NONE', *, *, #28112, .F. ) ;
#77916 = CARTESIAN_POINT ( 'NONE',  ( -8.100000000000010303, 2.500000000000000000, 3.983716857408420964 ) ) ;
#77917 = CARTESIAN_POINT ( 'NONE',  ( -5.600000000000020073, 2.500000000000000000, 4.083716857408421497 ) ) ;
#77918 = AXIS2_PLACEMENT_3D ( 'NONE', #73555, #31719, #33026 ) ;
#77919 = AXIS2_PLACEMENT_3D ( 'NONE', #2594, #81807, #121733 ) ;
#77920 = CONICAL_SURFACE ( 'NONE', #13061, 0.1000000000000002554, 0.003490658503988666988 ) ;
#77921 = PLANE ( 'NONE',  #27726 ) ;
#77923 = ADVANCED_FACE ( 'NONE', ( #27481 ), #57620, .F. ) ;
#77922 = DIRECTION ( 'NONE',  ( 0.000000000000000000, 0.000000000000000000, 1.000000000000000000 ) ) ;
#77924 = ADVANCED_FACE ( 'NONE', ( #65487 ), #84052, .T. ) ;
#77926 = EDGE_CURVE ( 'NONE', #61216, #69514, #36042, .T. ) ;
#77925 = CIRCLE ( 'NONE', #86331, 0.1000000000000002554 ) ;
#77928 = EDGE_LOOP ( 'NONE', ( #38286, #15060 ) ) ;
#77927 = AXIS2_PLACEMENT_3D ( 'NONE', #108443, #60656, #38445 ) ;
#77929 = CONICAL_SURFACE ( 'NONE', #90436, 0.1000000000000002554, 0.003490658503988666988 ) ;
#77930 = DIRECTION ( 'NONE',  ( -0.000000000000000000, -1.000000000000000000, -0.000000000000000000 ) ) ;
#77931 = DIRECTION ( 'NONE',  ( 0.000000000000000000, 0.000000000000000000, 1.000000000000000000 ) ) ;
#77932 = LINE ( 'NONE', #109328, #55534 ) ;
#77933 = AXIS2_PLACEMENT_3D ( 'NONE', #56845, #103572, #83288 ) ;
#77934 = DIRECTION ( 'NONE',  ( 0.000000000000000000, 0.000000000000000000, 1.000000000000000000 ) ) ;
#77936 = EDGE_LOOP ( 'NONE', ( #125794, #98299, #81230, #29057 ) ) ;
#77935 = AXIS2_PLACEMENT_3D ( 'NONE', #6016, #83934, #85238 ) ;
#77937 = DIRECTION ( 'NONE',  ( 0.000000000000000000, 1.000000000000000000, 0.000000000000000000 ) ) ;
#77938 = ORIENTED_EDGE ( 'NONE', *, *, #99977, .F. ) ;
#77939 = FACE_OUTER_BOUND ( 'NONE', #86268, .T. ) ;
#77940 = AXIS2_PLACEMENT_3D ( 'NONE', #129396, #97326, #99911 ) ;
#77941 = ORIENTED_EDGE ( 'NONE', *, *, #120335, .F. ) ;
#77942 = DIRECTION ( 'NONE',  ( 0.000000000000000000, -0.000000000000000000, 1.000000000000000000 ) ) ;
#77943 = CARTESIAN_POINT ( 'NONE',  ( 87.49999999999995737, -5.708722954879577927, -4.899943752027913213 ) ) ;
#77944 = DIRECTION ( 'NONE',  ( -1.000000000000000000, 0.000000000000000000, -0.000000000000000000 ) ) ;
#77945 = DIRECTION ( 'NONE',  ( -4.274815082592931898E-19, -0.9999939076577903929, -0.003490651415223739937 ) ) ;
#77946 = ORIENTED_EDGE ( 'NONE', *, *, #97843, .T. ) ;
#77947 = CARTESIAN_POINT ( 'NONE',  ( 8.749999999999957367, 2.500000000000000000, -6.595190528383302109 ) ) ;
#77948 = CARTESIAN_POINT ( 'NONE',  ( -10.80000000000000071, 2.500000000000000000, 4.330127018922196314 ) ) ;
#77949 = CARTESIAN_POINT ( 'NONE',  ( 4.349999999999938360, 2.500000000000000000, 1.818653347947321475 ) ) ;
#77950 = DIRECTION ( 'NONE',  ( -4.274815082592931898E-19, -0.9999939076577903929, -0.003490651415223739937 ) ) ;
#77951 = CARTESIAN_POINT ( 'NONE',  ( 187.5000000000000000, 0.000000000000000000, 7.700000000000000178 ) ) ;
#77952 = CONICAL_SURFACE ( 'NONE', #94675, 0.1000000000000000472, 0.003490658503988666988 ) ;
#77953 = EDGE_LOOP ( 'NONE', ( #6733, #84399, #121483, #23154 ) ) ;
#77954 = EDGE_LOOP ( 'NONE', ( #49148, #26107, #117588, #47379 ) ) ;
#77955 = DIRECTION ( 'NONE',  ( 0.000000000000000000, 0.000000000000000000, 1.000000000000000000 ) ) ;
#77956 = VERTEX_POINT ( 'NONE', #36699 ) ;
#77957 = DIRECTION ( 'NONE',  ( -0.000000000000000000, 1.000000000000000000, -0.000000000000000000 ) ) ;
#77959 = EDGE_LOOP ( 'NONE', ( #98342, #92852, #37183, #16097 ) ) ;
#77958 = VERTEX_POINT ( 'NONE', #87059 ) ;
#77960 = ORIENTED_EDGE ( 'NONE', *, *, #78530, .F. ) ;
#77961 = FACE_OUTER_BOUND ( 'NONE', #67008, .T. ) ;
#77962 = AXIS2_PLACEMENT_3D ( 'NONE', #69997, #109924, #587 ) ;
#77963 = CIRCLE ( 'NONE', #113469, 0.06509327318403743123 ) ;
#77964 = CARTESIAN_POINT ( 'NONE',  ( -10.00000000000000533, 2.500000000000000000, 5.022947341949748790 ) ) ;
#77965 = CONICAL_SURFACE ( 'NONE', #34151, 0.1000000000000002554, 0.003490658503988666988 ) ;
#77966 = CARTESIAN_POINT ( 'NONE',  ( 2.949999999999943334, 2.500000000000000000, 6.495190528383297135 ) ) ;
#77967 = SURFACE_STYLE_FILL_AREA ( #38053 ) ;
#77968 = DIRECTION ( 'NONE',  ( 0.000000000000000000, 0.000000000000000000, 1.000000000000000000 ) ) ;
#77969 = LINE ( 'NONE', #117886, #39717 ) ;
#77970 = FACE_OUTER_BOUND ( 'NONE', #71446, .T. ) ;
#77971 = DIRECTION ( 'NONE',  ( 0.000000000000000000, 0.000000000000000000, 1.000000000000000000 ) ) ;
#77972 = ADVANCED_FACE ( 'NONE', ( #94968 ), #56939, .T. ) ;
#77973 = VECTOR ( 'NONE', #128310, 1000.000000000000000 ) ;
#77974 = CIRCLE ( 'NONE', #121786, 0.09999999999999982514 ) ;
#77975 = DIRECTION ( 'NONE',  ( -0.000000000000000000, 1.000000000000000000, -0.000000000000000000 ) ) ;
#77976 = ORIENTED_EDGE ( 'NONE', *, *, #119181, .F. ) ;
#77977 = EDGE_CURVE ( 'NONE', #30581, #1004, #105429, .T. ) ;
#77978 = CONICAL_SURFACE ( 'NONE', #63307, 0.09999999999999982514, 0.003490658503988666988 ) ;
#77979 = EDGE_LOOP ( 'NONE', ( #123505, #73608, #99048, #57671 ) ) ;
#77980 = ORIENTED_EDGE ( 'NONE', *, *, #42088, .T. ) ;
#77981 = CONICAL_SURFACE ( 'NONE', #36134, 0.1000000000000002554, 0.003490658503988666988 ) ;
#77982 = EDGE_LOOP ( 'NONE', ( #82661, #10982 ) ) ;
#77983 = EDGE_CURVE ( 'NONE', #11927, #42980, #96563, .T. ) ;
#77984 = DIRECTION ( 'NONE',  ( -0.000000000000000000, 1.000000000000000000, -0.000000000000000000 ) ) ;
#77985 = ORIENTED_EDGE ( 'NONE', *, *, #96975, .T. ) ;
#77986 = ORIENTED_EDGE ( 'NONE', *, *, #56811, .T. ) ;
#77987 = CIRCLE ( 'NONE', #38285, 0.1000000000000000472 ) ;
#77988 = EDGE_CURVE ( 'NONE', #37050, #40625, #10871, .T. ) ;
#77989 = CARTESIAN_POINT ( 'NONE',  ( 7.949999999999922018, 2.500000000000000000, -2.165063509461101710 ) ) ;
#77990 = CARTESIAN_POINT ( 'NONE',  ( -2.500000000000032419, 12.50000000000000000, -3.572213422710612374 ) ) ;
#77991 = DIRECTION ( 'NONE',  ( 0.000000000000000000, 0.000000000000000000, 1.000000000000000000 ) ) ;
#77992 = CIRCLE ( 'NONE', #38290, 0.09999999999999982514 ) ;
#77993 = DIRECTION ( 'NONE',  ( -0.000000000000000000, 1.000000000000000000, -0.000000000000000000 ) ) ;
#77994 = DIRECTION ( 'NONE',  ( 0.000000000000000000, 0.000000000000000000, 1.000000000000000000 ) ) ;
#77995 = EDGE_LOOP ( 'NONE', ( #1634, #63471, #67792, #42929 ) ) ;
#77996 = AXIS2_PLACEMENT_3D ( 'NONE', #110436, #1130, #120275 ) ;
#77997 = DIRECTION ( 'NONE',  ( -0.000000000000000000, -1.000000000000000000, -0.000000000000000000 ) ) ;
#77998 = VERTEX_POINT ( 'NONE', #45222 ) ;
#77999 = DIRECTION ( 'NONE',  ( 0.000000000000000000, 0.000000000000000000, -1.000000000000000000 ) ) ;
#78000 = ORIENTED_EDGE ( 'NONE', *, *, #127310, .T. ) ;
#78001 = VECTOR ( 'NONE', #66504, 1000.000000000000000 ) ;
#78002 = CARTESIAN_POINT ( 'NONE',  ( -12.09999999999999432, 2.500000000000000000, 3.737306695894644371 ) ) ;
#78003 = ORIENTED_EDGE ( 'NONE', *, *, #35638, .F. ) ;
#78004 = ADVANCED_FACE ( 'NONE', ( #115883 ), #65267, .T. ) ;
#78005 = EDGE_LOOP ( 'NONE', ( #26334, #107377, #121590, #40068 ) ) ;
#78006 = CARTESIAN_POINT ( 'NONE',  ( -8.350000000000013856, 2.500000000000000000, -7.188010851410848723 ) ) ;
#78007 = CARTESIAN_POINT ( 'NONE',  ( -12.94999999999999218, 2.500000000000000000, 2.165063509461101265 ) ) ;
#78008 = DIRECTION ( 'NONE',  ( 0.000000000000000000, -0.9999939076577903929, 0.003490651415223739937 ) ) ;
#78009 = DIRECTION ( 'NONE',  ( 0.000000000000000000, -0.9999939076577903929, 0.003490651415223739937 ) ) ;
#78010 = CARTESIAN_POINT ( 'NONE',  ( -10.65000000000000391, 12.50000000000000000, -6.776507416713037912 ) ) ;
#78011 = ORIENTED_EDGE ( 'NONE', *, *, #127328, .F. ) ;
#78012 = LINE ( 'NONE', #48564, #116782 ) ;
#78014 = CONICAL_SURFACE ( 'NONE', #88467, 0.1000000000000002554, 0.003490658503988666988 ) ;
#78013 = DIRECTION ( 'NONE',  ( -0.000000000000000000, -1.000000000000000000, -0.000000000000000000 ) ) ;
#78015 = DIRECTION ( 'NONE',  ( 0.000000000000000000, 0.000000000000000000, 1.000000000000000000 ) ) ;
#78016 = DIRECTION ( 'NONE',  ( -0.000000000000000000, -1.000000000000000000, -0.000000000000000000 ) ) ;
#78017 = LINE ( 'NONE', #40039, #100042 ) ;
#78018 = ORIENTED_EDGE ( 'NONE', *, *, #98019, .T. ) ;
#78019 = CIRCLE ( 'NONE', #98953, 0.06509327318403745899 ) ;
#78020 = EDGE_CURVE ( 'NONE', #126618, #117214, #36041, .T. ) ;
#78021 = AXIS2_PLACEMENT_3D ( 'NONE', #12696, #93224, #82105 ) ;
#78022 = ORIENTED_EDGE ( 'NONE', *, *, #18503, .T. ) ;
#78023 = CIRCLE ( 'NONE', #71769, 0.1000000000000000472 ) ;
#78024 = CIRCLE ( 'NONE', #71770, 0.1000000000000002554 ) ;
#78025 = DIRECTION ( 'NONE',  ( 0.000000000000000000, 1.000000000000000000, 0.000000000000000000 ) ) ;
#78026 = VERTEX_POINT ( 'NONE', #85127 ) ;
#78027 = CARTESIAN_POINT ( 'NONE',  ( 9.599999999999914380, 12.50000000000000000, -4.395220292106239768 ) ) ;
#78028 = DIRECTION ( 'NONE',  ( 0.000000000000000000, 0.000000000000000000, -1.000000000000000000 ) ) ;
#78029 = CIRCLE ( 'NONE', #75874, 0.06509327318403745899 ) ;
#78030 = AXIS2_PLACEMENT_3D ( 'NONE', #78139, #38883, #30338 ) ;
#78031 = CIRCLE ( 'NONE', #82244, 0.09999999999999982514 ) ;
#78032 = AXIS2_PLACEMENT_3D ( 'NONE', #21455, #41766, #81662 ) ;
#78033 = CIRCLE ( 'NONE', #103167, 0.06509327318403745899 ) ;
#78034 = ORIENTED_EDGE ( 'NONE', *, *, #126217, .F. ) ;
#78035 = CARTESIAN_POINT ( 'NONE',  ( 185.1250000000000284, -8.891194145520236347, -1.633285867636356693E-15 ) ) ;
#78036 = DIRECTION ( 'NONE',  ( -4.274815082592931898E-19, -0.9999939076577903929, -0.003490651415223739937 ) ) ;
#78037 = EDGE_CURVE ( 'NONE', #17665, #34687, #96879, .T. ) ;
#78038 = DIRECTION ( 'NONE',  ( -0.000000000000000000, -1.000000000000000000, -0.000000000000000000 ) ) ;
#78039 = PLANE ( 'NONE',  #1649 ) ;
#78040 = ORIENTED_EDGE ( 'NONE', *, *, #83289, .F. ) ;
#78041 = CIRCLE ( 'NONE', #71784, 0.09999999999999982514 ) ;
#78042 = DIRECTION ( 'NONE',  ( 0.000000000000000000, 0.000000000000000000, -1.000000000000000000 ) ) ;
#78043 = DIRECTION ( 'NONE',  ( 0.000000000000000000, -0.000000000000000000, 1.000000000000000000 ) ) ;
#78044 = EDGE_LOOP ( 'NONE', ( #24712, #29050, #101978, #62291 ) ) ;
#78045 = CARTESIAN_POINT ( 'NONE',  ( -5.400000000000019895, 2.500000000000000000, 3.637306695894644726 ) ) ;
#78046 = DIRECTION ( 'NONE',  ( 0.000000000000000000, 1.000000000000000000, 0.000000000000000000 ) ) ;
#78047 = DIRECTION ( 'NONE',  ( 0.000000000000000000, 0.000000000000000000, -1.000000000000000000 ) ) ;
#78048 = AXIS2_PLACEMENT_3D ( 'NONE', #17840, #87856, #78053 ) ;
#78049 = EDGE_LOOP ( 'NONE', ( #83332, #107779, #77538, #14759 ) ) ;
#78050 = CARTESIAN_POINT ( 'NONE',  ( 195.0000000000000000, 9.236194438982661209E-16, 7.541925104783893552 ) ) ;
#78051 = EDGE_LOOP ( 'NONE', ( #82753, #119935 ) ) ;
#78052 = DIRECTION ( 'NONE',  ( 0.000000000000000000, 1.000000000000000000, 0.000000000000000000 ) ) ;
#78053 = DIRECTION ( 'NONE',  ( 0.000000000000000000, 0.000000000000000000, 1.000000000000000000 ) ) ;
#78054 = CARTESIAN_POINT ( 'NONE',  ( -0.4000000000000396572, 2.500000000000000000, 3.537306695894645081 ) ) ;
#78055 = AXIS2_PLACEMENT_3D ( 'NONE', #5734, #93499, #3822 ) ;
#78056 = ORIENTED_EDGE ( 'NONE', *, *, #44596, .T. ) ;
#78057 = VECTOR ( 'NONE', #76158, 1000.000000000000000 ) ;
#78058 = CIRCLE ( 'NONE', #21633, 0.09999999999999982514 ) ;
#78059 = DIRECTION ( 'NONE',  ( 0.000000000000000000, 0.000000000000000000, 1.000000000000000000 ) ) ;
#78060 = ADVANCED_FACE ( 'NONE', ( #127005 ), #105062, .T. ) ;
#78061 = DIRECTION ( 'NONE',  ( 0.000000000000000000, -0.9999939076577903929, 0.003490651415223739937 ) ) ;
#78062 = EDGE_LOOP ( 'NONE', ( #93824, #93288 ) ) ;
#78063 = DIRECTION ( 'NONE',  ( 0.000000000000000000, 0.000000000000000000, 1.000000000000000000 ) ) ;
#78064 = EDGE_LOOP ( 'NONE', ( #28534, #67799 ) ) ;
#78065 = VECTOR ( 'NONE', #36484, 1000.000000000000000 ) ;
#78066 = FACE_OUTER_BOUND ( 'NONE', #51499, .T. ) ;
#78068 = ADVANCED_FACE ( 'NONE', ( #55673 ), #127637, .T. ) ;
#78067 = CIRCLE ( 'NONE', #109462, 0.09999999999999982514 ) ;
#78069 = AXIS2_PLACEMENT_3D ( 'NONE', #64182, #2036, #92345 ) ;
#78070 = VERTEX_POINT ( 'NONE', #37968 ) ;
#78071 = DIRECTION ( 'NONE',  ( 0.000000000000000000, 0.000000000000000000, 1.000000000000000000 ) ) ;
#78072 = CARTESIAN_POINT ( 'NONE',  ( -14.34999999999998543, 12.50000000000000000, -1.818653347947323695 ) ) ;
#78073 = EDGE_CURVE ( 'NONE', #71153, #123556, #26224, .T. ) ;
#78074 = ORIENTED_EDGE ( 'NONE', *, *, #6816, .F. ) ;
#78075 = EDGE_CURVE ( 'NONE', #46687, #129191, #29874, .T. ) ;
#78076 = ORIENTED_EDGE ( 'NONE', *, *, #24118, .T. ) ;
#78077 = ADVANCED_FACE ( 'NONE', ( #64841 ), #77880, .T. ) ;
#78079 = EDGE_CURVE ( 'NONE', #22492, #55110, #23606, .T. ) ;
#78078 = CIRCLE ( 'NONE', #57144, 0.1000000000000002554 ) ;
#78080 = FACE_OUTER_BOUND ( 'NONE', #115164, .T. ) ;
#78081 = CARTESIAN_POINT ( 'NONE',  ( 9.349999999999916156, 2.500000000000000000, 6.148780366869520009 ) ) ;
#78082 = VERTEX_POINT ( 'NONE', #60838 ) ;
#78083 = CARTESIAN_POINT ( 'NONE',  ( 179.5000000000000000, -0.6250000000000000000, 7.634788798650553154 ) ) ;
#78084 = CARTESIAN_POINT ( 'NONE',  ( -11.25000000000000178, 12.50000000000000000, -5.802370205355746435 ) ) ;
#78085 = CIRCLE ( 'NONE', #42505, 0.06509327318403745899 ) ;
#78086 = AXIS2_PLACEMENT_3D ( 'NONE', #88079, #58660, #58019 ) ;
#78087 = EDGE_CURVE ( 'NONE', #93720, #109560, #109284, .T. ) ;
#78088 = CARTESIAN_POINT ( 'NONE',  ( -9.150000000000009237, 2.500000000000000000, -2.857883832488653741 ) ) ;
#78089 = DIRECTION ( 'NONE',  ( 0.000000000000000000, 0.000000000000000000, 1.000000000000000000 ) ) ;
#78090 = EDGE_CURVE ( 'NONE', #31018, #46687, #89655, .T. ) ;
#78091 = FACE_OUTER_BOUND ( 'NONE', #20475, .T. ) ;
#78092 = CIRCLE ( 'NONE', #63423, 0.1000000000000000056 ) ;
#78093 = DIRECTION ( 'NONE',  ( 0.000000000000000000, 0.000000000000000000, -1.000000000000000000 ) ) ;
#78094 = EDGE_CURVE ( 'NONE', #40852, #73230, #86281, .T. ) ;
#78095 = AXIS2_PLACEMENT_3D ( 'NONE', #129139, #116700, #108168 ) ;
#78096 = EDGE_CURVE ( 'NONE', #77488, #117879, #8923, .T. ) ;
#78097 = EDGE_CURVE ( 'NONE', #48532, #92622, #69351, .T. ) ;
#78098 = ORIENTED_EDGE ( 'NONE', *, *, #80811, .F. ) ;
#78099 = ORIENTED_EDGE ( 'NONE', *, *, #82395, .T. ) ;
#78100 = ORIENTED_EDGE ( 'NONE', *, *, #38941, .T. ) ;
#78101 = ORIENTED_EDGE ( 'NONE', *, *, #82081, .T. ) ;
#78102 = CARTESIAN_POINT ( 'NONE',  ( -9.550000000000007816, 2.500000000000000000, -6.395190528383296602 ) ) ;
#78103 = DIRECTION ( 'NONE',  ( 0.000000000000000000, -0.9999939076577903929, 0.003490651415223739937 ) ) ;
#78104 = CARTESIAN_POINT ( 'NONE',  ( 12.29999999999990656, 2.500000000000000000, -4.576537180435977348 ) ) ;
#78105 = ORIENTED_EDGE ( 'NONE', *, *, #2127, .F. ) ;
#78106 = FACE_BOUND ( 'NONE', #122000, .T. ) ;
#78107 = ORIENTED_EDGE ( 'NONE', *, *, #125569, .F. ) ;
#78108 = EDGE_CURVE ( 'NONE', #118058, #100004, #54899, .T. ) ;
#78109 = FACE_OUTER_BOUND ( 'NONE', #28744, .T. ) ;
#78110 = DIRECTION ( 'NONE',  ( 0.000000000000000000, -0.9999939076577903929, 0.003490651415223739937 ) ) ;
#78111 = CARTESIAN_POINT ( 'NONE',  ( 149.5981739382431783, 0.5000000000000000000, -1.703575533167231537 ) ) ;
#78112 = DIRECTION ( 'NONE',  ( 0.000000000000000000, 0.000000000000000000, 1.000000000000000000 ) ) ;
#78113 = FACE_OUTER_BOUND ( 'NONE', #44306, .T. ) ;
#78114 = LINE ( 'NONE', #8695, #106177 ) ;
#78115 = DIRECTION ( 'NONE',  ( 0.000000000000000000, 0.000000000000000000, 1.000000000000000000 ) ) ;
#78116 = CARTESIAN_POINT ( 'NONE',  ( -1.450000000000035039, 2.500000000000000000, -6.841600689897077814 ) ) ;
#78117 = VECTOR ( 'NONE', #92147, 1000.000000000000000 ) ;
#78118 = CONICAL_SURFACE ( 'NONE', #97068, 0.1000000000000002554, 0.003490658503988666988 ) ;
#78119 = DIRECTION ( 'NONE',  ( 0.000000000000000000, 0.000000000000000000, 1.000000000000000000 ) ) ;
#78120 = CARTESIAN_POINT ( 'NONE',  ( -0.8500000000000382805, 12.50000000000000000, -7.188010851410854052 ) ) ;
#78121 = CIRCLE ( 'NONE', #36364, 0.06509327318403745899 ) ;
#78123 = ORIENTED_EDGE ( 'NONE', *, *, #120346, .F. ) ;
#78122 = CIRCLE ( 'NONE', #48889, 10.00000000000000000 ) ;
#78124 = ORIENTED_EDGE ( 'NONE', *, *, #120476, .T. ) ;
#78125 = EDGE_LOOP ( 'NONE', ( #40283, #89564 ) ) ;
#78126 = AXIS2_PLACEMENT_3D ( 'NONE', #120911, #10318, #474 ) ;
#78127 = ORIENTED_EDGE ( 'NONE', *, *, #67369, .T. ) ;
#78129 = CONICAL_SURFACE ( 'NONE', #9160, 0.09999999999999982514, 0.003490658503988666988 ) ;
#78128 = CARTESIAN_POINT ( 'NONE',  ( -3.550000000000027800, 12.50000000000000000, 6.148780366869520009 ) ) ;
#78130 = CIRCLE ( 'NONE', #21693, 0.09999999999999999167 ) ;
#78131 = LINE ( 'NONE', #67643, #10918 ) ;
#78133 = ORIENTED_EDGE ( 'NONE', *, *, #90693, .F. ) ;
#78132 = EDGE_LOOP ( 'NONE', ( #50263, #82740 ) ) ;
#78134 = ORIENTED_EDGE ( 'NONE', *, *, #764, .F. ) ;
#78135 = CARTESIAN_POINT ( 'NONE',  ( -4.400000000000028777, 12.50000000000000000, -4.741630453620016006 ) ) ;
#78136 = CIRCLE ( 'NONE', #55041, 0.1000000000000002554 ) ;
#78137 = CIRCLE ( 'NONE', #88484, 0.09999999999999982514 ) ;
#78138 = CONICAL_SURFACE ( 'NONE', #128316, 0.1000000000000002554, 0.003490658503988666988 ) ;
#78139 = CARTESIAN_POINT ( 'NONE',  ( 12.94999999999990337, 12.50000000000000000, 2.165063509461097713 ) ) ;
#78140 = CARTESIAN_POINT ( 'NONE',  ( -1.250000000000036193, 12.50000000000000000, 1.407149913249508000 ) ) ;
#78141 = CARTESIAN_POINT ( 'NONE',  ( -2.500000000000032863, 2.500000000000000000, 4.922947341949748257 ) ) ;
#78142 = CARTESIAN_POINT ( 'NONE',  ( -0.6000000000000323963, 2.500000000000000000, 0.4464101615137759382 ) ) ;
#78143 = DIRECTION ( 'NONE',  ( 0.000000000000000000, 1.000000000000000000, 0.000000000000000000 ) ) ;
#78144 = CIRCLE ( 'NONE', #11216, 0.1000000000000000472 ) ;
#78145 = CARTESIAN_POINT ( 'NONE',  ( -7.100000000000017408, 2.500000000000000000, -0.6928203230275542523 ) ) ;
#78146 = ORIENTED_EDGE ( 'NONE', *, *, #76831, .F. ) ;
#78147 = DIRECTION ( 'NONE',  ( -0.000000000000000000, -1.000000000000000000, -0.000000000000000000 ) ) ;
#78148 = ORIENTED_EDGE ( 'NONE', *, *, #22996, .T. ) ;
#78149 = ADVANCED_FACE ( 'NONE', ( #128955 ), #119111, .T. ) ;
#78150 = VERTEX_POINT ( 'NONE', #39920 ) ;
#78151 = VERTEX_POINT ( 'NONE', #70652 ) ;
#78152 = ADVANCED_FACE ( 'NONE', ( #29448 ), #51034, .T. ) ;
#78153 = DIRECTION ( 'NONE',  ( 0.000000000000000000, 1.000000000000000000, 0.000000000000000000 ) ) ;
#78154 = EDGE_LOOP ( 'NONE', ( #39662, #11210 ) ) ;
#78155 = ORIENTED_EDGE ( 'NONE', *, *, #121136, .T. ) ;
#78156 = AXIS2_PLACEMENT_3D ( 'NONE', #55679, #87709, #96888 ) ;
#78157 = CARTESIAN_POINT ( 'NONE',  ( 9.599999999999914380, 12.50000000000000000, -5.022947341949754119 ) ) ;
#78158 = EDGE_CURVE ( 'NONE', #79022, #107927, #82097, .T. ) ;
#78159 = CARTESIAN_POINT ( 'NONE',  ( 11.24999999999994493, 2.500000000000000000, -2.265063509461101798 ) ) ;
#78160 = DIRECTION ( 'NONE',  ( -0.000000000000000000, 1.000000000000000000, -0.000000000000000000 ) ) ;
#78161 = CARTESIAN_POINT ( 'NONE',  ( -0.6500000000000389910, 12.50000000000000000, -6.083687093685488989 ) ) ;
#78162 = DIRECTION ( 'NONE',  ( -0.000000000000000000, -1.000000000000000000, -0.000000000000000000 ) ) ;
#78163 = ORIENTED_EDGE ( 'NONE', *, *, #70668, .T. ) ;
#78164 = DIRECTION ( 'NONE',  ( -4.274815082592931898E-19, -0.9999939076577903929, -0.003490651415223739937 ) ) ;
#78165 = VECTOR ( 'NONE', #99016, 1000.000000000000000 ) ;
#78166 = AXIS2_PLACEMENT_3D ( 'NONE', #93043, #3995, #112681 ) ;
#78167 = VERTEX_POINT ( 'NONE', #28155 ) ;
#78168 = CARTESIAN_POINT ( 'NONE',  ( -11.89999999999999680, 2.500000000000000000, -4.083716857408424161 ) ) ;
#78169 = VERTEX_POINT ( 'NONE', #68068 ) ;
#78170 = DIRECTION ( 'NONE',  ( -0.000000000000000000, -1.000000000000000000, -0.000000000000000000 ) ) ;
#78171 = CARTESIAN_POINT ( 'NONE',  ( -3.750000000000025757, 12.50000000000000000, 1.537336459617582918 ) ) ;
#78172 = ORIENTED_EDGE ( 'NONE', *, *, #21384, .F. ) ;
#78173 = DIRECTION ( 'NONE',  ( 0.000000000000000000, 0.000000000000000000, 1.000000000000000000 ) ) ;
#78175 = AXIS2_PLACEMENT_3D ( 'NONE', #86915, #116373, #14924 ) ;
#78174 = DIRECTION ( 'NONE',  ( 0.000000000000000000, -0.000000000000000000, 1.000000000000000000 ) ) ;
#78176 = ORIENTED_EDGE ( 'NONE', *, *, #105794, .T. ) ;
#78177 = CIRCLE ( 'NONE', #13303, 0.09999999999999982514 ) ;
#78178 = VECTOR ( 'NONE', #12741, 1000.000000000000000 ) ;
#78179 = AXIS2_PLACEMENT_3D ( 'NONE', #45531, #35703, #57275 ) ;
#78180 = DIRECTION ( 'NONE',  ( 0.000000000000000000, 0.000000000000000000, 1.000000000000000000 ) ) ;
#78181 = ORIENTED_EDGE ( 'NONE', *, *, #27350, .F. ) ;
#78182 = VERTEX_POINT ( 'NONE', #129603 ) ;
#78183 = CARTESIAN_POINT ( 'NONE',  ( -3.100000000000028511, 12.50000000000000000, 0.3464101615137736845 ) ) ;
#78184 = DIRECTION ( 'NONE',  ( 0.000000000000000000, 0.000000000000000000, 1.000000000000000000 ) ) ;
#78185 = CARTESIAN_POINT ( 'NONE',  ( 183.9010416670080588, -4.367472073101519747, 7.564683531249999149 ) ) ;
#78186 = AXIS2_PLACEMENT_3D ( 'NONE', #5646, #76984, #65869 ) ;
#78187 = DIRECTION ( 'NONE',  ( -0.000000000000000000, 1.000000000000000000, -0.000000000000000000 ) ) ;
#78188 = EDGE_CURVE ( 'NONE', #36304, #8747, #2658, .T. ) ;
#78189 = PLANE ( 'NONE',  #60454 ) ;
#78190 = CONICAL_SURFACE ( 'NONE', #53052, 0.09999999999999982514, 0.003490658503988666988 ) ;
#78191 = VECTOR ( 'NONE', #108677, 1000.000000000000000 ) ;
#78192 = VECTOR ( 'NONE', #89813, 1000.000000000000000 ) ;
#78193 = DIRECTION ( 'NONE',  ( 0.000000000000000000, -0.000000000000000000, 1.000000000000000000 ) ) ;
#78194 = AXIS2_PLACEMENT_3D ( 'NONE', #38174, #69554, #17203 ) ;
#78195 = VERTEX_POINT ( 'NONE', #49745 ) ;
#78196 = CIRCLE ( 'NONE', #38591, 0.06509327318403745899 ) ;
#78197 = DIRECTION ( 'NONE',  ( 0.000000000000000000, 0.000000000000000000, 1.000000000000000000 ) ) ;
#78198 = CARTESIAN_POINT ( 'NONE',  ( 1.649999999999951505, 2.500000000000000000, -2.757883832488654097 ) ) ;
#78199 = ORIENTED_EDGE ( 'NONE', *, *, #42034, .F. ) ;
#78200 = ADVANCED_FACE ( 'NONE', ( #90943 ), #71631, .T. ) ;
#78201 = DIRECTION ( 'NONE',  ( 0.000000000000000000, 1.000000000000000000, 0.000000000000000000 ) ) ;
#78202 = DIRECTION ( 'NONE',  ( 0.000000000000000000, 0.000000000000000000, 1.000000000000000000 ) ) ;
#78203 = DIRECTION ( 'NONE',  ( 0.000000000000000000, -0.9999939076577903929, 0.003490651415223739937 ) ) ;
#78204 = EDGE_CURVE ( 'NONE', #60586, #129244, #84135, .T. ) ;
#78205 = CARTESIAN_POINT ( 'NONE',  ( 10.79999999999991367, 2.500000000000000000, 0.09999999999999761857 ) ) ;
#78206 = CARTESIAN_POINT ( 'NONE',  ( 0.8499999999999553468, 12.50000000000000000, -2.165063509461101710 ) ) ;
#78207 = ORIENTED_EDGE ( 'NONE', *, *, #81972, .F. ) ;
#78208 = DIRECTION ( 'NONE',  ( 0.000000000000000000, 0.000000000000000000, -1.000000000000000000 ) ) ;
#78209 = SURFACE_SIDE_STYLE ('',( #117440 ) ) ;
#78210 = AXIS2_PLACEMENT_3D ( 'NONE', #42437, #71900, #1845 ) ;
#78211 = CONICAL_SURFACE ( 'NONE', #21683, 0.1000000000000002554, 0.003490658503988666988 ) ;
#78212 = VECTOR ( 'NONE', #109157, 1000.000000000000000 ) ;
#78213 = EDGE_CURVE ( 'NONE', #123206, #91215, #33984, .T. ) ;
#78214 = ORIENTED_EDGE ( 'NONE', *, *, #13191, .T. ) ;
#78215 = DIRECTION ( 'NONE',  ( 0.000000000000000000, 1.000000000000000000, 0.000000000000000000 ) ) ;
#78216 = CIRCLE ( 'NONE', #71962, 0.1000000000000000472 ) ;
#78217 = CIRCLE ( 'NONE', #51037, 0.06509327318403741736 ) ;
#78218 = ORIENTED_EDGE ( 'NONE', *, *, #11416, .T. ) ;
#78219 = VECTOR ( 'NONE', #27787, 1000.000000000000000 ) ;
#78220 = EDGE_LOOP ( 'NONE', ( #79333, #63326 ) ) ;
#78221 = DIRECTION ( 'NONE',  ( 0.000000000000000000, 0.000000000000000000, 1.000000000000000000 ) ) ;
#78222 = VECTOR ( 'NONE', #29840, 1000.000000000000000 ) ;
#78223 = ORIENTED_EDGE ( 'NONE', *, *, #119633, .F. ) ;
#78224 = DIRECTION ( 'NONE',  ( 0.000000000000000000, 0.000000000000000000, 1.000000000000000000 ) ) ;
#78225 = CARTESIAN_POINT ( 'NONE',  ( 12.49999999999993960, 2.500000000000000000, 4.230127018922196669 ) ) ;
#78226 = DIRECTION ( 'NONE',  ( 0.000000000000000000, 0.000000000000000000, -1.000000000000000000 ) ) ;
#78228 = EDGE_LOOP ( 'NONE', ( #52886, #16362 ) ) ;
#78227 = AXIS2_PLACEMENT_3D ( 'NONE', #110550, #71936, #61477 ) ;
#78229 = AXIS2_PLACEMENT_3D ( 'NONE', #96173, #3931, #6473 ) ;
#78230 = AXIS2_PLACEMENT_3D ( 'NONE', #12545, #93699, #100927 ) ;
#78231 = DIRECTION ( 'NONE',  ( -0.000000000000000000, -1.000000000000000000, -0.000000000000000000 ) ) ;
#78233 = ORIENTED_EDGE ( 'NONE', *, *, #92673, .F. ) ;
#78232 = DIRECTION ( 'NONE',  ( 0.000000000000000000, 0.000000000000000000, -1.000000000000000000 ) ) ;
#78234 = CONICAL_SURFACE ( 'NONE', #51050, 0.1000000000000000472, 0.003490658503988666988 ) ;
#78235 = LINE ( 'NONE', #19950, #71615 ) ;
#78236 = DIRECTION ( 'NONE',  ( 0.000000000000000000, -0.9999939076577903929, 0.003490651415223739937 ) ) ;
#78237 = ORIENTED_EDGE ( 'NONE', *, *, #2090, .T. ) ;
#78238 = EDGE_CURVE ( 'NONE', #66570, #54324, #48658, .T. ) ;
#78239 = ORIENTED_EDGE ( 'NONE', *, *, #3121, .F. ) ;
#78240 = ORIENTED_EDGE ( 'NONE', *, *, #55455, .T. ) ;
#78241 = CARTESIAN_POINT ( 'NONE',  ( 12.69999999999990337, 2.500000000000000000, -4.676537180435978769 ) ) ;
#78242 = CARTESIAN_POINT ( 'NONE',  ( 8.349999999999919709, 2.500000000000000000, -1.372243186433550033 ) ) ;
#78243 = FACE_OUTER_BOUND ( 'NONE', #103891, .T. ) ;
#78244 = EDGE_CURVE ( 'NONE', #68434, #123664, #88333, .T. ) ;
#78245 = FACE_BOUND ( 'NONE', #57483, .T. ) ;
#78246 = ORIENTED_EDGE ( 'NONE', *, *, #70570, .T. ) ;
#78247 = EDGE_CURVE ( 'NONE', #112782, #29210, #15174, .T. ) ;
#78248 = ADVANCED_FACE ( 'NONE', ( #3843 ), #72599, .T. ) ;
#78249 = DIRECTION ( 'NONE',  ( 0.000000000000000000, 0.000000000000000000, 1.000000000000000000 ) ) ;
#78250 = CARTESIAN_POINT ( 'NONE',  ( -8.100000000000010303, 2.500000000000000000, 4.576537180435972019 ) ) ;
#78251 = AXIS2_PLACEMENT_3D ( 'NONE', #56315, #15743, #67402 ) ;
#78252 = ORIENTED_EDGE ( 'NONE', *, *, #87201, .T. ) ;
#78253 = LINE ( 'NONE', #118800, #96708 ) ;
#78254 = DIRECTION ( 'NONE',  ( -4.274815082592931898E-19, -0.9999939076577903929, -0.003490651415223739937 ) ) ;
#78255 = ADVANCED_FACE ( 'NONE', ( #121678 ), #32695, .T. ) ;
#78256 = DIRECTION ( 'NONE',  ( 0.000000000000000000, 0.000000000000000000, -1.000000000000000000 ) ) ;
#78257 = LINE ( 'NONE', #99177, #73879 ) ;
#78258 = EDGE_CURVE ( 'NONE', #98580, #84166, #51675, .T. ) ;
#78259 = DIRECTION ( 'NONE',  ( 0.000000000000000000, 0.000000000000000000, 1.000000000000000000 ) ) ;
#78260 = EDGE_CURVE ( 'NONE', #107580, #30611, #42400, .T. ) ;
#78261 = FACE_OUTER_BOUND ( 'NONE', #8613, .T. ) ;
#78262 = CARTESIAN_POINT ( 'NONE',  ( -10.20000000000000462, 12.50000000000000000, -4.676537180435973440 ) ) ;
#78263 = CIRCLE ( 'NONE', #55270, 0.09999999999999982514 ) ;
#78264 = CONICAL_SURFACE ( 'NONE', #128447, 0.1000000000000002554, 0.003490658503988666988 ) ;
#78265 = EDGE_CURVE ( 'NONE', #4566, #40462, #91585, .T. ) ;
#78266 = ORIENTED_EDGE ( 'NONE', *, *, #91256, .F. ) ;
#78267 = EDGE_LOOP ( 'NONE', ( #108973, #28783, #105947, #57432 ) ) ;
#78268 = ORIENTED_EDGE ( 'NONE', *, *, #98807, .F. ) ;
#78269 = ORIENTED_EDGE ( 'NONE', *, *, #101197, .T. ) ;
#78270 = ORIENTED_EDGE ( 'NONE', *, *, #72897, .T. ) ;
#78271 = CARTESIAN_POINT ( 'NONE',  ( -12.09999999999999609, 12.50000000000000000, -3.637306695894647390 ) ) ;
#78272 = LINE ( 'NONE', #37692, #42607 ) ;
#78273 = ORIENTED_EDGE ( 'NONE', *, *, #47915, .F. ) ;
#78274 = EDGE_CURVE ( 'NONE', #41297, #27877, #17222, .T. ) ;
#78275 = FACE_BOUND ( 'NONE', #119509, .T. ) ;
#78276 = EDGE_CURVE ( 'NONE', #26093, #24306, #1905, .T. ) ;
#78277 = CARTESIAN_POINT ( 'NONE',  ( -2.500000000000030642, 12.50000000000000000, -0.7579135962115916003 ) ) ;
#78278 = CIRCLE ( 'NONE', #59510, 0.06509327318403741736 ) ;
#78279 = FACE_OUTER_BOUND ( 'NONE', #3721, .T. ) ;
#78280 = DIRECTION ( 'NONE',  ( 0.000000000000000000, 1.000000000000000000, 0.000000000000000000 ) ) ;
#78281 = DIRECTION ( 'NONE',  ( -0.000000000000000000, -1.000000000000000000, -0.000000000000000000 ) ) ;
#78282 = CARTESIAN_POINT ( 'NONE',  ( -3.350000000000031619, 12.50000000000000000, -5.802370205355749988 ) ) ;
#78283 = VERTEX_POINT ( 'NONE', #2539 ) ;
#78284 = DIRECTION ( 'NONE',  ( 0.000000000000000000, -0.9999939076577903929, 0.003490651415223739937 ) ) ;
#78285 = VERTEX_POINT ( 'NONE', #102680 ) ;
#78286 = VECTOR ( 'NONE', #13814, 1000.000000000000000 ) ;
#78287 = CONICAL_SURFACE ( 'NONE', #44834, 0.1000000000000000472, 0.003490658503988666988 ) ;
#78288 = EDGE_LOOP ( 'NONE', ( #106025, #26295 ) ) ;
#78289 = VERTEX_POINT ( 'NONE', #33959 ) ;
#78290 = DIRECTION ( 'NONE',  ( 0.000000000000000000, 0.000000000000000000, -1.000000000000000000 ) ) ;
#78291 = DIRECTION ( 'NONE',  ( 0.000000000000000000, 0.000000000000000000, 1.000000000000000000 ) ) ;
#78293 = VECTOR ( 'NONE', #56355, 1000.000000000000000 ) ;
#78292 = CARTESIAN_POINT ( 'NONE',  ( 12.49999999999993960, 2.500000000000000000, 4.430127018922196847 ) ) ;
#78294 = VERTEX_POINT ( 'NONE', #42502 ) ;
#78295 = FACE_OUTER_BOUND ( 'NONE', #90319, .T. ) ;
#78296 = AXIS2_PLACEMENT_3D ( 'NONE', #82095, #122030, #89972 ) ;
#78297 = CARTESIAN_POINT ( 'NONE',  ( 4.349999999999936584, 2.500000000000000000, 6.048780366869520364 ) ) ;
#78298 = DIRECTION ( 'NONE',  ( 0.000000000000000000, 1.000000000000000000, 0.000000000000000000 ) ) ;
#78299 = CARTESIAN_POINT ( 'NONE',  ( 186.1510416670080588, 4.367472073101518859, -7.564683531249999149 ) ) ;
#78300 = DIRECTION ( 'NONE',  ( 0.000000000000000000, 0.000000000000000000, -1.000000000000000000 ) ) ;
#78301 = CARTESIAN_POINT ( 'NONE',  ( 7.899999999999924860, 12.50000000000000000, -5.088040615133791356 ) ) ;
#78302 = CARTESIAN_POINT ( 'NONE',  ( -5.000000000000024869, 12.50000000000000000, -5.022947341949754119 ) ) ;
#78303 = ORIENTED_EDGE ( 'NONE', *, *, #123019, .T. ) ;
#78304 = DIRECTION ( 'NONE',  ( 0.000000000000000000, 0.000000000000000000, 1.000000000000000000 ) ) ;
#78305 = EDGE_LOOP ( 'NONE', ( #56971, #82477 ) ) ;
#78306 = EDGE_CURVE ( 'NONE', #68006, #68510, #92561, .T. ) ;
#78308 = ORIENTED_EDGE ( 'NONE', *, *, #3024, .F. ) ;
#78307 = CIRCLE ( 'NONE', #103625, 0.09999999999999982514 ) ;
#78309 = DIRECTION ( 'NONE',  ( -0.000000000000000000, 1.000000000000000000, -0.000000000000000000 ) ) ;
#78310 = AXIS2_PLACEMENT_3D ( 'NONE', #9590, #118897, #29875 ) ;
#78311 = ADVANCED_FACE ( 'NONE', ( #12998 ), #27709, .T. ) ;
#78312 = DIRECTION ( 'NONE',  ( 0.000000000000000000, 1.000000000000000000, 0.000000000000000000 ) ) ;
#78313 = CONICAL_SURFACE ( 'NONE', #11484, 0.09999999999999982514, 0.003490658503988666988 ) ;
#78314 = CARTESIAN_POINT ( 'NONE',  ( 1.649999999999948841, 2.500000000000000000, 6.395190528383296602 ) ) ;
#78315 = VERTEX_POINT ( 'NONE', #23484 ) ;
#78316 = ORIENTED_EDGE ( 'NONE', *, *, #45128, .T. ) ;
#78317 = CARTESIAN_POINT ( 'NONE',  ( 6.449999999999931788, 2.500000000000000000, -6.248780366869526759 ) ) ;
#78318 = AXIS2_PLACEMENT_3D ( 'NONE', #18372, #40628, #128361 ) ;
#78319 = CIRCLE ( 'NONE', #21882, 0.06509327318403741736 ) ;
#78320 = PLANE ( 'NONE',  #28646 ) ;
#78321 = DIRECTION ( 'NONE',  ( 1.000000000000000000, 0.000000000000000000, 0.000000000000000000 ) ) ;
#78322 = ORIENTED_EDGE ( 'NONE', *, *, #237, .F. ) ;
#78323 = EDGE_LOOP ( 'NONE', ( #102956, #9844 ) ) ;
#78324 = AXIS2_PLACEMENT_3D ( 'NONE', #128269, #98780, #66743 ) ;
#78325 = LINE ( 'NONE', #129367, #100454 ) ;
#78326 = ORIENTED_EDGE ( 'NONE', *, *, #59037, .F. ) ;
#78327 = DIRECTION ( 'NONE',  ( 0.000000000000000000, 0.000000000000000000, -1.000000000000000000 ) ) ;
#78328 = AXIS2_PLACEMENT_3D ( 'NONE', #77822, #128897, #99427 ) ;
#78329 = CIRCLE ( 'NONE', #82530, 0.06509327318403745899 ) ;
#78330 = DIRECTION ( 'NONE',  ( -4.274815082592931898E-19, -0.9999939076577903929, -0.003490651415223739937 ) ) ;
#78331 = EDGE_LOOP ( 'NONE', ( #7545, #48635, #109251, #128398 ) ) ;
#78332 = DIRECTION ( 'NONE',  ( -4.274815082592931898E-19, -0.9999939076577903929, -0.003490651415223739937 ) ) ;
#78333 = DIRECTION ( 'NONE',  ( 0.000000000000000000, 0.000000000000000000, -1.000000000000000000 ) ) ;
#78334 = CARTESIAN_POINT ( 'NONE',  ( 187.5000000000000000, 0.000000000000000000, 0.000000000000000000 ) ) ;
#78335 = DIRECTION ( 'NONE',  ( -0.000000000000000000, -1.000000000000000000, -0.000000000000000000 ) ) ;
#78336 = VERTEX_POINT ( 'NONE', #64058 ) ;
#78337 = LINE ( 'NONE', #17442, #121991 ) ;
#78338 = ORIENTED_EDGE ( 'NONE', *, *, #31447, .T. ) ;
#78339 = ORIENTED_EDGE ( 'NONE', *, *, #124329, .T. ) ;
#78340 = DIRECTION ( 'NONE',  ( 0.000000000000000000, 1.000000000000000000, 0.000000000000000000 ) ) ;
#78341 = DIRECTION ( 'NONE',  ( 0.000000000000000000, 0.000000000000000000, -1.000000000000000000 ) ) ;
#78342 = DIRECTION ( 'NONE',  ( 0.000000000000000000, 1.000000000000000000, 0.000000000000000000 ) ) ;
#78343 = DIRECTION ( 'NONE',  ( 0.000000000000000000, 1.000000000000000000, 0.000000000000000000 ) ) ;
#78344 = AXIS2_PLACEMENT_3D ( 'NONE', #20064, #96343, #105544 ) ;
#78345 = DIRECTION ( 'NONE',  ( 0.000000000000000000, 1.000000000000000000, 0.000000000000000000 ) ) ;
#78346 = DIRECTION ( 'NONE',  ( -0.000000000000000000, -1.000000000000000000, -0.000000000000000000 ) ) ;
#78347 = EDGE_CURVE ( 'NONE', #83000, #74312, #14296, .T. ) ;
#78348 = DIRECTION ( 'NONE',  ( 0.000000000000000000, -0.000000000000000000, 1.000000000000000000 ) ) ;
#78349 = CARTESIAN_POINT ( 'NONE',  ( 7.899999999999924860, 12.50000000000000000, 3.637306695894644726 ) ) ;
#78350 = LINE ( 'NONE', #80276, #33828 ) ;
#78352 = CIRCLE ( 'NONE', #118041, 0.1000000000000000472 ) ;
#78351 = DIRECTION ( 'NONE',  ( -0.000000000000000000, -1.000000000000000000, -0.000000000000000000 ) ) ;
#78353 = ADVANCED_FACE ( 'NONE', ( #44415 ), #514, .T. ) ;
#78354 = CONICAL_SURFACE ( 'NONE', #94977, 0.09999999999999999167, 0.003490658503988666988 ) ;
#78355 = ORIENTED_EDGE ( 'NONE', *, *, #40578, .F. ) ;
#78356 = DIRECTION ( 'NONE',  ( 0.000000000000000000, 0.000000000000000000, 1.000000000000000000 ) ) ;
#78357 = ADVANCED_FACE ( 'NONE', ( #54242 ), #123606, .T. ) ;
#78358 = CARTESIAN_POINT ( 'NONE',  ( -5.000000000000022204, 2.500000000000000000, 3.637306695894644726 ) ) ;
#78360 = EDGE_CURVE ( 'NONE', #79693, #54054, #4708, .T. ) ;
#78359 = LINE ( 'NONE', #7653, #72607 ) ;
#78361 = PLANE ( 'NONE',  #60960 ) ;
#78362 = CARTESIAN_POINT ( 'NONE',  ( -2.900000000000030553, 12.50000000000000000, 4.957854068765711553 ) ) ;
#78363 = ORIENTED_EDGE ( 'NONE', *, *, #64795, .F. ) ;
#78364 = DIRECTION ( 'NONE',  ( -0.000000000000000000, -1.000000000000000000, -0.000000000000000000 ) ) ;
#78365 = AXIS2_PLACEMENT_3D ( 'NONE', #118614, #88500, #38801 ) ;
#78366 = EDGE_CURVE ( 'NONE', #29851, #2948, #115625, .T. ) ;
#78367 = CIRCLE ( 'NONE', #69949, 0.06509327318403745899 ) ;
#78368 = DIRECTION ( 'NONE',  ( 0.000000000000000000, 1.000000000000000000, 0.000000000000000000 ) ) ;
#78370 = EDGE_LOOP ( 'NONE', ( #55753, #128377 ) ) ;
#78369 = DIRECTION ( 'NONE',  ( -4.274815082592931898E-19, -0.9999939076577903929, -0.003490651415223739937 ) ) ;
#78371 = EDGE_CURVE ( 'NONE', #87315, #60348, #84233, .T. ) ;
#78372 = ORIENTED_EDGE ( 'NONE', *, *, #49018, .F. ) ;
#78373 = DIRECTION ( 'NONE',  ( 0.000000000000000000, 1.000000000000000000, 0.000000000000000000 ) ) ;
#78374 = VECTOR ( 'NONE', #87070, 1000.000000000000000 ) ;
#78375 = CONICAL_SURFACE ( 'NONE', #116010, 0.09999999999999982514, 0.003490658503988666988 ) ;
#78376 = ORIENTED_EDGE ( 'NONE', *, *, #58726, .F. ) ;
#78377 = ORIENTED_EDGE ( 'NONE', *, *, #28699, .F. ) ;
#78378 = ORIENTED_EDGE ( 'NONE', *, *, #123420, .F. ) ;
#78379 = CARTESIAN_POINT ( 'NONE',  ( 8.349999999999923261, 2.500000000000000000, 1.372243186433545370 ) ) ;
#78380 = CONICAL_SURFACE ( 'NONE', #111525, 0.09999999999999999167, 0.003490658503988666988 ) ;
#78381 = DIRECTION ( 'NONE',  ( 0.000000000000000000, 0.000000000000000000, 1.000000000000000000 ) ) ;
#78382 = CARTESIAN_POINT ( 'NONE',  ( -9.200000000000006395, 12.50000000000000000, 4.330127018922196314 ) ) ;
#78383 = CIRCLE ( 'NONE', #88824, 0.06509327318403745899 ) ;
#78384 = DIRECTION ( 'NONE',  ( 0.000000000000000000, 1.000000000000000000, 0.000000000000000000 ) ) ;
#78385 = VERTEX_POINT ( 'NONE', #82430 ) ;
#78386 = DIRECTION ( 'NONE',  ( 0.000000000000000000, 1.000000000000000000, 0.000000000000000000 ) ) ;
#78387 = EDGE_LOOP ( 'NONE', ( #41997, #90187, #52711, #25173 ) ) ;
#78388 = DIRECTION ( 'NONE',  ( -0.000000000000000000, 1.000000000000000000, -0.000000000000000000 ) ) ;
#78389 = CARTESIAN_POINT ( 'NONE',  ( 17.29982614914525740, -2.489966891809380911, -2.989943721786608943 ) ) ;
#78390 = FACE_OUTER_BOUND ( 'NONE', #119254, .T. ) ;
#78391 = CARTESIAN_POINT ( 'NONE',  ( -11.05000000000000071, 2.500000000000000000, 6.841600689897072485 ) ) ;
#78392 = CARTESIAN_POINT ( 'NONE',  ( 9.549999999999915445, 2.500000000000000000, -2.165063509461101710 ) ) ;
#78393 = ORIENTED_EDGE ( 'NONE', *, *, #74734, .T. ) ;
#78394 = EDGE_CURVE ( 'NONE', #2954, #72494, #33333, .T. ) ;
#78395 = CIRCLE ( 'NONE', #38699, 0.06509327318403745899 ) ;
#78396 = VERTEX_POINT ( 'NONE', #83705 ) ;
#78397 = ORIENTED_EDGE ( 'NONE', *, *, #116187, .T. ) ;
#78398 = AXIS2_PLACEMENT_3D ( 'NONE', #86190, #126135, #76402 ) ;
#78399 = ORIENTED_EDGE ( 'NONE', *, *, #58048, .F. ) ;
#78400 = EDGE_LOOP ( 'NONE', ( #29955, #104588 ) ) ;
#78401 = LINE ( 'NONE', #127492, #92187 ) ;
#78402 = CARTESIAN_POINT ( 'NONE',  ( -10.65000000000000213, 12.50000000000000000, 6.213873640053558134 ) ) ;
#78403 = CIRCLE ( 'NONE', #19906, 0.1000000000000000472 ) ;
#78404 = DIRECTION ( 'NONE',  ( 0.000000000000000000, 0.000000000000000000, 1.000000000000000000 ) ) ;
#78405 = EDGE_CURVE ( 'NONE', #13448, #70324, #27800, .T. ) ;
#78406 = FACE_BOUND ( 'NONE', #25572, .T. ) ;
#78407 = DIRECTION ( 'NONE',  ( 0.000000000000000000, 0.000000000000000000, 1.000000000000000000 ) ) ;
#78408 = DIRECTION ( 'NONE',  ( 0.000000000000000000, -0.000000000000000000, 1.000000000000000000 ) ) ;
#78409 = EDGE_CURVE ( 'NONE', #55871, #121543, #71422, .T. ) ;
#78410 = CARTESIAN_POINT ( 'NONE',  ( -4.800000000000022915, 12.50000000000000000, 3.918623584224382839 ) ) ;
#78411 = DIRECTION ( 'NONE',  ( 0.000000000000000000, 0.000000000000000000, 1.000000000000000000 ) ) ;
#78412 = AXIS2_PLACEMENT_3D ( 'NONE', #116283, #116925, #5043 ) ;
#78413 = CONICAL_SURFACE ( 'NONE', #90911, 0.1000000000000000472, 0.003490658503988666988 ) ;
#78414 = AXIS2_PLACEMENT_3D ( 'NONE', #113568, #44174, #16631 ) ;
#78415 = ADVANCED_FACE ( 'NONE', ( #126199 ), #96723, .T. ) ;
#78416 = CARTESIAN_POINT ( 'NONE',  ( 184.7552083336747444, 6.551208109652275624, -3.782341765624998686 ) ) ;
#78417 = AXIS2_PLACEMENT_3D ( 'NONE', #75128, #52917, #92850 ) ;
#78418 = ADVANCED_FACE ( 'NONE', ( #95455 ), #111129, .T. ) ;
#78419 = DIRECTION ( 'NONE',  ( 0.000000000000000000, 0.000000000000000000, 1.000000000000000000 ) ) ;
#78420 = EDGE_CURVE ( 'NONE', #120360, #41032, #59227, .T. ) ;
#78421 = DIRECTION ( 'NONE',  ( 0.000000000000000000, -0.9999939076577903929, 0.003490651415223739937 ) ) ;
#78422 = ADVANCED_FACE ( 'NONE', ( #106550 ), #25447, .T. ) ;
#78423 = VECTOR ( 'NONE', #37757, 1000.000000000000000 ) ;
#78424 = AXIS2_PLACEMENT_3D ( 'NONE', #72954, #34335, #113511 ) ;
#78425 = DIRECTION ( 'NONE',  ( 0.000000000000000000, -0.000000000000000000, 1.000000000000000000 ) ) ;
#78426 = ADVANCED_FACE ( 'NONE', ( #36551 ), #14971, .T. ) ;
#78427 = EDGE_LOOP ( 'NONE', ( #68960, #46608 ) ) ;
#78428 = VERTEX_POINT ( 'NONE', #107193 ) ;
#78429 = EDGE_LOOP ( 'NONE', ( #60589, #8515 ) ) ;
#78430 = EDGE_LOOP ( 'NONE', ( #61966, #93846 ) ) ;
#78431 = AXIS2_PLACEMENT_3D ( 'NONE', #74156, #44696, #25048 ) ;
#78432 = CARTESIAN_POINT ( 'NONE',  ( -8.150000000000012790, 2.500000000000000000, -1.718653347947326049 ) ) ;
#78433 = FACE_OUTER_BOUND ( 'NONE', #122479, .T. ) ;
#78434 = FACE_BOUND ( 'NONE', #2093, .T. ) ;
#78435 = EDGE_CURVE ( 'NONE', #77344, #17860, #92659, .T. ) ;
#78436 = CARTESIAN_POINT ( 'NONE',  ( 2.500000000000002220, -2.500000000000000000, 9.000000000000001776 ) ) ;
#78437 = ORIENTED_EDGE ( 'NONE', *, *, #116175, .F. ) ;
#78438 = DIRECTION ( 'NONE',  ( 0.000000000000000000, 0.000000000000000000, -1.000000000000000000 ) ) ;
#78439 = DIRECTION ( 'NONE',  ( 0.000000000000000000, 0.000000000000000000, -1.000000000000000000 ) ) ;
#78440 = DIRECTION ( 'NONE',  ( 0.000000000000000000, 0.000000000000000000, 1.000000000000000000 ) ) ;
#78441 = DIRECTION ( 'NONE',  ( 0.000000000000000000, 0.000000000000000000, 1.000000000000000000 ) ) ;
#78443 = VERTEX_POINT ( 'NONE', #94807 ) ;
#78442 = CONICAL_SURFACE ( 'NONE', #70019, 0.09999999999999982514, 0.003490658503988666988 ) ;
#78444 = CARTESIAN_POINT ( 'NONE',  ( 12.49999999999990230, 12.50000000000000000, -0.6928203230275541413 ) ) ;
#78445 = ORIENTED_EDGE ( 'NONE', *, *, #3345, .F. ) ;
#78446 = ORIENTED_EDGE ( 'NONE', *, *, #43528, .F. ) ;
#78447 = DIRECTION ( 'NONE',  ( 0.000000000000000000, 0.000000000000000000, 1.000000000000000000 ) ) ;
#78448 = DIRECTION ( 'NONE',  ( 0.000000000000000000, 0.000000000000000000, 1.000000000000000000 ) ) ;
#78449 = EDGE_LOOP ( 'NONE', ( #93747, #3094, #32991, #125320 ) ) ;
#78450 = VECTOR ( 'NONE', #121404, 1000.000000000000000 ) ;
#78451 = VECTOR ( 'NONE', #106555, 1000.000000000000000 ) ;
#78452 = CARTESIAN_POINT ( 'NONE',  ( 6.449999999999931788, 12.50000000000000000, 6.148780366869520009 ) ) ;
#78453 = CARTESIAN_POINT ( 'NONE',  ( -14.39999999999998614, 2.500000000000000000, 0.2464101615137758439 ) ) ;
#78454 = ORIENTED_EDGE ( 'NONE', *, *, #29397, .T. ) ;
#78455 = CARTESIAN_POINT ( 'NONE',  ( 13.14999999999990088, 12.50000000000000000, 2.511473670974873507 ) ) ;
#78456 = ORIENTED_EDGE ( 'NONE', *, *, #33682, .F. ) ;
#78457 = DIRECTION ( 'NONE',  ( 0.000000000000000000, 0.000000000000000000, 1.000000000000000000 ) ) ;
#78458 = EDGE_LOOP ( 'NONE', ( #70325, #128130, #100191, #120944 ) ) ;
#78459 = DIRECTION ( 'NONE',  ( 0.000000000000000000, 0.000000000000000000, 1.000000000000000000 ) ) ;
#78460 = FACE_BOUND ( 'NONE', #55061, .T. ) ;
#78461 = AXIS2_PLACEMENT_3D ( 'NONE', #25549, #94967, #96878 ) ;
#78462 = EDGE_LOOP ( 'NONE', ( #125909, #34764 ) ) ;
#78463 = EDGE_CURVE ( 'NONE', #48770, #71603, #40353, .T. ) ;
#78465 = CARTESIAN_POINT ( 'NONE',  ( 112.3162792014981619, 7.273147445303300707, -2.544068225761106472 ) ) ;
#78464 = AXIS2_PLACEMENT_3D ( 'NONE', #112556, #81159, #121077 ) ;
#78466 = VERTEX_POINT ( 'NONE', #75170 ) ;
#78467 = CARTESIAN_POINT ( 'NONE',  ( 0.6499999999999561684, 2.500000000000000000, 1.818653347947321475 ) ) ;
#78468 = CARTESIAN_POINT ( 'NONE',  ( -2.700000000000030376, 2.500000000000000000, 4.083716857408421497 ) ) ;
#78469 = CARTESIAN_POINT ( 'NONE',  ( 10.19999999999991580, 2.500000000000000000, -0.3464101615137783474 ) ) ;
#78470 = DIRECTION ( 'NONE',  ( 0.000000000000000000, 1.000000000000000000, 0.000000000000000000 ) ) ;
#78471 = DIRECTION ( 'NONE',  ( -0.000000000000000000, -1.000000000000000000, -0.000000000000000000 ) ) ;
#78472 = ORIENTED_EDGE ( 'NONE', *, *, #47074, .F. ) ;
#78473 = EDGE_LOOP ( 'NONE', ( #72109, #46407, #62712, #91992 ) ) ;
#78474 = ADVANCED_FACE ( 'NONE', ( #115067 ), #123943, .T. ) ;
#78475 = ORIENTED_EDGE ( 'NONE', *, *, #101435, .F. ) ;
#78476 = DIRECTION ( 'NONE',  ( -0.000000000000000000, 1.000000000000000000, -0.000000000000000000 ) ) ;
#78477 = VECTOR ( 'NONE', #53302, 1000.000000000000000 ) ;
#78478 = CIRCLE ( 'NONE', #22033, 0.1000000000000002554 ) ;
#78479 = CARTESIAN_POINT ( 'NONE',  ( 8.749999999999921840, 12.50000000000000000, 2.857883832488649301 ) ) ;
#78480 = CARTESIAN_POINT ( 'NONE',  ( 12.69999999999990159, 12.50000000000000000, -3.983716857408426293 ) ) ;
#78482 = EDGE_LOOP ( 'NONE', ( #72431, #112664, #386, #69579 ) ) ;
#78481 = VERTEX_POINT ( 'NONE', #37189 ) ;
#78483 = ORIENTED_EDGE ( 'NONE', *, *, #85001, .F. ) ;
#78484 = DIRECTION ( 'NONE',  ( 0.000000000000000000, 0.000000000000000000, -1.000000000000000000 ) ) ;
#78485 = CARTESIAN_POINT ( 'NONE',  ( 1.449999999999952216, 12.50000000000000000, -2.511473670974877948 ) ) ;
#78486 = DIRECTION ( 'NONE',  ( -0.000000000000000000, -1.000000000000000000, -0.000000000000000000 ) ) ;
#78487 = CARTESIAN_POINT ( 'NONE',  ( -5.200000000000024158, 12.50000000000000000, -4.676537180435977881 ) ) ;
#78488 = VECTOR ( 'NONE', #23372, 1000.000000000000000 ) ;
#78489 = DIRECTION ( 'NONE',  ( -0.000000000000000000, 1.000000000000000000, -0.000000000000000000 ) ) ;
#78490 = CARTESIAN_POINT ( 'NONE',  ( -11.64999999999999680, 12.50000000000000000, -6.495190528383298911 ) ) ;
#78491 = FACE_OUTER_BOUND ( 'NONE', #38910, .T. ) ;
#78492 = AXIS2_PLACEMENT_3D ( 'NONE', #117723, #86338, #126285 ) ;
#78493 = CARTESIAN_POINT ( 'NONE',  ( 10.19999999999991402, 2.500000000000000000, 0.3464101615137735735 ) ) ;
#78494 = ORIENTED_EDGE ( 'NONE', *, *, #12907, .T. ) ;
#78495 = VERTEX_POINT ( 'NONE', #65986 ) ;
#78496 = CARTESIAN_POINT ( 'NONE',  ( -12.89999999999999147, 2.500000000000000000, -0.09999999999999815981 ) ) ;
#78497 = AXIS2_PLACEMENT_3D ( 'NONE', #122291, #32642, #83013 ) ;
#78498 = AXIS2_PLACEMENT_3D ( 'NONE', #105712, #94579, #65112 ) ;
#78499 = DIRECTION ( 'NONE',  ( 0.000000000000000000, 0.000000000000000000, -1.000000000000000000 ) ) ;
#78500 = ORIENTED_EDGE ( 'NONE', *, *, #73991, .T. ) ;
#78501 =( BOUNDED_CURVE ( )  B_SPLINE_CURVE ( 2, ( #123862, #104860, #3458 ),
 .UNSPECIFIED., .F., .F. ) 
 B_SPLINE_CURVE_WITH_KNOTS ( ( 3, 3 ),
 ( 0.000000000000000000, 0.01492713794235515402 ),
 .UNSPECIFIED. ) 
 CURVE ( )  GEOMETRIC_REPRESENTATION_ITEM ( )  RATIONAL_B_SPLINE_CURVE ( ( 0.8943752373141968803, 0.7762344340431479583, 1.000000000000000000 ) ) 
 REPRESENTATION_ITEM ( '' )  );
#78502 = EDGE_LOOP ( 'NONE', ( #64012, #12238 ) ) ;
#78503 = CARTESIAN_POINT ( 'NONE',  ( 187.0260416670080588, -6.551208109652273848, -3.782341765625003571 ) ) ;
#78504 = CARTESIAN_POINT ( 'NONE',  ( -8.150000000000012790, 12.50000000000000000, -1.883746621131363597 ) ) ;
#78505 = DIRECTION ( 'NONE',  ( 0.000000000000000000, 1.000000000000000000, 0.000000000000000000 ) ) ;
#78506 = CONICAL_SURFACE ( 'NONE', #95213, 0.09999999999999982514, 0.003490658503988666988 ) ;
#78507 = DIRECTION ( 'NONE',  ( -0.000000000000000000, 1.000000000000000000, -0.000000000000000000 ) ) ;
#78508 = AXIS2_PLACEMENT_3D ( 'NONE', #117688, #28053, #67961 ) ;
#78509 = AXIS2_PLACEMENT_3D ( 'NONE', #10673, #42102, #2162 ) ;
#78510 = CARTESIAN_POINT ( 'NONE',  ( -12.29999999999999361, 2.500000000000000000, 3.983716857408420076 ) ) ;
#78511 = DIRECTION ( 'NONE',  ( 0.000000000000000000, 0.000000000000000000, 1.000000000000000000 ) ) ;
#78512 = DIRECTION ( 'NONE',  ( -0.000000000000000000, -1.000000000000000000, -0.000000000000000000 ) ) ;
#78513 = AXIS2_PLACEMENT_3D ( 'NONE', #25211, #101857, #12168 ) ;
#78514 = DIRECTION ( 'NONE',  ( 0.000000000000000000, 0.000000000000000000, 1.000000000000000000 ) ) ;
#78515 = AXIS2_PLACEMENT_3D ( 'NONE', #53387, #33735, #84115 ) ;
#78517 = EDGE_CURVE ( 'NONE', #68282, #96334, #121902, .T. ) ;
#78516 = AXIS2_PLACEMENT_3D ( 'NONE', #113357, #52500, #43350 ) ;
#78518 = EDGE_LOOP ( 'NONE', ( #110738, #97042 ) ) ;
#78519 = ORIENTED_EDGE ( 'NONE', *, *, #78889, .F. ) ;
#78520 = AXIS2_PLACEMENT_3D ( 'NONE', #88973, #38604, #7819 ) ;
#78521 = EDGE_CURVE ( 'NONE', #50743, #118622, #31739, .T. ) ;
#78522 = ORIENTED_EDGE ( 'NONE', *, *, #73616, .T. ) ;
#78523 = ORIENTED_EDGE ( 'NONE', *, *, #64015, .F. ) ;
#78524 = EDGE_CURVE ( 'NONE', #59372, #125242, #105168, .T. ) ;
#78525 = CARTESIAN_POINT ( 'NONE',  ( -2.100000000000033840, 12.50000000000000000, 4.957854068765711553 ) ) ;
#78526 = LINE ( 'NONE', #88969, #3903 ) ;
#78527 = VERTEX_POINT ( 'NONE', #56783 ) ;
#78528 = DIRECTION ( 'NONE',  ( 0.000000000000000000, 0.000000000000000000, -1.000000000000000000 ) ) ;
#78529 = FACE_OUTER_BOUND ( 'NONE', #40009, .T. ) ;
#78530 = EDGE_CURVE ( 'NONE', #51256, #82532, #4805, .T. ) ;
#78531 = DIRECTION ( 'NONE',  ( 0.000000000000000000, 0.000000000000000000, 1.000000000000000000 ) ) ;
#78533 = EDGE_LOOP ( 'NONE', ( #74164, #68174 ) ) ;
#78532 = CARTESIAN_POINT ( 'NONE',  ( -2.500000000000032419, 2.500000000000000000, 0.5928203230275495006 ) ) ;
#78534 = EDGE_CURVE ( 'NONE', #51476, #12146, #613, .T. ) ;
#78535 = DIRECTION ( 'NONE',  ( 0.000000000000000000, 1.000000000000000000, 0.000000000000000000 ) ) ;
#78536 = CIRCLE ( 'NONE', #40882, 0.06509327318403745899 ) ;
#78537 = FACE_OUTER_BOUND ( 'NONE', #46733, .T. ) ;
#78538 = EDGE_LOOP ( 'NONE', ( #95274, #6679 ) ) ;
#78539 = ORIENTED_EDGE ( 'NONE', *, *, #12618, .F. ) ;
#78540 = VERTEX_POINT ( 'NONE', #17519 ) ;
#78541 = PLANE ( 'NONE',  #19535 ) ;
#78542 = CIRCLE ( 'NONE', #40891, 0.09999999999999982514 ) ;
#78543 = CIRCLE ( 'NONE', #88985, 0.06509327318403745899 ) ;
#78544 = DIRECTION ( 'NONE',  ( 0.000000000000000000, 1.000000000000000000, 0.000000000000000000 ) ) ;
#78545 = CIRCLE ( 'NONE', #30427, 0.06509327318403745899 ) ;
#78546 = ORIENTED_EDGE ( 'NONE', *, *, #39599, .T. ) ;
#78547 = DIRECTION ( 'NONE',  ( 0.000000000000000000, 1.000000000000000000, 0.000000000000000000 ) ) ;
#78548 = CARTESIAN_POINT ( 'NONE',  ( -3.550000000000028244, 2.500000000000000000, -1.718653347947326049 ) ) ;
#78549 = CARTESIAN_POINT ( 'NONE',  ( -11.04999999999999893, 2.500000000000000000, 6.148780366869520009 ) ) ;
#78550 = DIRECTION ( 'NONE',  ( -0.000000000000000000, -1.000000000000000000, -0.000000000000000000 ) ) ;
#78551 = AXIS2_PLACEMENT_3D ( 'NONE', #87703, #117797, #28153 ) ;
#78552 = ORIENTED_EDGE ( 'NONE', *, *, #3809, .F. ) ;
#78553 = FACE_OUTER_BOUND ( 'NONE', #25142, .T. ) ;
#78554 = AXIS2_PLACEMENT_3D ( 'NONE', #29331, #59449, #9677 ) ;
#78555 = ORIENTED_EDGE ( 'NONE', *, *, #88429, .F. ) ;
#78556 = ORIENTED_EDGE ( 'NONE', *, *, #126777, .F. ) ;
#78557 = CARTESIAN_POINT ( 'NONE',  ( -11.69999999999999574, 12.50000000000000000, 4.330127018922196314 ) ) ;
#78558 = DIRECTION ( 'NONE',  ( 0.000000000000000000, 0.000000000000000000, 1.000000000000000000 ) ) ;
#78559 = FACE_BOUND ( 'NONE', #65201, .T. ) ;
#78560 = DIRECTION ( 'NONE',  ( 0.000000000000000000, -0.9999939076577903929, 0.003490651415223739937 ) ) ;
#78561 = CARTESIAN_POINT ( 'NONE',  ( -11.64999999999999680, 12.50000000000000000, 1.472243186433545459 ) ) ;
#78562 = DIRECTION ( 'NONE',  ( 0.000000000000000000, 0.000000000000000000, 1.000000000000000000 ) ) ;
#78563 = AXIS2_PLACEMENT_3D ( 'NONE', #48626, #127820, #70198 ) ;
#78564 = AXIS2_PLACEMENT_3D ( 'NONE', #90487, #100959, #20484 ) ;
#78565 = ADVANCED_FACE ( 'NONE', ( #114434 ), #21556, .T. ) ;
#78566 = ORIENTED_EDGE ( 'NONE', *, *, #66666, .T. ) ;
#78567 = EDGE_CURVE ( 'NONE', #51160, #52643, #105271, .T. ) ;
#78568 = DIRECTION ( 'NONE',  ( -0.000000000000000000, 1.000000000000000000, -0.000000000000000000 ) ) ;
#78569 = CARTESIAN_POINT ( 'NONE',  ( 6.449999999999930012, 2.500000000000000000, 6.941600689897073018 ) ) ;
#78570 = DIRECTION ( 'NONE',  ( 0.000000000000000000, 0.000000000000000000, 1.000000000000000000 ) ) ;
#78571 = EDGE_CURVE ( 'NONE', #65511, #127177, #36232, .T. ) ;
#78572 = DIRECTION ( 'NONE',  ( 0.000000000000000000, 1.000000000000000000, 0.000000000000000000 ) ) ;
#78573 = VERTEX_POINT ( 'NONE', #10294 ) ;
#78574 = DIRECTION ( 'NONE',  ( -4.274815082592931898E-19, -0.9999939076577903929, -0.003490651415223739937 ) ) ;
#78575 = DIRECTION ( 'NONE',  ( 0.000000000000000000, 0.000000000000000000, 1.000000000000000000 ) ) ;
#78576 = EDGE_CURVE ( 'NONE', #56898, #45181, #109113, .T. ) ;
#78577 = ORIENTED_EDGE ( 'NONE', *, *, #21838, .F. ) ;
#78578 = ORIENTED_EDGE ( 'NONE', *, *, #65950, .F. ) ;
#78579 = CARTESIAN_POINT ( 'NONE',  ( -4.150000000000024336, 2.500000000000000000, 2.165063509461097713 ) ) ;
#78580 = CARTESIAN_POINT ( 'NONE',  ( -3.950000000000026379, 12.50000000000000000, 2.446380397790835826 ) ) ;
#78581 = FACE_BOUND ( 'NONE', #76602, .T. ) ;
#78582 = CARTESIAN_POINT ( 'NONE',  ( 13.92826131978669224, -2.499999999999998668, -6.790916465128551849 ) ) ;
#78583 = EDGE_CURVE ( 'NONE', #54326, #8077, #77987, .T. ) ;
#78584 = ADVANCED_FACE ( 'NONE', ( #129454 ), #50807, .T. ) ;
#78585 = CONICAL_SURFACE ( 'NONE', #89032, 0.09999999999999982514, 0.003490658503988666988 ) ;
#78586 = ORIENTED_EDGE ( 'NONE', *, *, #76192, .T. ) ;
#78587 = CARTESIAN_POINT ( 'NONE',  ( -10.20000000000000462, 2.500000000000000000, -4.576537180435972907 ) ) ;
#78588 = VECTOR ( 'NONE', #68993, 1000.000000000000000 ) ;
#78589 = ORIENTED_EDGE ( 'NONE', *, *, #15496, .F. ) ;
#78590 = VERTEX_POINT ( 'NONE', #128139 ) ;
#78591 = FACE_OUTER_BOUND ( 'NONE', #100367, .T. ) ;
#78592 = CARTESIAN_POINT ( 'NONE',  ( 185.6666666666666856, -6.668395609140176816, -3.850000000000003642 ) ) ;
#78593 = EDGE_CURVE ( 'NONE', #108519, #88013, #111420, .T. ) ;
#78594 = ORIENTED_EDGE ( 'NONE', *, *, #128348, .F. ) ;
#78595 = FACE_OUTER_BOUND ( 'NONE', #43276, .T. ) ;
#78596 = CARTESIAN_POINT ( 'NONE',  ( 11.84999999999990372, 2.500000000000000000, 2.611473670974873151 ) ) ;
#78597 = VECTOR ( 'NONE', #62440, 1000.000000000000000 ) ;
#78598 = FACE_OUTER_BOUND ( 'NONE', #27591, .T. ) ;
#78599 = CARTESIAN_POINT ( 'NONE',  ( -10.20000000000000284, 12.50000000000000000, 3.983716857408420964 ) ) ;
#78600 = AXIS2_PLACEMENT_3D ( 'NONE', #125736, #126405, #85821 ) ;
#78601 = ORIENTED_EDGE ( 'NONE', *, *, #25003, .T. ) ;
#78602 = CIRCLE ( 'NONE', #24300, 0.06509327318403745899 ) ;
#78603 = DIRECTION ( 'NONE',  ( 0.000000000000000000, 1.000000000000000000, 0.000000000000000000 ) ) ;
#78604 = LINE ( 'NONE', #68754, #129152 ) ;
#78605 = LINE ( 'NONE', #28198, #109914 ) ;
#78606 = CIRCLE ( 'NONE', #38916, 0.1000000000000002554 ) ;
#78607 = CARTESIAN_POINT ( 'NONE',  ( 13.09999999999990195, 2.500000000000000000, -4.676537180435978769 ) ) ;
#78608 = EDGE_LOOP ( 'NONE', ( #463, #72921, #19313, #13586 ) ) ;
#78609 = DIRECTION ( 'NONE',  ( 0.000000000000000000, 0.000000000000000000, 1.000000000000000000 ) ) ;
#78610 = ORIENTED_EDGE ( 'NONE', *, *, #5521, .F. ) ;
#78611 = DIRECTION ( 'NONE',  ( -0.000000000000000000, 1.000000000000000000, -0.000000000000000000 ) ) ;
#78612 = ORIENTED_EDGE ( 'NONE', *, *, #103233, .F. ) ;
#78613 = LINE ( 'NONE', #69402, #51129 ) ;
#78614 = CARTESIAN_POINT ( 'NONE',  ( 6.649999999999929301, 2.500000000000000000, 6.495190528383297135 ) ) ;
#78615 = CARTESIAN_POINT ( 'NONE',  ( 139.9358549477330200, 2.500000000000000000, -1.098523788719517169 ) ) ;
#78616 = DIRECTION ( 'NONE',  ( 0.000000000000000000, 0.000000000000000000, 1.000000000000000000 ) ) ;
#78617 = ORIENTED_EDGE ( 'NONE', *, *, #40895, .T. ) ;
#78618 = CARTESIAN_POINT ( 'NONE',  ( 11.24999999999991118, 2.500000000000000000, -2.757883832488654097 ) ) ;
#78619 = CARTESIAN_POINT ( 'NONE',  ( -12.29999999999999716, 2.500000000000000000, 0.3464101615137776813 ) ) ;
#78620 = DIRECTION ( 'NONE',  ( -4.274815082592931898E-19, -0.9999939076577903929, -0.003490651415223739937 ) ) ;
#78621 = CARTESIAN_POINT ( 'NONE',  ( 184.6093750003413732, 9.264065473108010111E-16, -7.564683531250000925 ) ) ;
#78622 = CARTESIAN_POINT ( 'NONE',  ( 13.09999999999990195, 2.500000000000000000, 3.883716857408420431 ) ) ;
#78623 = VECTOR ( 'NONE', #13040, 1000.000000000000000 ) ;
#78624 = DIRECTION ( 'NONE',  ( -0.000000000000000000, 1.000000000000000000, -0.000000000000000000 ) ) ;
#78625 = ORIENTED_EDGE ( 'NONE', *, *, #79165, .F. ) ;
#78626 = ADVANCED_FACE ( 'NONE', ( #30597 ), #19460, .T. ) ;
#78627 = EDGE_LOOP ( 'NONE', ( #71911, #102560 ) ) ;
#78628 = DIRECTION ( 'NONE',  ( 0.000000000000000000, 0.000000000000000000, 1.000000000000000000 ) ) ;
#78629 = ORIENTED_EDGE ( 'NONE', *, *, #64636, .F. ) ;
#78630 = DIRECTION ( 'NONE',  ( -0.000000000000000000, 1.000000000000000000, -0.000000000000000000 ) ) ;
#78632 = VERTEX_POINT ( 'NONE', #59419 ) ;
#78631 = ORIENTED_EDGE ( 'NONE', *, *, #50450, .F. ) ;
#78633 = VECTOR ( 'NONE', #75211, 1000.000000000000000 ) ;
#78634 = ORIENTED_EDGE ( 'NONE', *, *, #15659, .F. ) ;
#78635 = DIRECTION ( 'NONE',  ( -4.274815082592931898E-19, -0.9999939076577903929, -0.003490651415223739937 ) ) ;
#78636 = AXIS2_PLACEMENT_3D ( 'NONE', #29622, #38161, #28348 ) ;
#78637 = AXIS2_PLACEMENT_3D ( 'NONE', #123954, #35595, #33657 ) ;
#78638 = DIRECTION ( 'NONE',  ( 0.000000000000000000, 0.000000000000000000, 1.000000000000000000 ) ) ;
#78639 = DIRECTION ( 'NONE',  ( -0.000000000000000000, -1.000000000000000000, -0.000000000000000000 ) ) ;
#78640 = CIRCLE ( 'NONE', #15905, 0.06509327318403745899 ) ;
#78641 = DIRECTION ( 'NONE',  ( 0.000000000000000000, 1.000000000000000000, 0.000000000000000000 ) ) ;
#78642 = CARTESIAN_POINT ( 'NONE',  ( 1.249999999999950262, 2.500000000000000000, 7.188010851410848723 ) ) ;
#78643 = CARTESIAN_POINT ( 'NONE',  ( 3.149999999999944400, 2.500000000000000000, 2.411473670974873862 ) ) ;
#78644 = FACE_OUTER_BOUND ( 'NONE', #20886, .T. ) ;
#78645 = CARTESIAN_POINT ( 'NONE',  ( 5.199999999999935341, 12.50000000000000000, -4.048810130592463530 ) ) ;
#78646 = ORIENTED_EDGE ( 'NONE', *, *, #10800, .T. ) ;
#78647 = AXIS2_PLACEMENT_3D ( 'NONE', #110419, #29299, #119587 ) ;
#78648 = ORIENTED_EDGE ( 'NONE', *, *, #59633, .F. ) ;
#78649 = ORIENTED_EDGE ( 'NONE', *, *, #98802, .F. ) ;
#78650 = CIRCLE ( 'NONE', #74428, 0.06509327318403745899 ) ;
#78651 = LINE ( 'NONE', #118545, #15075 ) ;
#78652 = EDGE_LOOP ( 'NONE', ( #39151, #1092, #25931, #79314 ) ) ;
#78653 = ORIENTED_EDGE ( 'NONE', *, *, #65818, .T. ) ;
#78654 = DIRECTION ( 'NONE',  ( -0.000000000000000000, 1.000000000000000000, -0.000000000000000000 ) ) ;
#78655 = DIRECTION ( 'NONE',  ( -0.000000000000000000, 1.000000000000000000, -0.000000000000000000 ) ) ;
#78656 = DIRECTION ( 'NONE',  ( -0.000000000000000000, -1.000000000000000000, -0.000000000000000000 ) ) ;
#78657 = DIRECTION ( 'NONE',  ( 0.000000000000000000, -0.000000000000000000, 1.000000000000000000 ) ) ;
#78658 = CARTESIAN_POINT ( 'NONE',  ( 11.89999999999990798, 12.50000000000000000, -3.983716857408426293 ) ) ;
#78659 = ORIENTED_EDGE ( 'NONE', *, *, #541, .T. ) ;
#78660 = DIRECTION ( 'NONE',  ( 0.000000000000000000, -0.000000000000000000, 1.000000000000000000 ) ) ;
#78661 = EDGE_LOOP ( 'NONE', ( #42064, #88892, #121495, #45648 ) ) ;
#78662 = DIRECTION ( 'NONE',  ( -4.274815082592931898E-19, -0.9999939076577903929, -0.003490651415223739937 ) ) ;
#78663 = ADVANCED_FACE ( 'NONE', ( #20756 ), #67496, .T. ) ;
#78664 = VERTEX_POINT ( 'NONE', #77723 ) ;
#78665 = FACE_OUTER_BOUND ( 'NONE', #107510, .T. ) ;
#78666 = EDGE_LOOP ( 'NONE', ( #40115, #67024, #2528, #112494 ) ) ;
#78667 = ADVANCED_FACE ( 'NONE', ( #18816 ), #86876, .T. ) ;
#78668 = ORIENTED_EDGE ( 'NONE', *, *, #74403, .T. ) ;
#78669 = EDGE_CURVE ( 'NONE', #19600, #91108, #65454, .T. ) ;
#78670 = LINE ( 'NONE', #59014, #92068 ) ;
#78671 = CARTESIAN_POINT ( 'NONE',  ( -12.49999999999999289, 2.500000000000000000, -0.6928203230275500335 ) ) ;
#78672 = CONICAL_SURFACE ( 'NONE', #105843, 0.1000000000000000472, 0.003490658503988666988 ) ;
#78673 = CARTESIAN_POINT ( 'NONE',  ( -1.900000000000034106, 2.500000000000000000, -3.883716857408426648 ) ) ;
#78674 = CARTESIAN_POINT ( 'NONE',  ( 6.849999999999929479, 2.500000000000000000, 6.841600689897072485 ) ) ;
#78675 = ADVANCED_FACE ( 'NONE', ( #104250 ), #98917, .T. ) ;
#78676 = CARTESIAN_POINT ( 'NONE',  ( 0.6499999999999566125, 2.500000000000000000, -6.941600689897077459 ) ) ;
#78678 = VERTEX_POINT ( 'NONE', #91211 ) ;
#78677 = ADVANCED_FACE ( 'NONE', ( #93152 ), #54691, .T. ) ;
#78679 = DIRECTION ( 'NONE',  ( 0.000000000000000000, 1.000000000000000000, 0.000000000000000000 ) ) ;
#78680 = CARTESIAN_POINT ( 'NONE',  ( 7.499999999999961808, 2.500000000000000000, 4.430127018922196847 ) ) ;
#78681 = ADVANCED_FACE ( 'NONE', ( #3471 ), #71531, .T. ) ;
#78682 = DIRECTION ( 'NONE',  ( 0.000000000000000000, 1.000000000000000000, 0.000000000000000000 ) ) ;
#78683 = EDGE_CURVE ( 'NONE', #95241, #4391, #67290, .T. ) ;
#78684 = EDGE_CURVE ( 'NONE', #113935, #64066, #62408, .T. ) ;
#78685 = DIRECTION ( 'NONE',  ( 0.000000000000000000, 0.000000000000000000, 1.000000000000000000 ) ) ;
#78687 = VECTOR ( 'NONE', #109798, 1000.000000000000000 ) ;
#78686 = CIRCLE ( 'NONE', #24383, 0.1000000000000002554 ) ;
#78688 = DIRECTION ( 'NONE',  ( 0.000000000000000000, -0.9999939076577903929, 0.003490651415223739937 ) ) ;
#78689 = ORIENTED_EDGE ( 'NONE', *, *, #119160, .F. ) ;
#78690 = VERTEX_POINT ( 'NONE', #82694 ) ;
#78691 = CARTESIAN_POINT ( 'NONE',  ( 11.84999999999990372, 12.50000000000000000, -6.148780366869526226 ) ) ;
#78692 = ADVANCED_FACE ( 'NONE', ( #73484 ), #29683, .T. ) ;
#78693 = EDGE_LOOP ( 'NONE', ( #36564, #34636 ) ) ;
#78695 = AXIS2_PLACEMENT_3D ( 'NONE', #82587, #11240, #121846 ) ;
#78694 = AXIS2_PLACEMENT_3D ( 'NONE', #125190, #25686, #15862 ) ;
#78696 = CARTESIAN_POINT ( 'NONE',  ( -7.050000000000016698, 12.50000000000000000, -6.560283801567339701 ) ) ;
#78697 = PLANE ( 'NONE',  #64903 ) ;
#78698 = CIRCLE ( 'NONE', #105868, 0.06509327318403745899 ) ;
#78699 = EDGE_LOOP ( 'NONE', ( #110897, #84263 ) ) ;
#78700 = CARTESIAN_POINT ( 'NONE',  ( 186.4166666666666856, 6.668395609140176816, 3.850000000000000977 ) ) ;
#78701 = CARTESIAN_POINT ( 'NONE',  ( -8.750000000000010658, 2.500000000000000000, 2.857883832488649301 ) ) ;
#78702 = DIRECTION ( 'NONE',  ( -4.274815082592931898E-19, -0.9999939076577903929, -0.003490651415223739937 ) ) ;
#78703 = DIRECTION ( 'NONE',  ( 0.000000000000000000, 0.000000000000000000, -1.000000000000000000 ) ) ;
#78704 = ORIENTED_EDGE ( 'NONE', *, *, #102482, .F. ) ;
#78705 = CARTESIAN_POINT ( 'NONE',  ( 6.249999999999965361, 2.500000000000000000, 2.265063509461097357 ) ) ;
#78706 = VERTEX_POINT ( 'NONE', #22493 ) ;
#78707 = DIRECTION ( 'NONE',  ( -0.000000000000000000, 1.000000000000000000, -0.000000000000000000 ) ) ;
#78708 = AXIS2_PLACEMENT_3D ( 'NONE', #117039, #27374, #67279 ) ;
#78709 = DIRECTION ( 'NONE',  ( -4.274815082592931898E-19, -0.9999939076577903929, -0.003490651415223739937 ) ) ;
#78710 = CARTESIAN_POINT ( 'NONE',  ( 115.5000000000000000, -2.000000000000000000, 5.000000000000003553 ) ) ;
#78711 = VERTEX_POINT ( 'NONE', #32957 ) ;
#78712 = AXIS2_PLACEMENT_3D ( 'NONE', #19949, #8809, #99797 ) ;
#78713 = CIRCLE ( 'NONE', #53569, 0.06509327318403743123 ) ;
#78714 = DIRECTION ( 'NONE',  ( -0.000000000000000000, -1.000000000000000000, -0.000000000000000000 ) ) ;
#78715 = CONICAL_SURFACE ( 'NONE', #22291, 0.1000000000000002554, 0.003490658503988666988 ) ;
#78716 = ORIENTED_EDGE ( 'NONE', *, *, #70009, .T. ) ;
#78717 = EDGE_CURVE ( 'NONE', #38652, #6400, #77774, .T. ) ;
#78718 = CARTESIAN_POINT ( 'NONE',  ( 4.149999999999938183, 12.50000000000000000, 7.188010851410848723 ) ) ;
#78719 = CARTESIAN_POINT ( 'NONE',  ( 4.999999999999936939, 2.500000000000000000, -0.5928203230275541635 ) ) ;
#78720 = VECTOR ( 'NONE', #50893, 1000.000000000000000 ) ;
#78721 = LINE ( 'NONE', #118621, #7806 ) ;
#78722 = EDGE_CURVE ( 'NONE', #6219, #115023, #23767, .T. ) ;
#78723 = AXIS2_PLACEMENT_3D ( 'NONE', #126549, #48630, #116710 ) ;
#78724 = VERTEX_POINT ( 'NONE', #44045 ) ;
#78725 = CARTESIAN_POINT ( 'NONE',  ( 2.099999999999950351, 2.500000000000000000, -5.022947341949754119 ) ) ;
#78726 = AXIS2_PLACEMENT_3D ( 'NONE', #26369, #17141, #117279 ) ;
#78727 = EDGE_CURVE ( 'NONE', #115959, #33163, #11998, .T. ) ;
#78728 = CARTESIAN_POINT ( 'NONE',  ( -10.20000000000000462, 2.500000000000000000, 0.3464101615137735735 ) ) ;
#78729 = ORIENTED_EDGE ( 'NONE', *, *, #83892, .F. ) ;
#78730 = DIRECTION ( 'NONE',  ( 0.000000000000000000, 0.000000000000000000, 1.000000000000000000 ) ) ;
#78731 = ADVANCED_FACE ( 'NONE', ( #111486 ), #4101, .T. ) ;
#78732 = ORIENTED_EDGE ( 'NONE', *, *, #8443, .F. ) ;
#78734 = AXIS2_PLACEMENT_3D ( 'NONE', #123932, #4795, #75478 ) ;
#78733 = CARTESIAN_POINT ( 'NONE',  ( -11.05000000000000249, 2.500000000000000000, -6.148780366869522673 ) ) ;
#78735 = EDGE_CURVE ( 'NONE', #58451, #7794, #66888, .T. ) ;
#78736 = EDGE_CURVE ( 'NONE', #27277, #17873, #47272, .T. ) ;
#78739 = ADVANCED_FACE ( 'NONE', ( #106191 ), #6649, .T. ) ;
#78738 = AXIS2_PLACEMENT_3D ( 'NONE', #78614, #49154, #10484 ) ;
#78737 = AXIS2_PLACEMENT_3D ( 'NONE', #97293, #64607, #36465 ) ;
#78740 = ORIENTED_EDGE ( 'NONE', *, *, #52986, .T. ) ;
#78741 = DIRECTION ( 'NONE',  ( -0.000000000000000000, -1.000000000000000000, -0.000000000000000000 ) ) ;
#78742 = CARTESIAN_POINT ( 'NONE',  ( 3.549999999999940314, 12.50000000000000000, 6.841600689897072485 ) ) ;
#78743 = ORIENTED_EDGE ( 'NONE', *, *, #77593, .T. ) ;
#78744 = ORIENTED_EDGE ( 'NONE', *, *, #23083, .T. ) ;
#78745 = DIRECTION ( 'NONE',  ( -0.000000000000000000, -1.000000000000000000, -0.000000000000000000 ) ) ;
#78746 = DIRECTION ( 'NONE',  ( 0.000000000000000000, 0.000000000000000000, 1.000000000000000000 ) ) ;
#78747 = ORIENTED_EDGE ( 'NONE', *, *, #76084, .T. ) ;
#78748 = ADVANCED_FACE ( 'NONE', ( #4733 ), #115415, .T. ) ;
#78749 = DIRECTION ( 'NONE',  ( -0.000000000000000000, 1.000000000000000000, -0.000000000000000000 ) ) ;
#78750 = CARTESIAN_POINT ( 'NONE',  ( -2.900000000000030109, 2.500000000000000000, -3.737306695894649700 ) ) ;
#78751 = DIRECTION ( 'NONE',  ( -0.000000000000000000, -1.000000000000000000, -0.000000000000000000 ) ) ;
#78752 = DIRECTION ( 'NONE',  ( -0.000000000000000000, 1.000000000000000000, -0.000000000000000000 ) ) ;
#78753 = DIRECTION ( 'NONE',  ( 0.000000000000000000, 1.000000000000000000, 0.000000000000000000 ) ) ;
#78754 = LINE ( 'NONE', #9991, #47316 ) ;
#78755 = DIRECTION ( 'NONE',  ( 0.000000000000000000, 0.000000000000000000, 1.000000000000000000 ) ) ;
#78756 = EDGE_LOOP ( 'NONE', ( #44330, #74518, #42474, #47401 ) ) ;
#78757 = ORIENTED_EDGE ( 'NONE', *, *, #91309, .F. ) ;
#78758 = VERTEX_POINT ( 'NONE', #35522 ) ;
#78759 = ORIENTED_EDGE ( 'NONE', *, *, #40136, .F. ) ;
#78760 = FACE_OUTER_BOUND ( 'NONE', #53442, .T. ) ;
#78761 = DIRECTION ( 'NONE',  ( 0.000000000000000000, 0.000000000000000000, -1.000000000000000000 ) ) ;
#78762 = FACE_OUTER_BOUND ( 'NONE', #56611, .T. ) ;
#78763 = EDGE_LOOP ( 'NONE', ( #32442, #59890, #37, #2548 ) ) ;
#78764 = FACE_BOUND ( 'NONE', #33950, .T. ) ;
#78765 = EDGE_LOOP ( 'NONE', ( #106510, #39567, #92341, #19403 ) ) ;
#78766 = EDGE_CURVE ( 'NONE', #23542, #87945, #107471, .T. ) ;
#78767 = LINE ( 'NONE', #59114, #85628 ) ;
#78768 = LINE ( 'NONE', #118662, #97940 ) ;
#78769 = CARTESIAN_POINT ( 'NONE',  ( -7.700000000000014388, 12.50000000000000000, -4.611443907251939756 ) ) ;
#78770 = CARTESIAN_POINT ( 'NONE',  ( -1.650000000000034328, 2.500000000000000000, -2.065063509461102065 ) ) ;
#78771 = AXIS2_PLACEMENT_3D ( 'NONE', #123719, #24255, #54995 ) ;
#78772 = CARTESIAN_POINT ( 'NONE',  ( -7.300000000000018474, 2.500000000000000000, -3.983716857408426293 ) ) ;
#78773 = CARTESIAN_POINT ( 'NONE',  ( 8.299999999999922551, 12.50000000000000000, 0.06509327318403504425 ) ) ;
#78774 = ORIENTED_EDGE ( 'NONE', *, *, #16891, .F. ) ;
#78775 = DIRECTION ( 'NONE',  ( 0.000000000000000000, 0.000000000000000000, 1.000000000000000000 ) ) ;
#78776 = DIRECTION ( 'NONE',  ( 0.000000000000000000, -0.000000000000000000, 1.000000000000000000 ) ) ;
#78777 = DIRECTION ( 'NONE',  ( 0.000000000000000000, 0.000000000000000000, 1.000000000000000000 ) ) ;
#78778 = AXIS2_PLACEMENT_3D ( 'NONE', #80482, #100106, #29434 ) ;
#78779 = ORIENTED_EDGE ( 'NONE', *, *, #109624, .T. ) ;
#78780 = EDGE_LOOP ( 'NONE', ( #104753, #5828, #13581, #40326 ) ) ;
#78781 = ADVANCED_FACE ( 'NONE', ( #16489 ), #81997, .T. ) ;
#78782 = ORIENTED_EDGE ( 'NONE', *, *, #34551, .T. ) ;
#78783 = ORIENTED_EDGE ( 'NONE', *, *, #29173, .T. ) ;
#78784 = CARTESIAN_POINT ( 'NONE',  ( 6.049999999999932321, 2.500000000000000000, -1.818653347947326138 ) ) ;
#78785 = DIRECTION ( 'NONE',  ( 0.000000000000000000, 0.000000000000000000, -1.000000000000000000 ) ) ;
#78787 = EDGE_LOOP ( 'NONE', ( #62735, #71526, #79447, #109710 ) ) ;
#78786 = ORIENTED_EDGE ( 'NONE', *, *, #114728, .T. ) ;
#78788 = VERTEX_POINT ( 'NONE', #127126 ) ;
#78789 = CARTESIAN_POINT ( 'NONE',  ( 185.1250000000000000, -8.891194145520236347, -1.633285867636356299E-15 ) ) ;
#78791 = CIRCLE ( 'NONE', #66237, 0.1000000000000000472 ) ;
#78790 = CONICAL_SURFACE ( 'NONE', #3461, 0.09999999999999982514, 0.003490658503988666988 ) ;
#78792 = CIRCLE ( 'NONE', #39084, 0.1000000000000002554 ) ;
#78793 = DIRECTION ( 'NONE',  ( 0.000000000000000000, -0.9999939076577903929, 0.003490651415223739937 ) ) ;
#78794 = PLANE ( 'NONE',  #85305 ) ;
#78795 = DIRECTION ( 'NONE',  ( 0.000000000000000000, 1.000000000000000000, 0.000000000000000000 ) ) ;
#78796 = CARTESIAN_POINT ( 'NONE',  ( -10.45000000000000462, 12.50000000000000000, -6.495190528383298911 ) ) ;
#78797 = CARTESIAN_POINT ( 'NONE',  ( 2.500000000000002220, 1.499999999999999334, 10.00000000000000178 ) ) ;
#78798 = CARTESIAN_POINT ( 'NONE',  ( -5.200000000000020606, 12.50000000000000000, -0.3464101615137782364 ) ) ;
#78799 = EDGE_CURVE ( 'NONE', #112624, #76508, #94509, .T. ) ;
#78800 = ORIENTED_EDGE ( 'NONE', *, *, #77017, .T. ) ;
#78801 = DIRECTION ( 'NONE',  ( 0.000000000000000000, -0.000000000000000000, 1.000000000000000000 ) ) ;
#78802 = ORIENTED_EDGE ( 'NONE', *, *, #44592, .T. ) ;
#78803 = ORIENTED_EDGE ( 'NONE', *, *, #79469, .F. ) ;
#78804 = ORIENTED_EDGE ( 'NONE', *, *, #97617, .F. ) ;
#78805 = DIRECTION ( 'NONE',  ( 0.000000000000000000, -0.000000000000000000, 1.000000000000000000 ) ) ;
#78806 = ORIENTED_EDGE ( 'NONE', *, *, #78158, .F. ) ;
#78807 = AXIS2_PLACEMENT_3D ( 'NONE', #17401, #87440, #47538 ) ;
#78808 = ORIENTED_EDGE ( 'NONE', *, *, #89273, .T. ) ;
#78809 = CIRCLE ( 'NONE', #35178, 0.06509327318403745899 ) ;
#78810 = CARTESIAN_POINT ( 'NONE',  ( -12.94999999999999218, 2.500000000000000000, -2.165063509461099489 ) ) ;
#78811 = DIRECTION ( 'NONE',  ( 0.000000000000000000, 0.000000000000000000, -1.000000000000000000 ) ) ;
#78813 = AXIS2_PLACEMENT_3D ( 'NONE', #28326, #39457, #38820 ) ;
#78812 = DIRECTION ( 'NONE',  ( 0.000000000000000000, -0.000000000000000000, 1.000000000000000000 ) ) ;
#78814 = DIRECTION ( 'NONE',  ( 0.000000000000000000, 0.000000000000000000, 1.000000000000000000 ) ) ;
#78815 = CARTESIAN_POINT ( 'NONE',  ( -9.999999999999969802, 2.500000000000000000, 4.330127018922196314 ) ) ;
#78816 = CIRCLE ( 'NONE', #122715, 0.09999999999999999167 ) ;
#78817 = ORIENTED_EDGE ( 'NONE', *, *, #47795, .T. ) ;
#78819 = CIRCLE ( 'NONE', #59957, 0.06509327318403745899 ) ;
#78818 = CARTESIAN_POINT ( 'NONE',  ( -13.74999999999998934, 2.500000000000000000, -1.472243186433547901 ) ) ;
#78820 = EDGE_LOOP ( 'NONE', ( #45246, #80142, #7944, #83049 ) ) ;
#78821 = CONICAL_SURFACE ( 'NONE', #45366, 0.09999999999999982514, 0.003490658503988666988 ) ;
#78822 = CARTESIAN_POINT ( 'NONE',  ( 6.449999999999931788, 12.50000000000000000, -6.148780366869526226 ) ) ;
#78823 = ADVANCED_FACE ( 'NONE', ( #96344 ), #88226, .T. ) ;
#78824 = ORIENTED_EDGE ( 'NONE', *, *, #39277, .F. ) ;
#78825 = FACE_OUTER_BOUND ( 'NONE', #110695, .T. ) ;
#78826 = DIRECTION ( 'NONE',  ( -0.000000000000000000, -1.000000000000000000, -0.000000000000000000 ) ) ;
#78827 = ORIENTED_EDGE ( 'NONE', *, *, #3658, .T. ) ;
#78828 = CARTESIAN_POINT ( 'NONE',  ( -8.950000000000009948, 2.500000000000000000, 2.611473670974873151 ) ) ;
#78829 = CIRCLE ( 'NONE', #116447, 0.1000000000000000472 ) ;
#78830 = CARTESIAN_POINT ( 'NONE',  ( 2.099999999999950351, 12.50000000000000000, -2.276824562219559311E-15 ) ) ;
#78831 = ORIENTED_EDGE ( 'NONE', *, *, #52322, .T. ) ;
#78832 = CONICAL_SURFACE ( 'NONE', #22388, 0.1000000000000000056, 0.003490658503988666988 ) ;
#78833 = AXIS2_PLACEMENT_3D ( 'NONE', #29848, #110337, #97935 ) ;
#78834 = CARTESIAN_POINT ( 'NONE',  ( -12.69999999999999218, 2.500000000000000000, -4.676537180435975216 ) ) ;
#78835 = ORIENTED_EDGE ( 'NONE', *, *, #4615, .T. ) ;
#78836 = ADVANCED_FACE ( 'NONE', ( #15853 ), #97004, .T. ) ;
#78838 = ORIENTED_EDGE ( 'NONE', *, *, #100222, .F. ) ;
#78837 = EDGE_CURVE ( 'NONE', #6221, #87480, #38090, .T. ) ;
#78839 = CARTESIAN_POINT ( 'NONE',  ( -1.250000000000037970, 2.500000000000000000, 7.288010851410849256 ) ) ;
#78840 = CARTESIAN_POINT ( 'NONE',  ( 3.549999999999944755, 12.50000000000000000, -6.906693963081115051 ) ) ;
#78841 = ADVANCED_FACE ( 'NONE', ( #64955 ), #40154, .T. ) ;
#78842 = CARTESIAN_POINT ( 'NONE',  ( 184.7968750003414016, 8.734944146203032389, 5.348610694689227483E-16 ) ) ;
#78843 = EDGE_CURVE ( 'NONE', #102605, #118212, #76082, .T. ) ;
#78844 = DIRECTION ( 'NONE',  ( 0.000000000000000000, 0.000000000000000000, -1.000000000000000000 ) ) ;
#78845 = FACE_OUTER_BOUND ( 'NONE', #80072, .T. ) ;
#78846 = ORIENTED_EDGE ( 'NONE', *, *, #118386, .T. ) ;
#78847 = CARTESIAN_POINT ( 'NONE',  ( 184.0312500006828031, 9.429780353434619030E-16, -7.700000000000000178 ) ) ;
#78849 = ADVANCED_FACE ( 'NONE', ( #26987 ), #25680, .T. ) ;
#78848 = AXIS2_PLACEMENT_3D ( 'NONE', #129500, #39821, #79724 ) ;
#78850 = ORIENTED_EDGE ( 'NONE', *, *, #8933, .F. ) ;
#78851 = EDGE_CURVE ( 'NONE', #108664, #86700, #33877, .T. ) ;
#78852 = PLANE ( 'NONE',  #48650 ) ;
#78853 = LINE ( 'NONE', #129250, #93978 ) ;
#78854 = EDGE_CURVE ( 'NONE', #33691, #86214, #25046, .T. ) ;
#78855 = EDGE_LOOP ( 'NONE', ( #101405, #5731, #86222, #41323 ) ) ;
#78856 = CARTESIAN_POINT ( 'NONE',  ( -3.150000000000032330, 12.50000000000000000, -6.148780366869526226 ) ) ;
#78857 = CARTESIAN_POINT ( 'NONE',  ( -5.000000000000023093, 2.500000000000000000, 0.7928203230275495672 ) ) ;
#78858 = DIRECTION ( 'NONE',  ( 0.000000000000000000, 1.000000000000000000, 0.000000000000000000 ) ) ;
#78859 = FACE_OUTER_BOUND ( 'NONE', #68916, .T. ) ;
#78860 = FACE_OUTER_BOUND ( 'NONE', #86387, .T. ) ;
#78861 = ORIENTED_EDGE ( 'NONE', *, *, #17651, .T. ) ;
#78862 = CARTESIAN_POINT ( 'NONE',  ( -5.200000000000022382, 2.500000000000000000, 0.4464101615137735513 ) ) ;
#78863 = CIRCLE ( 'NONE', #93419, 0.06509327318403745899 ) ;
#78864 = DIRECTION ( 'NONE',  ( 0.000000000000000000, 0.000000000000000000, -1.000000000000000000 ) ) ;
#78865 = CARTESIAN_POINT ( 'NONE',  ( 0.3999999999999555023, 2.500000000000000000, 4.430127018922196847 ) ) ;
#78866 = ORIENTED_EDGE ( 'NONE', *, *, #30447, .F. ) ;
#78868 = CIRCLE ( 'NONE', #87153, 0.09999999999999999167 ) ;
#78867 = VECTOR ( 'NONE', #43284, 1000.000000000000000 ) ;
#78869 = CARTESIAN_POINT ( 'NONE',  ( -10.40000000000000213, 12.50000000000000000, 4.330127018922196314 ) ) ;
#78870 = ORIENTED_EDGE ( 'NONE', *, *, #96543, .T. ) ;
#78871 = VERTEX_POINT ( 'NONE', #85253 ) ;
#78872 = FACE_OUTER_BOUND ( 'NONE', #126711, .T. ) ;
#78873 = ORIENTED_EDGE ( 'NONE', *, *, #123006, .F. ) ;
#78874 = CARTESIAN_POINT ( 'NONE',  ( 8.949999999999915801, 12.50000000000000000, 6.841600689897072485 ) ) ;
#78875 = DIRECTION ( 'NONE',  ( 0.000000000000000000, 0.000000000000000000, 1.000000000000000000 ) ) ;
#78877 = CIRCLE ( 'NONE', #60098, 0.06509327318403745899 ) ;
#78876 = VECTOR ( 'NONE', #19406, 1000.000000000000000 ) ;
#78878 = ORIENTED_EDGE ( 'NONE', *, *, #110786, .F. ) ;
#78879 = VECTOR ( 'NONE', #89839, 1000.000000000000000 ) ;
#78880 = DIRECTION ( 'NONE',  ( -0.000000000000000000, -1.000000000000000000, -0.000000000000000000 ) ) ;
#78882 = ORIENTED_EDGE ( 'NONE', *, *, #84789, .T. ) ;
#78881 = DIRECTION ( 'NONE',  ( -0.000000000000000000, 1.000000000000000000, -0.000000000000000000 ) ) ;
#78883 = DIRECTION ( 'NONE',  ( 0.000000000000000000, 0.000000000000000000, 1.000000000000000000 ) ) ;
#78884 = FACE_OUTER_BOUND ( 'NONE', #106940, .T. ) ;
#78885 = ORIENTED_EDGE ( 'NONE', *, *, #24270, .T. ) ;
#78886 = EDGE_CURVE ( 'NONE', #87133, #109940, #113290, .T. ) ;
#78887 = VECTOR ( 'NONE', #90655, 1000.000000000000000 ) ;
#78888 = ORIENTED_EDGE ( 'NONE', *, *, #64956, .T. ) ;
#78889 = EDGE_CURVE ( 'NONE', #72558, #23223, #125802, .T. ) ;
#78890 = ORIENTED_EDGE ( 'NONE', *, *, #25621, .T. ) ;
#78891 = DIRECTION ( 'NONE',  ( 0.000000000000000000, 1.000000000000000000, 0.000000000000000000 ) ) ;
#78892 = DIRECTION ( 'NONE',  ( -0.000000000000000000, 1.000000000000000000, -0.000000000000000000 ) ) ;
#78893 = FACE_OUTER_BOUND ( 'NONE', #101234, .T. ) ;
#78894 = FACE_BOUND ( 'NONE', #48822, .T. ) ;
#78895 = ORIENTED_EDGE ( 'NONE', *, *, #16403, .F. ) ;
#78896 = DIRECTION ( 'NONE',  ( -0.000000000000000000, 1.000000000000000000, -0.000000000000000000 ) ) ;
#78897 = LINE ( 'NONE', #88698, #121305 ) ;
#78898 = VECTOR ( 'NONE', #59405, 1000.000000000000000 ) ;
#78899 = ORIENTED_EDGE ( 'NONE', *, *, #34460, .F. ) ;
#78900 = EDGE_CURVE ( 'NONE', #33453, #117544, #19191, .T. ) ;
#78901 = CARTESIAN_POINT ( 'NONE',  ( -3.150000000000030109, 2.500000000000000000, -2.411473670974877859 ) ) ;
#78902 = CARTESIAN_POINT ( 'NONE',  ( 16.80832070733759664, 1.716026667499273239, 5.822501722867528429 ) ) ;
#78903 = VECTOR ( 'NONE', #113608, 1000.000000000000000 ) ;
#78904 = DIRECTION ( 'NONE',  ( 0.000000000000000000, 0.000000000000000000, 1.000000000000000000 ) ) ;
#78905 = CARTESIAN_POINT ( 'NONE',  ( -7.300000000000016698, 2.500000000000000000, -0.3464101615137783474 ) ) ;
#78906 = DIRECTION ( 'NONE',  ( 0.000000000000000000, 0.000000000000000000, 1.000000000000000000 ) ) ;
#78907 = DIRECTION ( 'NONE',  ( 0.000000000000000000, 1.000000000000000000, 0.000000000000000000 ) ) ;
#78908 = CARTESIAN_POINT ( 'NONE',  ( -12.49999999999999289, 12.50000000000000000, -4.957854068765714217 ) ) ;
#78909 = CIRCLE ( 'NONE', #49668, 5.000000000000000000 ) ;
#78910 = AXIS2_PLACEMENT_3D ( 'NONE', #25535, #53092, #13788 ) ;
#78911 = VERTEX_POINT ( 'NONE', #85 ) ;
#78912 = ORIENTED_EDGE ( 'NONE', *, *, #87349, .T. ) ;
#78913 = ORIENTED_EDGE ( 'NONE', *, *, #30069, .T. ) ;
#78914 = ORIENTED_EDGE ( 'NONE', *, *, #25859, .F. ) ;
#78915 = VERTEX_POINT ( 'NONE', #118568 ) ;
#78916 = CARTESIAN_POINT ( 'NONE',  ( -4.150000000000024336, 2.500000000000000000, -2.957883832488653830 ) ) ;
#78917 = CARTESIAN_POINT ( 'NONE',  ( -1.650000000000034772, 2.500000000000000000, 6.495190528383297135 ) ) ;
#78918 = AXIS2_PLACEMENT_3D ( 'NONE', #9715, #109853, #99391 ) ;
#78919 = VERTEX_POINT ( 'NONE', #28269 ) ;
#78920 = FACE_BOUND ( 'NONE', #82900, .T. ) ;
#78921 = DIRECTION ( 'NONE',  ( 0.000000000000000000, 0.000000000000000000, -1.000000000000000000 ) ) ;
#78923 = CIRCLE ( 'NONE', #20323, 0.06509327318403745899 ) ;
#78922 = CIRCLE ( 'NONE', #53761, 0.06509327318403745899 ) ;
#78924 = LINE ( 'NONE', #48158, #21948 ) ;
#78925 = CARTESIAN_POINT ( 'NONE',  ( 6.249999999999967137, 12.50000000000000000, 6.495190528383297135 ) ) ;
#78926 = DIRECTION ( 'NONE',  ( 0.000000000000000000, -0.000000000000000000, 1.000000000000000000 ) ) ;
#78927 = CARTESIAN_POINT ( 'NONE',  ( 5.849999999999933920, 2.500000000000000000, 6.495190528383297135 ) ) ;
#78928 = ORIENTED_EDGE ( 'NONE', *, *, #64069, .T. ) ;
#78929 = ORIENTED_EDGE ( 'NONE', *, *, #71108, .F. ) ;
#78930 = EDGE_CURVE ( 'NONE', #26610, #128555, #117463, .T. ) ;
#78931 = VERTEX_POINT ( 'NONE', #7969 ) ;
#78932 = ORIENTED_EDGE ( 'NONE', *, *, #120786, .F. ) ;
#78933 = CARTESIAN_POINT ( 'NONE',  ( -8.950000000000011724, 2.500000000000000000, -6.148780366869520897 ) ) ;
#78934 = LINE ( 'NONE', #57343, #52617 ) ;
#78935 = CARTESIAN_POINT ( 'NONE',  ( 2.299999999999948752, 12.50000000000000000, 0.2813168883297361700 ) ) ;
#78936 = ORIENTED_EDGE ( 'NONE', *, *, #66114, .T. ) ;
#78937 = LINE ( 'NONE', #29195, #7877 ) ;
#78938 = DIRECTION ( 'NONE',  ( -1.000000000000000000, -0.000000000000000000, -0.000000000000000000 ) ) ;
#78939 = CARTESIAN_POINT ( 'NONE',  ( -1.250000000000037526, 12.50000000000000000, -5.802370205355749988 ) ) ;
#78941 = CARTESIAN_POINT ( 'NONE',  ( 184.9010416670080588, -4.367472073101519747, 7.564683531249999149 ) ) ;
#78940 = ADVANCED_BREP_SHAPE_REPRESENTATION ( '', ( #57499, #108296 ), #20574 ) ;
#78942 = DIRECTION ( 'NONE',  ( -0.000000000000000000, 1.000000000000000000, -0.000000000000000000 ) ) ;
#78943 = CARTESIAN_POINT ( 'NONE',  ( 6.049999999999932321, 2.500000000000000000, 1.818653347947321475 ) ) ;
#78944 = EDGE_CURVE ( 'NONE', #29090, #81317, #410, .T. ) ;
#78945 = DIRECTION ( 'NONE',  ( 0.000000000000000000, 0.000000000000000000, -1.000000000000000000 ) ) ;
#78946 = EDGE_CURVE ( 'NONE', #107061, #35451, #61071, .T. ) ;
#78947 = EDGE_LOOP ( 'NONE', ( #25118, #46923 ) ) ;
#78948 = CARTESIAN_POINT ( 'NONE',  ( 4.349999999999941025, 12.50000000000000000, -6.148780366869526226 ) ) ;
#78949 = AXIS2_PLACEMENT_3D ( 'NONE', #32602, #102588, #43067 ) ;
#78950 = ORIENTED_EDGE ( 'NONE', *, *, #85320, .T. ) ;
#78951 = VECTOR ( 'NONE', #53253, 1000.000000000000000 ) ;
#78952 = EDGE_LOOP ( 'NONE', ( #86203, #124435, #122174, #79934 ) ) ;
#78953 = CARTESIAN_POINT ( 'NONE',  ( 9.599999999999917932, 2.500000000000000000, 0.7928203230275495672 ) ) ;
#78954 = DIRECTION ( 'NONE',  ( 0.000000000000000000, 0.000000000000000000, 1.000000000000000000 ) ) ;
#78956 = ADVANCED_FACE ( 'NONE', ( #9913 ), #59015, .T. ) ;
#78955 = CARTESIAN_POINT ( 'NONE',  ( -6.050000000000018474, 2.500000000000000000, 6.741600689897071952 ) ) ;
#78957 = ORIENTED_EDGE ( 'NONE', *, *, #36344, .F. ) ;
#78959 = ORIENTED_EDGE ( 'NONE', *, *, #73057, .T. ) ;
#78958 = VECTOR ( 'NONE', #126831, 1000.000000000000000 ) ;
#78960 = CARTESIAN_POINT ( 'NONE',  ( 9.349999999999916156, 2.500000000000000000, -1.818653347947326138 ) ) ;
#78961 = AXIS2_PLACEMENT_3D ( 'NONE', #81990, #21807, #102916 ) ;
#78962 = AXIS2_PLACEMENT_3D ( 'NONE', #80055, #20497, #60437 ) ;
#78963 = CARTESIAN_POINT ( 'NONE',  ( -9.400000000000007461, 2.500000000000000000, -0.3464101615137783474 ) ) ;
#78964 = DIRECTION ( 'NONE',  ( 0.000000000000000000, 0.000000000000000000, -1.000000000000000000 ) ) ;
#78965 = ORIENTED_EDGE ( 'NONE', *, *, #18905, .F. ) ;
#78966 = FACE_OUTER_BOUND ( 'NONE', #6873, .T. ) ;
#78967 = ORIENTED_EDGE ( 'NONE', *, *, #45030, .F. ) ;
#78968 = LINE ( 'NONE', #97942, #108444 ) ;
#78969 = AXIS2_PLACEMENT_3D ( 'NONE', #88379, #128351, #56989 ) ;
#78970 = ORIENTED_EDGE ( 'NONE', *, *, #75758, .F. ) ;
#78971 = DIRECTION ( 'NONE',  ( 0.000000000000000000, 1.000000000000000000, 0.000000000000000000 ) ) ;
#78972 = EDGE_CURVE ( 'NONE', #56832, #124839, #15005, .T. ) ;
#78973 = CARTESIAN_POINT ( 'NONE',  ( 5.849999999999933031, 2.500000000000000000, 7.088010851410848190 ) ) ;
#78974 = CARTESIAN_POINT ( 'NONE',  ( 179.5000000000000000, 0.6250000000000000000, 7.634788798650556707 ) ) ;
#78975 = CONICAL_SURFACE ( 'NONE', #87343, 0.1000000000000002554, 0.003490658503988666988 ) ;
#78976 = FACE_OUTER_BOUND ( 'NONE', #102636, .T. ) ;
#78977 = VERTEX_POINT ( 'NONE', #119222 ) ;
#78978 = EDGE_CURVE ( 'NONE', #90845, #57522, #98941, .T. ) ;
#78980 = AXIS2_PLACEMENT_3D ( 'NONE', #105922, #102835, #73381 ) ;
#78979 = DIRECTION ( 'NONE',  ( 0.000000000000000000, 0.000000000000000000, 1.000000000000000000 ) ) ;
#78981 = VECTOR ( 'NONE', #116112, 1000.000000000000000 ) ;
#78982 = VERTEX_POINT ( 'NONE', #19748 ) ;
#78983 = ORIENTED_EDGE ( 'NONE', *, *, #2932, .T. ) ;
#78984 = EDGE_CURVE ( 'NONE', #15244, #32827, #97647, .T. ) ;
#78985 = ADVANCED_FACE ( 'NONE', ( #129070 ), #73575, .T. ) ;
#78986 = DIRECTION ( 'NONE',  ( -4.274815082592931898E-19, -0.9999939076577903929, -0.003490651415223739937 ) ) ;
#78987 = CARTESIAN_POINT ( 'NONE',  ( -4.800000000000024691, 12.50000000000000000, 4.676537180435972552 ) ) ;
#78988 = CARTESIAN_POINT ( 'NONE',  ( -7.700000000000014388, 2.500000000000000000, -0.4464101615137782142 ) ) ;
#78989 = EDGE_CURVE ( 'NONE', #78289, #101891, #35936, .T. ) ;
#78990 = DIRECTION ( 'NONE',  ( 0.000000000000000000, -0.9999939076577903929, 0.003490651415223739937 ) ) ;
#78991 = EDGE_CURVE ( 'NONE', #108881, #52645, #69376, .T. ) ;
#78992 = DIRECTION ( 'NONE',  ( 0.000000000000000000, -0.9999939076577903929, 0.003490651415223739937 ) ) ;
#78993 = DIRECTION ( 'NONE',  ( 0.000000000000000000, 0.000000000000000000, 1.000000000000000000 ) ) ;
#78994 = CIRCLE ( 'NONE', #91589, 0.1000000000000002554 ) ;
#78995 = DIRECTION ( 'NONE',  ( 0.000000000000000000, 0.000000000000000000, 1.000000000000000000 ) ) ;
#78996 = PLANE ( 'NONE',  #126527 ) ;
#78997 = DIRECTION ( 'NONE',  ( -0.000000000000000000, -1.000000000000000000, -0.000000000000000000 ) ) ;
#78998 = EDGE_CURVE ( 'NONE', #120218, #49230, #80596, .T. ) ;
#78999 = ADVANCED_FACE ( 'NONE', ( #9272 ), #4700, .T. ) ;
#79000 = AXIS2_PLACEMENT_3D ( 'NONE', #48653, #171, #128529 ) ;
#79001 = CIRCLE ( 'NONE', #43407, 0.1000000000000002554 ) ;
#79002 = EDGE_CURVE ( 'NONE', #94563, #102844, #49218, .T. ) ;
#79003 = CIRCLE ( 'NONE', #39309, 0.06509327318403745899 ) ;
#79004 = EDGE_CURVE ( 'NONE', #3617, #25385, #102923, .T. ) ;
#79005 = VERTEX_POINT ( 'NONE', #57738 ) ;
#79006 = LINE ( 'NONE', #56734, #119455 ) ;
#79007 = EDGE_CURVE ( 'NONE', #97758, #31178, #88324, .T. ) ;
#79008 = FACE_OUTER_BOUND ( 'NONE', #81786, .T. ) ;
#79009 = CARTESIAN_POINT ( 'NONE',  ( -13.09999999999999254, 12.50000000000000000, -4.741630453620012453 ) ) ;
#79010 = PLANE ( 'NONE',  #94492 ) ;
#79011 = FACE_OUTER_BOUND ( 'NONE', #123480, .T. ) ;
#79012 = EDGE_CURVE ( 'NONE', #71169, #107580, #89215, .T. ) ;
#79013 = ORIENTED_EDGE ( 'NONE', *, *, #50606, .F. ) ;
#79014 = DIRECTION ( 'NONE',  ( 0.000000000000000000, 0.000000000000000000, 1.000000000000000000 ) ) ;
#79015 = CIRCLE ( 'NONE', #14130, 0.09999999999999982514 ) ;
#79016 = DIRECTION ( 'NONE',  ( 0.000000000000000000, 1.000000000000000000, 0.000000000000000000 ) ) ;
#79018 = ORIENTED_EDGE ( 'NONE', *, *, #21257, .T. ) ;
#79017 = CARTESIAN_POINT ( 'NONE',  ( -1.650000000000034328, 12.50000000000000000, -6.560283801567339701 ) ) ;
#79019 = ORIENTED_EDGE ( 'NONE', *, *, #101906, .F. ) ;
#79020 = DIRECTION ( 'NONE',  ( -4.274815082592931898E-19, -0.9999939076577903929, -0.003490651415223739937 ) ) ;
#79021 = EDGE_LOOP ( 'NONE', ( #54338, #43470, #116505, #109456 ) ) ;
#79022 = VERTEX_POINT ( 'NONE', #79408 ) ;
#79023 = VERTEX_POINT ( 'NONE', #119307 ) ;
#79024 = CARTESIAN_POINT ( 'NONE',  ( 6.049999999999930544, 12.50000000000000000, 2.511473670974873507 ) ) ;
#79025 = FACE_OUTER_BOUND ( 'NONE', #42606, .T. ) ;
#79026 = DIRECTION ( 'NONE',  ( 0.000000000000000000, 1.000000000000000000, 0.000000000000000000 ) ) ;
#79027 = DIRECTION ( 'NONE',  ( -0.000000000000000000, 1.000000000000000000, -0.000000000000000000 ) ) ;
#79028 = ORIENTED_EDGE ( 'NONE', *, *, #123284, .T. ) ;
#79029 = DIRECTION ( 'NONE',  ( 0.000000000000000000, 0.000000000000000000, -1.000000000000000000 ) ) ;
#79030 = ORIENTED_EDGE ( 'NONE', *, *, #66943, .T. ) ;
#79031 = DIRECTION ( 'NONE',  ( 0.000000000000000000, 0.000000000000000000, 1.000000000000000000 ) ) ;
#79032 = CONICAL_SURFACE ( 'NONE', #56017, 0.1000000000000002554, 0.003490658503988666988 ) ;
#79033 = DIRECTION ( 'NONE',  ( -0.000000000000000000, -1.000000000000000000, -0.000000000000000000 ) ) ;
#79034 = LINE ( 'NONE', #89483, #104957 ) ;
#79035 = DIRECTION ( 'NONE',  ( 0.000000000000000000, 1.000000000000000000, 0.000000000000000000 ) ) ;
#79036 = ORIENTED_EDGE ( 'NONE', *, *, #120038, .F. ) ;
#79037 = AXIS2_PLACEMENT_3D ( 'NONE', #122577, #1498, #2793 ) ;
#79038 = EDGE_CURVE ( 'NONE', #85834, #98777, #100857, .T. ) ;
#79039 = AXIS2_PLACEMENT_3D ( 'NONE', #48586, #88493, #78703 ) ;
#79040 = EDGE_LOOP ( 'NONE', ( #97698, #17723, #81548, #38081 ) ) ;
#79041 = VERTEX_POINT ( 'NONE', #21112 ) ;
#79043 = ADVANCED_FACE ( 'NONE', ( #128528 ), #90488, .T. ) ;
#79042 = ORIENTED_EDGE ( 'NONE', *, *, #92224, .T. ) ;
#79044 = VERTEX_POINT ( 'NONE', #71502 ) ;
#79045 = CARTESIAN_POINT ( 'NONE',  ( -5.400000000000020783, 2.500000000000000000, 5.022947341949748790 ) ) ;
#79046 = DIRECTION ( 'NONE',  ( 0.000000000000000000, 1.000000000000000000, 0.000000000000000000 ) ) ;
#79047 = FACE_OUTER_BOUND ( 'NONE', #4610, .T. ) ;
#79048 = FACE_BOUND ( 'NONE', #56376, .T. ) ;
#79049 = CARTESIAN_POINT ( 'NONE',  ( -9.150000000000009237, 12.50000000000000000, 2.230156782645134950 ) ) ;
#79050 = CARTESIAN_POINT ( 'NONE',  ( 186.7812500006828031, 0.000000000000000000, 7.700000000000000178 ) ) ;
#79051 = AXIS2_PLACEMENT_3D ( 'NONE', #128789, #37594, #106949 ) ;
#79052 = LINE ( 'NONE', #109114, #68580 ) ;
#79053 = CARTESIAN_POINT ( 'NONE',  ( -7.900000000000014566, 2.500000000000000000, 0.6928203230275494784 ) ) ;
#79054 = AXIS2_PLACEMENT_3D ( 'NONE', #77247, #27476, #67386 ) ;
#79055 = DIRECTION ( 'NONE',  ( -0.000000000000000000, 1.000000000000000000, -0.000000000000000000 ) ) ;
#79056 = CARTESIAN_POINT ( 'NONE',  ( -3.550000000000027800, 12.50000000000000000, 6.148780366869520009 ) ) ;
#79057 = CARTESIAN_POINT ( 'NONE',  ( 1.249999999999953815, 2.500000000000000000, -2.757883832488654097 ) ) ;
#79058 = CIRCLE ( 'NONE', #24764, 3.000000000000000000 ) ;
#79059 = DIRECTION ( 'NONE',  ( 0.000000000000000000, 1.000000000000000000, 0.000000000000000000 ) ) ;
#79060 = VERTEX_POINT ( 'NONE', #19160 ) ;
#79061 = ORIENTED_EDGE ( 'NONE', *, *, #125424, .F. ) ;
#79062 = ORIENTED_EDGE ( 'NONE', *, *, #4777, .F. ) ;
#79063 = ORIENTED_EDGE ( 'NONE', *, *, #86632, .F. ) ;
#79064 = AXIS2_PLACEMENT_3D ( 'NONE', #55162, #15199, #6038 ) ;
#79065 = DIRECTION ( 'NONE',  ( 0.000000000000000000, -0.9999939076577903929, 0.003490651415223739937 ) ) ;
#79066 = CARTESIAN_POINT ( 'NONE',  ( 3.099999999999945022, 12.50000000000000000, -0.4115034346978157509 ) ) ;
#79067 = FACE_BOUND ( 'NONE', #68283, .T. ) ;
#79068 = FACE_OUTER_BOUND ( 'NONE', #93478, .T. ) ;
#79069 = AXIS2_PLACEMENT_3D ( 'NONE', #54813, #83017, #14867 ) ;
#79070 =( GEOMETRIC_REPRESENTATION_CONTEXT ( 3 ) GLOBAL_UNCERTAINTY_ASSIGNED_CONTEXT ( ( #25699 ) ) GLOBAL_UNIT_ASSIGNED_CONTEXT ( ( #30989, #40807, #63655 ) ) REPRESENTATION_CONTEXT ( 'NONE', 'WORKASPACE' ) );
#79071 = ORIENTED_EDGE ( 'NONE', *, *, #79151, .F. ) ;
#79072 = DIRECTION ( 'NONE',  ( -0.000000000000000000, 1.000000000000000000, -0.000000000000000000 ) ) ;
#79073 = LINE ( 'NONE', #20788, #78720 ) ;
#79074 = CARTESIAN_POINT ( 'NONE',  ( -9.150000000000009237, 12.50000000000000000, -2.922977105672691422 ) ) ;
#79075 = DIRECTION ( 'NONE',  ( 0.000000000000000000, 0.000000000000000000, -1.000000000000000000 ) ) ;
#79076 = LINE ( 'NONE', #10321, #80864 ) ;
#79077 = CIRCLE ( 'NONE', #89523, 0.09999999999999982514 ) ;
#79078 = ORIENTED_EDGE ( 'NONE', *, *, #18810, .T. ) ;
#79079 = AXIS2_PLACEMENT_3D ( 'NONE', #32114, #93592, #103417 ) ;
#79080 = FACE_OUTER_BOUND ( 'NONE', #62922, .T. ) ;
#79081 = EDGE_CURVE ( 'NONE', #45854, #71342, #27700, .T. ) ;
#79082 = VERTEX_POINT ( 'NONE', #31591 ) ;
#79083 = VERTEX_POINT ( 'NONE', #69567 ) ;
#79084 = DIRECTION ( 'NONE',  ( 0.000000000000000000, 0.000000000000000000, 1.000000000000000000 ) ) ;
#79085 = FACE_OUTER_BOUND ( 'NONE', #107148, .T. ) ;
#79086 = ORIENTED_EDGE ( 'NONE', *, *, #57580, .F. ) ;
#79087 = DIRECTION ( 'NONE',  ( -0.000000000000000000, -1.000000000000000000, -0.000000000000000000 ) ) ;
#79088 = CARTESIAN_POINT ( 'NONE',  ( -13.74999999999998757, 2.500000000000000000, 1.472243186433549456 ) ) ;
#79089 = ORIENTED_EDGE ( 'NONE', *, *, #117956, .T. ) ;
#79090 = CARTESIAN_POINT ( 'NONE',  ( -2.100000000000034284, 12.50000000000000000, -0.06509327318403980434 ) ) ;
#79091 = VERTEX_POINT ( 'NONE', #91153 ) ;
#79092 = EDGE_CURVE ( 'NONE', #51861, #47076, #111309, .T. ) ;
#79093 = AXIS2_PLACEMENT_3D ( 'NONE', #88872, #7714, #28023 ) ;
#79094 = ADVANCED_FACE ( 'NONE', ( #59121 ), #54893, .T. ) ;
#79095 = DIRECTION ( 'NONE',  ( 0.000000000000000000, 0.000000000000000000, -1.000000000000000000 ) ) ;
#79096 = ORIENTED_EDGE ( 'NONE', *, *, #40136, .T. ) ;
#79097 = DIRECTION ( 'NONE',  ( 0.000000000000000000, 0.000000000000000000, 1.000000000000000000 ) ) ;
#79098 = FACE_BOUND ( 'NONE', #62772, .T. ) ;
#79100 = AXIS2_PLACEMENT_3D ( 'NONE', #34766, #113953, #104134 ) ;
#79099 = AXIS2_PLACEMENT_3D ( 'NONE', #37438, #17096, #57718 ) ;
#79101 = ORIENTED_EDGE ( 'NONE', *, *, #794, .T. ) ;
#79102 = DIRECTION ( 'NONE',  ( 0.000000000000000000, 0.000000000000000000, -1.000000000000000000 ) ) ;
#79103 = ORIENTED_EDGE ( 'NONE', *, *, #69950, .F. ) ;
#79104 = FACE_OUTER_BOUND ( 'NONE', #16966, .T. ) ;
#79105 = CARTESIAN_POINT ( 'NONE',  ( -2.000000000000000000, 2.449293598294706414E-16, -5.000000000000004441 ) ) ;
#79106 = CYLINDRICAL_SURFACE ( 'NONE', #32047, 7.699999999999999289 ) ;
#79108 = EDGE_CURVE ( 'NONE', #12415, #75136, #128068, .T. ) ;
#79107 = CARTESIAN_POINT ( 'NONE',  ( 12.94999999999989981, 12.50000000000000000, -2.165063509461101710 ) ) ;
#79109 = CARTESIAN_POINT ( 'NONE',  ( 7.699999999999922018, 12.50000000000000000, 0.4115034346978109769 ) ) ;
#79110 = ORIENTED_EDGE ( 'NONE', *, *, #47546, .F. ) ;
#79111 = ORIENTED_EDGE ( 'NONE', *, *, #92558, .T. ) ;
#79112 = ORIENTED_EDGE ( 'NONE', *, *, #84745, .T. ) ;
#79113 = CARTESIAN_POINT ( 'NONE',  ( 5.799999999999934985, 2.500000000000000000, -4.430127018922202176 ) ) ;
#79114 = LINE ( 'NONE', #128208, #32778 ) ;
#79115 = FACE_OUTER_BOUND ( 'NONE', #83373, .T. ) ;
#79118 = ORIENTED_EDGE ( 'NONE', *, *, #120501, .F. ) ;
#79117 = VERTEX_POINT ( 'NONE', #118666 ) ;
#79116 = CIRCLE ( 'NONE', #31096, 0.1000000000000002554 ) ;
#79119 = VERTEX_POINT ( 'NONE', #40788 ) ;
#79120 = CARTESIAN_POINT ( 'NONE',  ( 14.99999999999989164, 2.500000000000000000, 0.7928203230275495672 ) ) ;
#79121 = DIRECTION ( 'NONE',  ( -1.000000000000000000, -0.000000000000000000, -0.000000000000000000 ) ) ;
#79122 = AXIS2_PLACEMENT_3D ( 'NONE', #29563, #39414, #70145 ) ;
#79124 = DIRECTION ( 'NONE',  ( 0.000000000000000000, -0.000000000000000000, 1.000000000000000000 ) ) ;
#79123 = VECTOR ( 'NONE', #2984, 1000.000000000000000 ) ;
#79125 = DIRECTION ( 'NONE',  ( 0.000000000000000000, 0.000000000000000000, 1.000000000000000000 ) ) ;
#79126 = CARTESIAN_POINT ( 'NONE',  ( -10.45000000000000462, 2.500000000000000000, -6.595190528383298556 ) ) ;
#79127 = DIRECTION ( 'NONE',  ( 0.000000000000000000, 1.000000000000000000, 0.000000000000000000 ) ) ;
#79128 = DIRECTION ( 'NONE',  ( 0.000000000000000000, 0.000000000000000000, 1.000000000000000000 ) ) ;
#79129 = FACE_OUTER_BOUND ( 'NONE', #68315, .T. ) ;
#79130 = AXIS2_PLACEMENT_3D ( 'NONE', #112261, #2279, #5346 ) ;
#79131 = VERTEX_POINT ( 'NONE', #101627 ) ;
#79133 = EDGE_LOOP ( 'NONE', ( #89365, #60409 ) ) ;
#79132 = CIRCLE ( 'NONE', #22697, 0.09999999999999999167 ) ;
#79134 = EDGE_CURVE ( 'NONE', #26297, #1525, #30960, .T. ) ;
#79136 = DIRECTION ( 'NONE',  ( 0.000000000000000000, -0.000000000000000000, 1.000000000000000000 ) ) ;
#79135 = VECTOR ( 'NONE', #93661, 1000.000000000000000 ) ;
#79137 = DIRECTION ( 'NONE',  ( -0.000000000000000000, -1.000000000000000000, -0.000000000000000000 ) ) ;
#79138 = EDGE_LOOP ( 'NONE', ( #17134, #113833, #117488, #63872 ) ) ;
#79139 = ORIENTED_EDGE ( 'NONE', *, *, #117779, .F. ) ;
#79140 = EDGE_CURVE ( 'NONE', #20502, #47459, #19284, .T. ) ;
#79141 = CARTESIAN_POINT ( 'NONE',  ( 186.3593750003414016, 0.000000000000000000, 7.564683531250000925 ) ) ;
#79142 = DIRECTION ( 'NONE',  ( 0.000000000000000000, 0.000000000000000000, -1.000000000000000000 ) ) ;
#79143 = CARTESIAN_POINT ( 'NONE',  ( -13.74999999999995381, 12.50000000000000000, -2.165063509461099489 ) ) ;
#79145 = EDGE_CURVE ( 'NONE', #120749, #21424, #21447, .T. ) ;
#79144 = AXIS2_PLACEMENT_3D ( 'NONE', #39550, #59170, #9416 ) ;
#79146 = CARTESIAN_POINT ( 'NONE',  ( -2.050000000000032685, 2.500000000000000000, -2.065063509461102065 ) ) ;
#79147 = VECTOR ( 'NONE', #117754, 1000.000000000000000 ) ;
#79148 = CARTESIAN_POINT ( 'NONE',  ( 5.849999999999932143, 2.500000000000000000, 1.572243186433545548 ) ) ;
#79149 = DIRECTION ( 'NONE',  ( 0.000000000000000000, 1.000000000000000000, 0.000000000000000000 ) ) ;
#79150 = LINE ( 'NONE', #68019, #85407 ) ;
#79151 = EDGE_CURVE ( 'NONE', #24359, #23899, #88561, .T. ) ;
#79152 = EDGE_CURVE ( 'NONE', #119576, #39789, #17212, .T. ) ;
#79153 = EDGE_CURVE ( 'NONE', #89280, #54263, #31924, .T. ) ;
#79154 = DIRECTION ( 'NONE',  ( 0.000000000000000000, -0.000000000000000000, 1.000000000000000000 ) ) ;
#79155 = CIRCLE ( 'NONE', #20656, 0.06509327318403741736 ) ;
#79156 = ORIENTED_EDGE ( 'NONE', *, *, #96712, .T. ) ;
#79157 = EDGE_CURVE ( 'NONE', #34557, #24306, #46478, .T. ) ;
#79158 = ORIENTED_EDGE ( 'NONE', *, *, #94242, .T. ) ;
#79159 = CLOSED_SHELL ( 'NONE', ( #35992, #44206, #23962, #71006, #90669, #119020, #60205, #81435, #43519, #91832, #26070, #106782, #34979, #37376, #39327, #33335, #13139, #94184, #100289, #8660, #103003, #48814, #85650, #50480, #122277, #55783, #77589, #1819, #98128, #113920, #47131, #75565, #109141, #23021, #14914, #81885, #33929, #108267, #72146, #69832, #121906, #129240, #66265, #104391, #114709, #35407, #63610, #44718, #56483, #114147, #72726, #57424, #32030, #33949, #88081, #124217, #37942, #42290, #59542, #1226 ) ) ;
#79160 = AXIS2_PLACEMENT_3D ( 'NONE', #76728, #38097, #129078 ) ;
#79161 = ORIENTED_EDGE ( 'NONE', *, *, #46171, .T. ) ;
#79162 = ORIENTED_EDGE ( 'NONE', *, *, #77399, .T. ) ;
#79163 = CARTESIAN_POINT ( 'NONE',  ( 4.149999999999939959, 12.50000000000000000, -2.165063509461101710 ) ) ;
#79164 = DIRECTION ( 'NONE',  ( -0.000000000000000000, -1.000000000000000000, -0.000000000000000000 ) ) ;
#79165 = EDGE_CURVE ( 'NONE', #13562, #3295, #33979, .T. ) ;
#79166 = CONICAL_SURFACE ( 'NONE', #16418, 0.09999999999999982514, 0.003490658503988666988 ) ;
#79167 = ORIENTED_EDGE ( 'NONE', *, *, #66936, .T. ) ;
#79168 = CARTESIAN_POINT ( 'NONE',  ( 6.249999999999930722, 2.500000000000000000, 1.572243186433545548 ) ) ;
#79169 = LINE ( 'NONE', #48400, #69603 ) ;
#79170 = CARTESIAN_POINT ( 'NONE',  ( -5.800000000000022027, 12.50000000000000000, -4.330127018922201643 ) ) ;
#79172 = VERTEX_POINT ( 'NONE', #89851 ) ;
#79171 = DIRECTION ( 'NONE',  ( 0.000000000000000000, 0.000000000000000000, 1.000000000000000000 ) ) ;
#79173 = CARTESIAN_POINT ( 'NONE',  ( -15.59999999999998010, 12.50000000000000000, -0.4115034346978133639 ) ) ;
#79174 = CIRCLE ( 'NONE', #112527, 0.09999999999999982514 ) ;
#79175 = CARTESIAN_POINT ( 'NONE',  ( -12.89999999999999147, 12.50000000000000000, 4.330127018922196314 ) ) ;
#79176 = ORIENTED_EDGE ( 'NONE', *, *, #10662, .F. ) ;
#79177 = AXIS2_PLACEMENT_3D ( 'NONE', #128291, #17667, #38632 ) ;
#79178 = EDGE_LOOP ( 'NONE', ( #24730, #116588 ) ) ;
#79179 = EDGE_LOOP ( 'NONE', ( #42384, #101000, #122005, #64273 ) ) ;
#79180 = VERTEX_POINT ( 'NONE', #40120 ) ;
#79181 = CARTESIAN_POINT ( 'NONE',  ( 3.099999999999944134, 12.50000000000000000, 4.676537180435972552 ) ) ;
#79182 = FACE_OUTER_BOUND ( 'NONE', #26744, .T. ) ;
#79183 = DIRECTION ( 'NONE',  ( 0.000000000000000000, 0.000000000000000000, 1.000000000000000000 ) ) ;
#79184 = AXIS2_PLACEMENT_3D ( 'NONE', #26225, #123753, #104751 ) ;
#79185 = VERTEX_POINT ( 'NONE', #81966 ) ;
#79186 = CARTESIAN_POINT ( 'NONE',  ( 8.149999999999923972, 2.500000000000000000, 2.411473670974873862 ) ) ;
#79188 = CONICAL_SURFACE ( 'NONE', #22854, 0.1000000000000002554, 0.003490658503988666988 ) ;
#79187 = PLANE ( 'NONE',  #68416 ) ;
#79189 = CARTESIAN_POINT ( 'NONE',  ( -2.900000000000029221, 12.50000000000000000, -2.276824562219559311E-15 ) ) ;
#79190 = FACE_OUTER_BOUND ( 'NONE', #1871, .T. ) ;
#79191 = ORIENTED_EDGE ( 'NONE', *, *, #72789, .T. ) ;
#79193 = CIRCLE ( 'NONE', #77030, 0.06509327318403745899 ) ;
#79192 = CONICAL_SURFACE ( 'NONE', #95901, 0.09999999999999982514, 0.003490658503988666988 ) ;
#79194 = FACE_OUTER_BOUND ( 'NONE', #23821, .T. ) ;
#79195 = ADVANCED_FACE ( 'NONE', ( #23056 ), #36030, .T. ) ;
#79196 = ORIENTED_EDGE ( 'NONE', *, *, #127785, .F. ) ;
#79197 = ORIENTED_EDGE ( 'NONE', *, *, #55022, .F. ) ;
#79198 = FACE_OUTER_BOUND ( 'NONE', #80714, .T. ) ;
#79199 = DIRECTION ( 'NONE',  ( 0.000000000000000000, 0.000000000000000000, -1.000000000000000000 ) ) ;
#79200 = FACE_BOUND ( 'NONE', #128131, .T. ) ;
#79201 = CARTESIAN_POINT ( 'NONE',  ( 9.999999999999912959, 2.500000000000000000, 3.737306695894644371 ) ) ;
#79202 = CARTESIAN_POINT ( 'NONE',  ( 14.99999999999989342, 12.50000000000000000, -0.6928203230275541413 ) ) ;
#79203 = DIRECTION ( 'NONE',  ( 0.000000000000000000, 0.000000000000000000, 1.000000000000000000 ) ) ;
#79204 = EDGE_CURVE ( 'NONE', #87232, #55744, #2554, .T. ) ;
#79205 = VERTEX_POINT ( 'NONE', #3412 ) ;
#79206 = CARTESIAN_POINT ( 'NONE',  ( -4.800000000000028244, 12.50000000000000000, -3.983716857408426293 ) ) ;
#79207 = DIRECTION ( 'NONE',  ( -0.000000000000000000, 1.000000000000000000, -0.000000000000000000 ) ) ;
#79208 = DIRECTION ( 'NONE',  ( -0.000000000000000000, 1.000000000000000000, -0.000000000000000000 ) ) ;
#79209 = CARTESIAN_POINT ( 'NONE',  ( 186.4479166673494603, -6.668395609140176816, -3.850000000000003642 ) ) ;
#79210 = VERTEX_POINT ( 'NONE', #84550 ) ;
#79211 = CARTESIAN_POINT ( 'NONE',  ( 0.3999999999999628852, 2.500000000000000000, -0.6928203230275520319 ) ) ;
#79212 = AXIS2_PLACEMENT_3D ( 'NONE', #20542, #60483, #4556 ) ;
#79213 = FACE_OUTER_BOUND ( 'NONE', #104002, .T. ) ;
#79214 = VERTEX_POINT ( 'NONE', #64895 ) ;
#79215 = ORIENTED_EDGE ( 'NONE', *, *, #92306, .T. ) ;
#79216 = DIRECTION ( 'NONE',  ( 0.000000000000000000, 0.000000000000000000, -1.000000000000000000 ) ) ;
#79217 = CARTESIAN_POINT ( 'NONE',  ( -9.200000000000006395, 2.500000000000000000, 4.430127018922196847 ) ) ;
#79218 = FACE_BOUND ( 'NONE', #4373, .T. ) ;
#79219 = DIRECTION ( 'NONE',  ( 0.000000000000000000, 0.000000000000000000, -1.000000000000000000 ) ) ;
#79220 = CIRCLE ( 'NONE', #58388, 0.06509327318403745899 ) ;
#79221 = AXIS2_PLACEMENT_3D ( 'NONE', #113891, #44495, #54957 ) ;
#79222 = VECTOR ( 'NONE', #126771, 1000.000000000000000 ) ;
#79223 = DIRECTION ( 'NONE',  ( -0.000000000000000000, -1.000000000000000000, -0.000000000000000000 ) ) ;
#79224 = ORIENTED_EDGE ( 'NONE', *, *, #38630, .F. ) ;
#79225 = CARTESIAN_POINT ( 'NONE',  ( 5.599999999999934808, 12.50000000000000000, -4.741630453620016006 ) ) ;
#79226 = CARTESIAN_POINT ( 'NONE',  ( 184.5416666666666572, -4.445597072760122614, 7.699999999999998401 ) ) ;
#79227 = AXIS2_PLACEMENT_3D ( 'NONE', #98492, #88692, #38985 ) ;
#79228 = ORIENTED_EDGE ( 'NONE', *, *, #110861, .F. ) ;
#79229 = DIRECTION ( 'NONE',  ( -0.000000000000000000, -1.000000000000000000, -0.000000000000000000 ) ) ;
#79230 = DIRECTION ( 'NONE',  ( 0.000000000000000000, 0.000000000000000000, 1.000000000000000000 ) ) ;
#79232 = ADVANCED_FACE ( 'NONE', ( #42056 ), #96644, .T. ) ;
#79231 = AXIS2_PLACEMENT_3D ( 'NONE', #29410, #9759, #49704 ) ;
#79233 = DIRECTION ( 'NONE',  ( 0.000000000000000000, 1.000000000000000000, 0.000000000000000000 ) ) ;
#79234 = CARTESIAN_POINT ( 'NONE',  ( 8.549999999999920774, 2.500000000000000000, 6.148780366869520897 ) ) ;
#79236 = ADVANCED_FACE ( 'NONE', ( #72806 ), #94595, .T. ) ;
#79235 = AXIS2_PLACEMENT_3D ( 'NONE', #4848, #26450, #42381 ) ;
#79237 = ORIENTED_EDGE ( 'NONE', *, *, #129164, .T. ) ;
#79238 = CARTESIAN_POINT ( 'NONE',  ( 3.149999999999942624, 2.500000000000000000, 6.148780366869520897 ) ) ;
#79239 = FACE_OUTER_BOUND ( 'NONE', #57745, .T. ) ;
#79240 = CARTESIAN_POINT ( 'NONE',  ( -12.94999999999999218, 12.50000000000000000, 2.099970236277064028 ) ) ;
#79241 = AXIS2_PLACEMENT_3D ( 'NONE', #64654, #36507, #26029 ) ;
#79242 = CARTESIAN_POINT ( 'NONE',  ( -9.150000000000009237, 2.500000000000000000, -1.572243186433550211 ) ) ;
#79243 = VERTEX_POINT ( 'NONE', #23700 ) ;
#79244 = ADVANCED_FACE ( 'NONE', ( #54436 ), #82086, .T. ) ;
#79245 = ORIENTED_EDGE ( 'NONE', *, *, #27421, .F. ) ;
#79246 = EDGE_CURVE ( 'NONE', #40987, #18162, #115517, .T. ) ;
#79247 = CARTESIAN_POINT ( 'NONE',  ( 2.499999999999948930, 12.50000000000000000, -5.022947341949754119 ) ) ;
#79248 = ORIENTED_EDGE ( 'NONE', *, *, #60685, .T. ) ;
#79249 = CARTESIAN_POINT ( 'NONE',  ( 6.649999999999930189, 2.500000000000000000, 5.902370205355745192 ) ) ;
#79250 = CARTESIAN_POINT ( 'NONE',  ( 17.50000000000000000, -2.499999999999999556, -0.6666666666666614116 ) ) ;
#79251 = CARTESIAN_POINT ( 'NONE',  ( -8.100000000000013856, 2.500000000000000000, -3.983716857408426293 ) ) ;
#79252 = DIRECTION ( 'NONE',  ( -0.000000000000000000, -1.000000000000000000, -0.000000000000000000 ) ) ;
#79253 = ORIENTED_EDGE ( 'NONE', *, *, #41783, .T. ) ;
#79254 = AXIS2_PLACEMENT_3D ( 'NONE', #114233, #6190, #5552 ) ;
#79255 = ADVANCED_FACE ( 'NONE', ( #13216 ), #15165, .T. ) ;
#79256 = CARTESIAN_POINT ( 'NONE',  ( 9.349999999999916156, 12.50000000000000000, -2.511473670974877948 ) ) ;
#79257 = DIRECTION ( 'NONE',  ( 0.000000000000000000, 0.000000000000000000, 1.000000000000000000 ) ) ;
#79258 = DIRECTION ( 'NONE',  ( -0.000000000000000000, 1.000000000000000000, -0.000000000000000000 ) ) ;
#79259 = CARTESIAN_POINT ( 'NONE',  ( 184.8593750003413732, 0.000000000000000000, 7.564683531250000925 ) ) ;
#79260 = CARTESIAN_POINT ( 'NONE',  ( 8.749999999999923617, 2.500000000000000000, 1.572243186433545548 ) ) ;
#79261 = EDGE_CURVE ( 'NONE', #25034, #35273, #73668, .T. ) ;
#79262 = CONICAL_SURFACE ( 'NONE', #110543, 0.1000000000000002554, 0.003490658503988666988 ) ;
#79263 = LINE ( 'NONE', #126419, #118355 ) ;
#79265 = ORIENTED_EDGE ( 'NONE', *, *, #120172, .F. ) ;
#79264 = AXIS2_PLACEMENT_3D ( 'NONE', #10433, #40567, #50359 ) ;
#79266 = EDGE_LOOP ( 'NONE', ( #23585, #67998 ) ) ;
#79267 = FACE_OUTER_BOUND ( 'NONE', #105586, .T. ) ;
#79268 = ORIENTED_EDGE ( 'NONE', *, *, #6872, .F. ) ;
#79269 = CARTESIAN_POINT ( 'NONE',  ( -0.8500000000000382805, 12.50000000000000000, -5.737276932171712751 ) ) ;
#79271 = ORIENTED_EDGE ( 'NONE', *, *, #127694, .F. ) ;
#79270 = ORIENTED_EDGE ( 'NONE', *, *, #42028, .T. ) ;
#79272 = EDGE_LOOP ( 'NONE', ( #105068, #51605, #123445, #83156 ) ) ;
#79273 = AXIS2_PLACEMENT_3D ( 'NONE', #120144, #91322, #347 ) ;
#79274 = DIRECTION ( 'NONE',  ( 0.000000000000000000, -0.000000000000000000, 1.000000000000000000 ) ) ;
#79275 = DIRECTION ( 'NONE',  ( 0.000000000000000000, 0.000000000000000000, 1.000000000000000000 ) ) ;
#79276 = CARTESIAN_POINT ( 'NONE',  ( -10.20000000000000284, 12.50000000000000000, -0.2813168883297408329 ) ) ;
#79277 = FILL_AREA_STYLE_COLOUR ( '', #77000 ) ;
#79279 = VECTOR ( 'NONE', #81133, 1000.000000000000000 ) ;
#79278 = AXIS2_PLACEMENT_3D ( 'NONE', #56114, #81867, #35846 ) ;
#79280 = LINE ( 'NONE', #30831, #13816 ) ;
#79281 = DIRECTION ( 'NONE',  ( 0.000000000000000000, 0.000000000000000000, 1.000000000000000000 ) ) ;
#79282 = LINE ( 'NONE', #110025, #83605 ) ;
#79283 = DIRECTION ( 'NONE',  ( 0.000000000000000000, -1.846105847067148022E-16, 1.000000000000000000 ) ) ;
#79284 = DIRECTION ( 'NONE',  ( -4.274815082592931898E-19, -0.9999939076577903929, -0.003490651415223739937 ) ) ;
#79285 = AXIS2_PLACEMENT_3D ( 'NONE', #111583, #51396, #79551 ) ;
#79286 = CARTESIAN_POINT ( 'NONE',  ( -1.850000000000033840, 2.500000000000000000, 2.511473670974873507 ) ) ;
#79287 = ORIENTED_EDGE ( 'NONE', *, *, #72768, .F. ) ;
#79289 = CIRCLE ( 'NONE', #60511, 0.06509327318403745899 ) ;
#79288 = AXIS2_PLACEMENT_3D ( 'NONE', #31974, #62077, #111139 ) ;
#79290 = ORIENTED_EDGE ( 'NONE', *, *, #105449, .T. ) ;
#79291 = FACE_OUTER_BOUND ( 'NONE', #93935, .T. ) ;
#79292 = ORIENTED_EDGE ( 'NONE', *, *, #2939, .F. ) ;
#79293 = EDGE_LOOP ( 'NONE', ( #44242, #107599 ) ) ;
#79294 = DIRECTION ( 'NONE',  ( 0.000000000000000000, 1.000000000000000000, 0.000000000000000000 ) ) ;
#79295 = EDGE_CURVE ( 'NONE', #112355, #7480, #71619, .T. ) ;
#79296 = DIRECTION ( 'NONE',  ( 0.000000000000000000, 1.000000000000000000, 0.000000000000000000 ) ) ;
#79297 = PLANE ( 'NONE',  #61116 ) ;
#79298 = CARTESIAN_POINT ( 'NONE',  ( -5.850000000000021849, 2.500000000000000000, -2.757883832488654097 ) ) ;
#79299 = EDGE_CURVE ( 'NONE', #94406, #120997, #505, .T. ) ;
#79301 = AXIS2_PLACEMENT_3D ( 'NONE', #12717, #112876, #13374 ) ;
#79300 = CARTESIAN_POINT ( 'NONE',  ( 0.4499999999999569344, 12.50000000000000000, 2.165063509461097713 ) ) ;
#79302 = ORIENTED_EDGE ( 'NONE', *, *, #94886, .T. ) ;
#79303 = ADVANCED_FACE ( 'NONE', ( #12573 ), #113388, .T. ) ;
#79304 = EDGE_CURVE ( 'NONE', #21644, #38111, #69465, .T. ) ;
#79305 = ADVANCED_FACE ( 'NONE', ( #34174 ), #77978, .T. ) ;
#79306 = ORIENTED_EDGE ( 'NONE', *, *, #16186, .T. ) ;
#79308 = DIRECTION ( 'NONE',  ( 0.000000000000000000, 0.000000000000000000, 1.000000000000000000 ) ) ;
#79307 = AXIS2_PLACEMENT_3D ( 'NONE', #83039, #72571, #122317 ) ;
#79310 = VERTEX_POINT ( 'NONE', #114019 ) ;
#79309 = AXIS2_PLACEMENT_3D ( 'NONE', #127593, #68665, #69296 ) ;
#79311 = FACE_OUTER_BOUND ( 'NONE', #92578, .T. ) ;
#79312 = ADVANCED_FACE ( 'NONE', ( #24350 ), #64259, .T. ) ;
#79313 = EDGE_LOOP ( 'NONE', ( #93474, #10112, #23911, #55293 ) ) ;
#79314 = ORIENTED_EDGE ( 'NONE', *, *, #73819, .F. ) ;
#79316 = AXIS2_PLACEMENT_3D ( 'NONE', #74163, #114084, #14575 ) ;
#79315 = CARTESIAN_POINT ( 'NONE',  ( 3.349999999999941913, 12.50000000000000000, 6.495190528383297135 ) ) ;
#79317 = DIRECTION ( 'NONE',  ( 0.000000000000000000, -0.000000000000000000, 1.000000000000000000 ) ) ;
#79319 = EDGE_CURVE ( 'NONE', #47762, #46559, #111410, .T. ) ;
#79318 = AXIS2_PLACEMENT_3D ( 'NONE', #38413, #78335, #108411 ) ;
#79320 = AXIS2_PLACEMENT_3D ( 'NONE', #65568, #97606, #106770 ) ;
#79321 = ADVANCED_FACE ( 'NONE', ( #2108 ), #82632, .T. ) ;
#79322 = DIRECTION ( 'NONE',  ( 0.000000000000000000, 0.000000000000000000, -1.000000000000000000 ) ) ;
#79323 = CARTESIAN_POINT ( 'NONE',  ( -10.65000000000000213, 2.500000000000000000, 1.818653347947321475 ) ) ;
#79324 = DIRECTION ( 'NONE',  ( 0.000000000000000000, 0.000000000000000000, 1.000000000000000000 ) ) ;
#79325 = ORIENTED_EDGE ( 'NONE', *, *, #107208, .F. ) ;
#79326 = DIRECTION ( 'NONE',  ( 0.000000000000000000, 0.000000000000000000, 1.000000000000000000 ) ) ;
#79327 = CARTESIAN_POINT ( 'NONE',  ( 2.699999999999946443, 2.500000000000000000, 0.2464101615137735679 ) ) ;
#79328 = DIRECTION ( 'NONE',  ( 0.000000000000000000, 1.000000000000000000, 0.000000000000000000 ) ) ;
#79329 = DIRECTION ( 'NONE',  ( 0.000000000000000000, 0.000000000000000000, 1.000000000000000000 ) ) ;
#79330 = AXIS2_PLACEMENT_3D ( 'NONE', #78072, #68244, #58449 ) ;
#79331 = DIRECTION ( 'NONE',  ( -0.000000000000000000, -1.000000000000000000, -0.000000000000000000 ) ) ;
#79332 = AXIS2_PLACEMENT_3D ( 'NONE', #910, #50042, #9451 ) ;
#79333 = ORIENTED_EDGE ( 'NONE', *, *, #44271, .T. ) ;
#79334 = CONICAL_SURFACE ( 'NONE', #85570, 0.1000000000000000472, 0.003490658503988666988 ) ;
#79335 = ORIENTED_EDGE ( 'NONE', *, *, #47488, .F. ) ;
#79336 = PLANE ( 'NONE',  #119788 ) ;
#79337 = EDGE_LOOP ( 'NONE', ( #62804, #70960, #94603, #122049 ) ) ;
#79338 = DIRECTION ( 'NONE',  ( -0.000000000000000000, -1.000000000000000000, -0.000000000000000000 ) ) ;
#79339 = DIRECTION ( 'NONE',  ( -0.000000000000000000, -1.000000000000000000, -0.000000000000000000 ) ) ;
#79340 = CIRCLE ( 'NONE', #106415, 0.1000000000000002554 ) ;
#79341 = ORIENTED_EDGE ( 'NONE', *, *, #28157, .F. ) ;
#79342 = DIRECTION ( 'NONE',  ( -4.274815082592931898E-19, -0.9999939076577903929, -0.003490651415223739937 ) ) ;
#79343 = CARTESIAN_POINT ( 'NONE',  ( -3.350000000000028955, 2.500000000000000000, 5.702370205355745014 ) ) ;
#79344 = DIRECTION ( 'NONE',  ( -0.000000000000000000, -1.000000000000000000, -0.000000000000000000 ) ) ;
#79345 = CARTESIAN_POINT ( 'NONE',  ( 5.399999999999934630, 12.50000000000000000, -0.6928203230275542523 ) ) ;
#79346 = ORIENTED_EDGE ( 'NONE', *, *, #125521, .T. ) ;
#79347 = DIRECTION ( 'NONE',  ( -0.000000000000000000, 1.000000000000000000, -0.000000000000000000 ) ) ;
#79348 = EDGE_LOOP ( 'NONE', ( #46837, #52467 ) ) ;
#79349 = DIRECTION ( 'NONE',  ( 0.000000000000000000, 1.000000000000000000, 0.000000000000000000 ) ) ;
#79350 = AXIS2_PLACEMENT_3D ( 'NONE', #102310, #12615, #95064 ) ;
#79351 = DIRECTION ( 'NONE',  ( -1.000000000000000000, -0.000000000000000000, -0.000000000000000000 ) ) ;
#79352 = DIRECTION ( 'NONE',  ( 0.000000000000000000, 1.000000000000000000, 0.000000000000000000 ) ) ;
#79353 = ADVANCED_FACE ( 'NONE', ( #117195 ), #5334, .T. ) ;
#79354 = VERTEX_POINT ( 'NONE', #107409 ) ;
#79355 = CARTESIAN_POINT ( 'NONE',  ( 6.649999999999931966, 12.50000000000000000, -5.737276932171712751 ) ) ;
#79356 = ORIENTED_EDGE ( 'NONE', *, *, #26816, .F. ) ;
#79358 = AXIS2_PLACEMENT_3D ( 'NONE', #49983, #194, #80065 ) ;
#79357 = FACE_OUTER_BOUND ( 'NONE', #113178, .T. ) ;
#79359 = FACE_OUTER_BOUND ( 'NONE', #125735, .T. ) ;
#79360 = DIRECTION ( 'NONE',  ( 0.000000000000000000, 0.000000000000000000, 1.000000000000000000 ) ) ;
#79361 = VERTEX_POINT ( 'NONE', #115263 ) ;
#79362 = DIRECTION ( 'NONE',  ( 0.000000000000000000, 0.000000000000000000, -1.000000000000000000 ) ) ;
#79364 = CIRCLE ( 'NONE', #98123, 0.06509327318403741736 ) ;
#79363 = CIRCLE ( 'NONE', #56352, 0.1000000000000002554 ) ;
#79365 = DIRECTION ( 'NONE',  ( -4.274815082592931898E-19, -0.9999939076577903929, -0.003490651415223739937 ) ) ;
#79366 = ORIENTED_EDGE ( 'NONE', *, *, #29814, .T. ) ;
#79367 = DIRECTION ( 'NONE',  ( -0.000000000000000000, -1.000000000000000000, -0.000000000000000000 ) ) ;
#79368 = ORIENTED_EDGE ( 'NONE', *, *, #65483, .F. ) ;
#79369 = DIRECTION ( 'NONE',  ( -0.000000000000000000, -1.000000000000000000, -0.000000000000000000 ) ) ;
#79371 = CIRCLE ( 'NONE', #22938, 0.06509327318403745899 ) ;
#79370 = CIRCLE ( 'NONE', #54233, 0.06509327318403745899 ) ;
#79372 = ORIENTED_EDGE ( 'NONE', *, *, #65791, .T. ) ;
#79373 = CARTESIAN_POINT ( 'NONE',  ( 4.399999999999937295, 2.500000000000000000, 4.776537180435972196 ) ) ;
#79374 = CARTESIAN_POINT ( 'NONE',  ( 10.04522989427052160, 2.499999999999999112, -8.164691043833789408 ) ) ;
#79375 = EDGE_LOOP ( 'NONE', ( #108147, #94111 ) ) ;
#79376 = ORIENTED_EDGE ( 'NONE', *, *, #108672, .F. ) ;
#79377 = PLANE ( 'NONE',  #33141 ) ;
#79378 = DIRECTION ( 'NONE',  ( -0.000000000000000000, 1.000000000000000000, -0.000000000000000000 ) ) ;
#79379 = EDGE_LOOP ( 'NONE', ( #20005, #105734, #59640, #6189 ) ) ;
#79380 = CARTESIAN_POINT ( 'NONE',  ( 3.949999999999942446, 2.500000000000000000, -6.941600689897078347 ) ) ;
#79381 = CARTESIAN_POINT ( 'NONE',  ( 186.5260416670080588, -6.551208109652273848, -3.782341765625003571 ) ) ;
#79382 = DIRECTION ( 'NONE',  ( 0.000000000000000000, 0.000000000000000000, 1.000000000000000000 ) ) ;
#79383 = CARTESIAN_POINT ( 'NONE',  ( 103.6750765693973761, 8.328912879160041527, 2.529530674324913964 ) ) ;
#79384 = CARTESIAN_POINT ( 'NONE',  ( -11.05000000000000071, 2.500000000000000000, 2.511473670974873507 ) ) ;
#79385 = CARTESIAN_POINT ( 'NONE',  ( -4.150000000000024336, 2.500000000000000000, -2.165063509461101710 ) ) ;
#79386 = DIRECTION ( 'NONE',  ( 0.000000000000000000, -0.9999939076577903929, 0.003490651415223739937 ) ) ;
#79387 = CIRCLE ( 'NONE', #31368, 0.09999999999999982514 ) ;
#79388 = ADVANCED_FACE ( 'NONE', ( #35463 ), #92545, .T. ) ;
#79389 = CIRCLE ( 'NONE', #93961, 0.1000000000000000472 ) ;
#79390 = ORIENTED_EDGE ( 'NONE', *, *, #41288, .F. ) ;
#79391 = ORIENTED_EDGE ( 'NONE', *, *, #21171, .F. ) ;
#79392 = VERTEX_POINT ( 'NONE', #55731 ) ;
#79393 = ORIENTED_EDGE ( 'NONE', *, *, #106874, .T. ) ;
#79394 = CARTESIAN_POINT ( 'NONE',  ( 1.649999999999951505, 2.500000000000000000, -1.472243186433550122 ) ) ;
#79395 = DIRECTION ( 'NONE',  ( -0.000000000000000000, 1.000000000000000000, -0.000000000000000000 ) ) ;
#79396 = DIRECTION ( 'NONE',  ( 0.000000000000000000, 0.000000000000000000, 1.000000000000000000 ) ) ;
#79397 = ORIENTED_EDGE ( 'NONE', *, *, #97344, .F. ) ;
#79398 = EDGE_CURVE ( 'NONE', #76857, #32813, #25739, .T. ) ;
#79399 = FACE_BOUND ( 'NONE', #96938, .T. ) ;
#79400 = ORIENTED_EDGE ( 'NONE', *, *, #108724, .F. ) ;
#79401 = EDGE_CURVE ( 'NONE', #85979, #58087, #23596, .T. ) ;
#79402 = CARTESIAN_POINT ( 'NONE',  ( 14.14999999999989555, 2.500000000000000000, 2.265063509461097357 ) ) ;
#79403 = DIRECTION ( 'NONE',  ( 0.000000000000000000, 1.000000000000000000, 0.000000000000000000 ) ) ;
#79404 = AXIS2_PLACEMENT_3D ( 'NONE', #72715, #51154, #21687 ) ;
#79405 = AXIS2_PLACEMENT_3D ( 'NONE', #114223, #14061, #74944 ) ;
#79406 = DIRECTION ( 'NONE',  ( 0.000000000000000000, 1.000000000000000000, 0.000000000000000000 ) ) ;
#79407 = CARTESIAN_POINT ( 'NONE',  ( 7.049999999999930544, 12.50000000000000000, -6.495190528383302464 ) ) ;
#79408 = CARTESIAN_POINT ( 'NONE',  ( 9.999999999999911182, 2.500000000000000000, -3.537306695894649966 ) ) ;
#79409 = EDGE_CURVE ( 'NONE', #81872, #34821, #127690, .T. ) ;
#79410 = FACE_OUTER_BOUND ( 'NONE', #53380, .T. ) ;
#79411 = EDGE_CURVE ( 'NONE', #40041, #26625, #87119, .T. ) ;
#79412 = FACE_OUTER_BOUND ( 'NONE', #7463, .T. ) ;
#79413 = DIRECTION ( 'NONE',  ( 0.000000000000000000, 0.000000000000000000, -1.000000000000000000 ) ) ;
#79414 = EDGE_CURVE ( 'NONE', #56250, #42358, #15796, .T. ) ;
#79415 = DIRECTION ( 'NONE',  ( 0.000000000000000000, 1.000000000000000000, 0.000000000000000000 ) ) ;
#79416 = ADVANCED_FACE ( 'NONE', ( #117859 ), #42491, .T. ) ;
#79417 = CONICAL_SURFACE ( 'NONE', #60551, 0.1000000000000002554, 0.003490658503988666988 ) ;
#79418 = PLANE ( 'NONE',  #12553 ) ;
#79419 = CIRCLE ( 'NONE', #37647, 0.1000000000000000472 ) ;
#79420 = EDGE_LOOP ( 'NONE', ( #51840, #48212, #124102, #25603 ) ) ;
#79421 = VERTEX_POINT ( 'NONE', #15138 ) ;
#79422 = VECTOR ( 'NONE', #71440, 1000.000000000000000 ) ;
#79423 = ORIENTED_EDGE ( 'NONE', *, *, #73250, .T. ) ;
#79424 = ORIENTED_EDGE ( 'NONE', *, *, #8893, .T. ) ;
#79425 = DIRECTION ( 'NONE',  ( -0.000000000000000000, -1.000000000000000000, -0.000000000000000000 ) ) ;
#79426 = CARTESIAN_POINT ( 'NONE',  ( 1.849999999999950129, 2.500000000000000000, -6.741600689897078169 ) ) ;
#79428 = ORIENTED_EDGE ( 'NONE', *, *, #62386, .T. ) ;
#79427 = ORIENTED_EDGE ( 'NONE', *, *, #58566, .T. ) ;
#79429 = EDGE_CURVE ( 'NONE', #34708, #78443, #29865, .T. ) ;
#79430 = ORIENTED_EDGE ( 'NONE', *, *, #60576, .T. ) ;
#79431 = DIRECTION ( 'NONE',  ( 0.000000000000000000, 0.000000000000000000, 1.000000000000000000 ) ) ;
#79432 = CARTESIAN_POINT ( 'NONE',  ( -5.200000000000020606, 2.500000000000000000, -0.3464101615137782364 ) ) ;
#79433 = CARTESIAN_POINT ( 'NONE',  ( 13.74999999999989342, 2.500000000000000000, -1.472243186433550122 ) ) ;
#79434 = CARTESIAN_POINT ( 'NONE',  ( -14.14999999999998792, 2.500000000000000000, -1.472243186433547901 ) ) ;
#79435 = DIRECTION ( 'NONE',  ( -0.000000000000000000, -1.000000000000000000, -0.000000000000000000 ) ) ;
#79436 = CIRCLE ( 'NONE', #89782, 0.06509327318403741736 ) ;
#79437 = CARTESIAN_POINT ( 'NONE',  ( 7.499999999999925393, 12.50000000000000000, -3.572213422710612374 ) ) ;
#79438 = FACE_OUTER_BOUND ( 'NONE', #55895, .T. ) ;
#79439 = VERTEX_POINT ( 'NONE', #76016 ) ;
#79440 = FACE_OUTER_BOUND ( 'NONE', #84983, .T. ) ;
#79441 = EDGE_LOOP ( 'NONE', ( #7063, #11349, #29293, #17017 ) ) ;
#79442 = ORIENTED_EDGE ( 'NONE', *, *, #123260, .T. ) ;
#79443 = ORIENTED_EDGE ( 'NONE', *, *, #10165, .F. ) ;
#79444 = DIRECTION ( 'NONE',  ( 0.000000000000000000, -0.000000000000000000, 1.000000000000000000 ) ) ;
#79445 = EDGE_CURVE ( 'NONE', #101675, #20773, #105158, .T. ) ;
#79446 = EDGE_LOOP ( 'NONE', ( #86882, #23949 ) ) ;
#79447 = ORIENTED_EDGE ( 'NONE', *, *, #27416, .T. ) ;
#79448 = DIRECTION ( 'NONE',  ( -0.000000000000000000, -1.000000000000000000, -0.000000000000000000 ) ) ;
#79449 = DIRECTION ( 'NONE',  ( 0.000000000000000000, 0.000000000000000000, 1.000000000000000000 ) ) ;
#79450 = CARTESIAN_POINT ( 'NONE',  ( 13.09999999999990195, 2.500000000000000000, -3.883716857408426648 ) ) ;
#79451 = DIRECTION ( 'NONE',  ( 0.000000000000000000, 0.000000000000000000, 1.000000000000000000 ) ) ;
#79452 = EDGE_CURVE ( 'NONE', #75136, #12415, #71719, .T. ) ;
#79453 = CIRCLE ( 'NONE', #41811, 0.1000000000000000472 ) ;
#79454 = VERTEX_POINT ( 'NONE', #45282 ) ;
#79455 = ADVANCED_FACE ( 'NONE', ( #95660 ), #85192, .T. ) ;
#79456 = CARTESIAN_POINT ( 'NONE',  ( 11.24999999999990763, 12.50000000000000000, 1.407149913249508000 ) ) ;
#79457 = ORIENTED_EDGE ( 'NONE', *, *, #114599, .T. ) ;
#79459 = ADVANCED_FACE ( 'NONE', ( #6591 ), #45930, .T. ) ;
#79458 = CARTESIAN_POINT ( 'NONE',  ( 8.099999999999923261, 2.500000000000000000, -3.983716857408426293 ) ) ;
#79460 = AXIS2_PLACEMENT_3D ( 'NONE', #67052, #106989, #7507 ) ;
#79461 = VERTEX_POINT ( 'NONE', #115939 ) ;
#79462 = DIRECTION ( 'NONE',  ( 0.000000000000000000, 0.000000000000000000, -1.000000000000000000 ) ) ;
#79463 = DIRECTION ( 'NONE',  ( 0.000000000000000000, 0.000000000000000000, 1.000000000000000000 ) ) ;
#79464 = ORIENTED_EDGE ( 'NONE', *, *, #53214, .F. ) ;
#79465 = CARTESIAN_POINT ( 'NONE',  ( -0.6000000000000388356, 12.50000000000000000, 4.611443907251934426 ) ) ;
#79466 = EDGE_CURVE ( 'NONE', #81575, #46684, #37395, .T. ) ;
#79467 = DIRECTION ( 'NONE',  ( 0.000000000000000000, 0.000000000000000000, 1.000000000000000000 ) ) ;
#79468 = VERTEX_POINT ( 'NONE', #106123 ) ;
#79469 = EDGE_CURVE ( 'NONE', #62361, #2581, #76668, .T. ) ;
#79471 = CIRCLE ( 'NONE', #114942, 0.06509327318403745899 ) ;
#79470 = CIRCLE ( 'NONE', #66915, 0.09999999999999982514 ) ;
#79472 = EDGE_CURVE ( 'NONE', #113011, #104247, #38281, .T. ) ;
#79473 = EDGE_CURVE ( 'NONE', #26951, #76450, #59222, .T. ) ;
#79474 = DIRECTION ( 'NONE',  ( 0.000000000000000000, 0.000000000000000000, -1.000000000000000000 ) ) ;
#79475 = EDGE_LOOP ( 'NONE', ( #30331, #73440, #97752, #18553 ) ) ;
#79476 = ORIENTED_EDGE ( 'NONE', *, *, #58817, .F. ) ;
#79477 = DIRECTION ( 'NONE',  ( -0.000000000000000000, -1.000000000000000000, -0.000000000000000000 ) ) ;
#79478 = FACE_OUTER_BOUND ( 'NONE', #40398, .T. ) ;
#79479 = CARTESIAN_POINT ( 'NONE',  ( 184.1302083336747160, -4.367472073101514418, -7.564683531250002702 ) ) ;
#79480 = DIRECTION ( 'NONE',  ( 0.000000000000000000, 0.000000000000000000, -1.000000000000000000 ) ) ;
#79481 = EDGE_CURVE ( 'NONE', #10025, #45696, #17307, .T. ) ;
#79482 = CARTESIAN_POINT ( 'NONE',  ( -10.20000000000000462, 12.50000000000000000, 4.676537180435972552 ) ) ;
#79483 = ORIENTED_EDGE ( 'NONE', *, *, #5238, .F. ) ;
#79484 = CARTESIAN_POINT ( 'NONE',  ( 184.1145833340161175, 6.668395609140177704, -3.849999999999998312 ) ) ;
#79485 = ORIENTED_EDGE ( 'NONE', *, *, #85932, .T. ) ;
#79486 = CARTESIAN_POINT ( 'NONE',  ( -10.00000000000000355, 2.500000000000000000, -0.6928203230275541413 ) ) ;
#79487 = CIRCLE ( 'NONE', #64873, 0.09999999999999982514 ) ;
#79488 = CARTESIAN_POINT ( 'NONE',  ( 14.14999999999989555, 12.50000000000000000, 2.165063509461097713 ) ) ;
#79489 = VECTOR ( 'NONE', #83436, 1000.000000000000000 ) ;
#79490 = DIRECTION ( 'NONE',  ( -0.000000000000000000, 1.000000000000000000, -0.000000000000000000 ) ) ;
#79491 = DIRECTION ( 'NONE',  ( -0.000000000000000000, -1.000000000000000000, -0.000000000000000000 ) ) ;
#79492 = DIRECTION ( 'NONE',  ( 0.000000000000000000, 1.000000000000000000, 0.000000000000000000 ) ) ;
#79493 = CARTESIAN_POINT ( 'NONE',  ( -9.800000000000007816, 12.50000000000000000, -4.048810130592459089 ) ) ;
#79494 = DIRECTION ( 'NONE',  ( 0.000000000000000000, 0.000000000000000000, 1.000000000000000000 ) ) ;
#79495 = ORIENTED_EDGE ( 'NONE', *, *, #106467, .T. ) ;
#79496 = AXIS2_PLACEMENT_3D ( 'NONE', #30091, #102038, #122332 ) ;
#79497 = DIRECTION ( 'NONE',  ( 0.000000000000000000, 0.000000000000000000, 1.000000000000000000 ) ) ;
#79498 = CARTESIAN_POINT ( 'NONE',  ( 0.4499999999999573785, 2.500000000000000000, -6.495190528383302464 ) ) ;
#79499 = AXIS2_PLACEMENT_3D ( 'NONE', #10310, #66155, #39791 ) ;
#79500 = ORIENTED_EDGE ( 'NONE', *, *, #7734, .F. ) ;
#79501 = CARTESIAN_POINT ( 'NONE',  ( -0.4500000000000402012, 2.500000000000000000, 2.265063509461097357 ) ) ;
#79502 = AXIS2_PLACEMENT_3D ( 'NONE', #20405, #50496, #49880 ) ;
#79503 = AXIS2_PLACEMENT_3D ( 'NONE', #124266, #34616, #16213 ) ;
#79504 = EDGE_CURVE ( 'NONE', #18510, #79117, #48748, .T. ) ;
#79505 = EDGE_LOOP ( 'NONE', ( #22875, #119578, #28383, #79965 ) ) ;
#79506 = VERTEX_POINT ( 'NONE', #49798 ) ;
#79507 = DIRECTION ( 'NONE',  ( 0.000000000000000000, -0.000000000000000000, 1.000000000000000000 ) ) ;
#79508 = EDGE_LOOP ( 'NONE', ( #105326, #94530 ) ) ;
#79509 = CARTESIAN_POINT ( 'NONE',  ( -0.2000000000000339284, 2.500000000000000000, -0.3464101615137759604 ) ) ;
#79510 = DIRECTION ( 'NONE',  ( -0.000000000000000000, 1.000000000000000000, -0.000000000000000000 ) ) ;
#79511 = CIRCLE ( 'NONE', #16777, 0.09999999999999999167 ) ;
#79512 = ORIENTED_EDGE ( 'NONE', *, *, #96396, .F. ) ;
#79513 = PLANE ( 'NONE',  #126102 ) ;
#79515 = EDGE_LOOP ( 'NONE', ( #104559, #29759 ) ) ;
#79514 = DIRECTION ( 'NONE',  ( 0.000000000000000000, 0.000000000000000000, 1.000000000000000000 ) ) ;
#79516 = CONICAL_SURFACE ( 'NONE', #123330, 0.09999999999999999167, 0.003490658503988666988 ) ;
#79517 = DIRECTION ( 'NONE',  ( -0.000000000000000000, 1.000000000000000000, -0.000000000000000000 ) ) ;
#79518 = EDGE_CURVE ( 'NONE', #16084, #64702, #2757, .T. ) ;
#79519 = ORIENTED_EDGE ( 'NONE', *, *, #43829, .F. ) ;
#79520 = ORIENTED_EDGE ( 'NONE', *, *, #114551, .T. ) ;
#79521 = ORIENTED_EDGE ( 'NONE', *, *, #7006, .T. ) ;
#79522 = LINE ( 'NONE', #61165, #39980 ) ;
#79523 = CARTESIAN_POINT ( 'NONE',  ( 7.899999999999924860, 2.500000000000000000, -3.537306695894649966 ) ) ;
#79524 = CARTESIAN_POINT ( 'NONE',  ( -14.14999999999998614, 2.500000000000000000, 1.372243186433549367 ) ) ;
#79525 = FACE_BOUND ( 'NONE', #3834, .T. ) ;
#79526 = EDGE_LOOP ( 'NONE', ( #45535, #44241 ) ) ;
#79527 = DIRECTION ( 'NONE',  ( -0.000000000000000000, 1.000000000000000000, -0.000000000000000000 ) ) ;
#79528 = DIRECTION ( 'NONE',  ( 0.000000000000000000, -0.9999939076577903929, 0.003490651415223739937 ) ) ;
#79529 = ORIENTED_EDGE ( 'NONE', *, *, #116388, .T. ) ;
#79530 = CARTESIAN_POINT ( 'NONE',  ( -2.300000000000033129, 2.500000000000000000, 3.983716857408420076 ) ) ;
#79531 = DIRECTION ( 'NONE',  ( -0.000000000000000000, -1.000000000000000000, -0.000000000000000000 ) ) ;
#79533 = DIRECTION ( 'NONE',  ( -0.000000000000000000, -1.000000000000000000, -0.000000000000000000 ) ) ;
#79532 = VECTOR ( 'NONE', #99247, 1000.000000000000000 ) ;
#79534 = CARTESIAN_POINT ( 'NONE',  ( -14.59999999999998366, 12.50000000000000000, 0.6928203230275518099 ) ) ;
#79535 = CARTESIAN_POINT ( 'NONE',  ( -0.8000000000000381251, 2.500000000000000000, 4.430127018922196847 ) ) ;
#79536 = CONICAL_SURFACE ( 'NONE', #54385, 0.1000000000000002554, 0.003490658503988666988 ) ;
#79537 = DIRECTION ( 'NONE',  ( -0.000000000000000000, -1.000000000000000000, -0.000000000000000000 ) ) ;
#79538 = DIRECTION ( 'NONE',  ( 0.000000000000000000, 0.000000000000000000, -1.000000000000000000 ) ) ;
#79539 = EDGE_CURVE ( 'NONE', #36792, #28566, #107220, .T. ) ;
#79540 = CONICAL_SURFACE ( 'NONE', #41896, 0.09999999999999982514, 0.003490658503988666988 ) ;
#79541 = VERTEX_POINT ( 'NONE', #10485 ) ;
#79542 = ORIENTED_EDGE ( 'NONE', *, *, #126095, .F. ) ;
#79543 = ORIENTED_EDGE ( 'NONE', *, *, #2182, .T. ) ;
#79544 = ORIENTED_EDGE ( 'NONE', *, *, #54408, .T. ) ;
#79545 = ORIENTED_EDGE ( 'NONE', *, *, #98371, .F. ) ;
#79546 = DIRECTION ( 'NONE',  ( -0.000000000000000000, -1.000000000000000000, -0.000000000000000000 ) ) ;
#79547 = PLANE ( 'NONE',  #94814 ) ;
#79548 = VERTEX_POINT ( 'NONE', #69405 ) ;
#79549 = FACE_BOUND ( 'NONE', #114452, .T. ) ;
#79550 = ADVANCED_FACE ( 'NONE', ( #79881 ), #125989, .T. ) ;
#79551 = DIRECTION ( 'NONE',  ( 0.000000000000000000, 0.000000000000000000, 1.000000000000000000 ) ) ;
#79552 = DIRECTION ( 'NONE',  ( -0.000000000000000000, -1.000000000000000000, -0.000000000000000000 ) ) ;
#79553 = DIRECTION ( 'NONE',  ( 0.000000000000000000, 0.000000000000000000, 1.000000000000000000 ) ) ;
#79554 = EDGE_CURVE ( 'NONE', #53683, #58504, #39968, .T. ) ;
#79555 = DIRECTION ( 'NONE',  ( 0.000000000000000000, -0.9999939076577903929, 0.003490651415223739937 ) ) ;
#79556 = EDGE_CURVE ( 'NONE', #23819, #126044, #13113, .T. ) ;
#79557 = DIRECTION ( 'NONE',  ( 0.000000000000000000, 0.000000000000000000, -1.000000000000000000 ) ) ;
#79558 = EDGE_CURVE ( 'NONE', #112102, #11681, #98905, .T. ) ;
#79559 = DIRECTION ( 'NONE',  ( -0.000000000000000000, -1.000000000000000000, -0.000000000000000000 ) ) ;
#79560 = ADVANCED_FACE ( 'NONE', ( #109992 ), #15252, .T. ) ;
#79561 = ORIENTED_EDGE ( 'NONE', *, *, #42842, .F. ) ;
#79562 = EDGE_CURVE ( 'NONE', #21250, #127872, #118511, .T. ) ;
#79563 = ORIENTED_EDGE ( 'NONE', *, *, #121855, .F. ) ;
#79564 = ORIENTED_EDGE ( 'NONE', *, *, #36687, .T. ) ;
#79565 = ORIENTED_EDGE ( 'NONE', *, *, #26434, .T. ) ;
#79566 = ORIENTED_EDGE ( 'NONE', *, *, #63590, .T. ) ;
#79567 = CARTESIAN_POINT ( 'NONE',  ( 15.83209681635554666, 2.500000000000000000, 5.404881881984142211 ) ) ;
#79568 = DIRECTION ( 'NONE',  ( -0.000000000000000000, -1.000000000000000000, -0.000000000000000000 ) ) ;
#79569 = VERTEX_POINT ( 'NONE', #49157 ) ;
#79570 = EDGE_CURVE ( 'NONE', #72840, #120418, #86275, .T. ) ;
#79571 = DIRECTION ( 'NONE',  ( 0.000000000000000000, 1.000000000000000000, 0.000000000000000000 ) ) ;
#79572 = EDGE_CURVE ( 'NONE', #90854, #127558, #119806, .T. ) ;
#79573 = FACE_OUTER_BOUND ( 'NONE', #325, .T. ) ;
#79574 = ADVANCED_FACE ( 'NONE', ( #30804 ), #100955, .T. ) ;
#79575 = DIRECTION ( 'NONE',  ( 0.000000000000000000, 1.000000000000000000, 0.000000000000000000 ) ) ;
#79576 = CARTESIAN_POINT ( 'NONE',  ( 185.2760416670080588, 6.551208109652274736, 3.782341765625001351 ) ) ;
#79577 = CARTESIAN_POINT ( 'NONE',  ( 3.549999999999944755, 2.500000000000000000, -2.611473670974877592 ) ) ;
#79578 = DIRECTION ( 'NONE',  ( 0.000000000000000000, 1.000000000000000000, 0.000000000000000000 ) ) ;
#79579 = DIRECTION ( 'NONE',  ( -0.000000000000000000, 1.000000000000000000, -0.000000000000000000 ) ) ;
#79580 = ORIENTED_EDGE ( 'NONE', *, *, #27273, .T. ) ;
#79581 = DIRECTION ( 'NONE',  ( -0.000000000000000000, 1.000000000000000000, -0.000000000000000000 ) ) ;
#79582 = CIRCLE ( 'NONE', #12657, 0.06509327318403745899 ) ;
#79583 = ORIENTED_EDGE ( 'NONE', *, *, #126850, .T. ) ;
#79584 = ORIENTED_EDGE ( 'NONE', *, *, #112206, .T. ) ;
#79585 = DIRECTION ( 'NONE',  ( 0.000000000000000000, 0.000000000000000000, -1.000000000000000000 ) ) ;
#79586 = DIRECTION ( 'NONE',  ( 0.000000000000000000, -0.9999939076577903929, 0.003490651415223739937 ) ) ;
#79587 = CARTESIAN_POINT ( 'NONE',  ( 1.249999999999953815, 2.500000000000000000, -2.857883832488653741 ) ) ;
#79588 = ORIENTED_EDGE ( 'NONE', *, *, #79845, .F. ) ;
#79589 = ORIENTED_EDGE ( 'NONE', *, *, #111682, .F. ) ;
#79590 = CARTESIAN_POINT ( 'NONE',  ( 184.9479166673494603, -6.668395609140176816, -3.850000000000003642 ) ) ;
#79591 = CIRCLE ( 'NONE', #75464, 0.06509327318403745899 ) ;
#79592 = LINE ( 'NONE', #98555, #43237 ) ;
#79593 = FACE_OUTER_BOUND ( 'NONE', #83183, .T. ) ;
#79594 = DIRECTION ( 'NONE',  ( 0.000000000000000000, 1.000000000000000000, 0.000000000000000000 ) ) ;
#79595 = EDGE_LOOP ( 'NONE', ( #109028, #79837 ) ) ;
#79596 = DIRECTION ( 'NONE',  ( 0.000000000000000000, 0.000000000000000000, -1.000000000000000000 ) ) ;
#79597 = AXIS2_PLACEMENT_3D ( 'NONE', #16215, #56152, #6383 ) ;
#79598 = VERTEX_POINT ( 'NONE', #39344 ) ;
#79599 = DIRECTION ( 'NONE',  ( 0.000000000000000000, -0.9999939076577903929, 0.003490651415223739937 ) ) ;
#79600 = EDGE_LOOP ( 'NONE', ( #15077, #79521, #111724, #92499 ) ) ;
#79601 = CARTESIAN_POINT ( 'NONE',  ( -7.050000000000016698, 12.50000000000000000, -2.165063509461101710 ) ) ;
#79602 = DIRECTION ( 'NONE',  ( 0.000000000000000000, -0.000000000000000000, 1.000000000000000000 ) ) ;
#79603 = AXIS2_PLACEMENT_3D ( 'NONE', #92909, #57317, #125409 ) ;
#79604 = DIRECTION ( 'NONE',  ( 0.000000000000000000, 0.000000000000000000, -1.000000000000000000 ) ) ;
#79605 = EDGE_CURVE ( 'NONE', #113972, #51049, #670, .T. ) ;
#79606 = DIRECTION ( 'NONE',  ( -0.000000000000000000, 1.000000000000000000, -0.000000000000000000 ) ) ;
#79607 = VERTEX_POINT ( 'NONE', #40632 ) ;
#79608 = ADVANCED_FACE ( 'NONE', ( #70706 ), #82189, .T. ) ;
#79609 = DIRECTION ( 'NONE',  ( -0.000000000000000000, 1.000000000000000000, -0.000000000000000000 ) ) ;
#79610 = EDGE_CURVE ( 'NONE', #63429, #5496, #9010, .T. ) ;
#79611 = ORIENTED_EDGE ( 'NONE', *, *, #8320, .T. ) ;
#79612 = ORIENTED_EDGE ( 'NONE', *, *, #43362, .F. ) ;
#79613 = CARTESIAN_POINT ( 'NONE',  ( 14.14999999999989733, 12.50000000000000000, 1.472243186433545459 ) ) ;
#79614 = CARTESIAN_POINT ( 'NONE',  ( 7.949999999999925571, 2.500000000000000000, 2.265063509461097357 ) ) ;
#79615 = FACE_OUTER_BOUND ( 'NONE', #3327, .T. ) ;
#79616 = DIRECTION ( 'NONE',  ( -0.000000000000000000, 1.000000000000000000, -0.000000000000000000 ) ) ;
#79617 = EDGE_CURVE ( 'NONE', #48600, #77665, #36332, .T. ) ;
#79618 = CARTESIAN_POINT ( 'NONE',  ( 2.899999999999944844, 2.500000000000000000, 5.022947341949748790 ) ) ;
#79619 = CARTESIAN_POINT ( 'NONE',  ( 5.449999999999937117, 2.500000000000000000, -6.495190528383302464 ) ) ;
#79620 = FACE_OUTER_BOUND ( 'NONE', #43524, .T. ) ;
#79621 = DIRECTION ( 'NONE',  ( 0.000000000000000000, 0.000000000000000000, 1.000000000000000000 ) ) ;
#79622 = AXIS2_PLACEMENT_3D ( 'NONE', #3608, #125945, #105682 ) ;
#79623 = CIRCLE ( 'NONE', #90071, 0.1000000000000002554 ) ;
#79624 = VECTOR ( 'NONE', #52703, 1000.000000000000000 ) ;
#79625 = VECTOR ( 'NONE', #121182, 1000.000000000000000 ) ;
#79626 = ORIENTED_EDGE ( 'NONE', *, *, #58600, .F. ) ;
#79627 = LINE ( 'NONE', #50820, #14973 ) ;
#79628 = DIRECTION ( 'NONE',  ( 0.000000000000000000, 0.000000000000000000, 1.000000000000000000 ) ) ;
#79629 = DIRECTION ( 'NONE',  ( 0.000000000000000000, 0.000000000000000000, -1.000000000000000000 ) ) ;
#79630 = EDGE_CURVE ( 'NONE', #55154, #26833, #72008, .T. ) ;
#79631 = DIRECTION ( 'NONE',  ( 0.000000000000000000, 1.000000000000000000, 0.000000000000000000 ) ) ;
#79632 = CARTESIAN_POINT ( 'NONE',  ( -2.950000000000030376, 2.500000000000000000, 6.395190528383296602 ) ) ;
#79633 = VERTEX_POINT ( 'NONE', #101461 ) ;
#79634 = DIRECTION ( 'NONE',  ( 0.000000000000000000, 0.000000000000000000, -1.000000000000000000 ) ) ;
#79635 = DIRECTION ( 'NONE',  ( -4.274815082592931898E-19, -0.9999939076577903929, -0.003490651415223739937 ) ) ;
#79637 = EDGE_LOOP ( 'NONE', ( #84492, #8456, #17370, #41965 ) ) ;
#79636 = DIRECTION ( 'NONE',  ( 0.000000000000000000, 0.000000000000000000, 1.000000000000000000 ) ) ;
#79638 = ORIENTED_EDGE ( 'NONE', *, *, #78576, .F. ) ;
#79639 = CARTESIAN_POINT ( 'NONE',  ( -5.650000000000019895, 2.500000000000000000, 6.148780366869520009 ) ) ;
#79640 = VECTOR ( 'NONE', #114492, 1000.000000000000000 ) ;
#79642 = VERTEX_POINT ( 'NONE', #82476 ) ;
#79641 = EDGE_CURVE ( 'NONE', #91540, #1964, #2855, .T. ) ;
#79643 = VERTEX_POINT ( 'NONE', #105150 ) ;
#79644 = ORIENTED_EDGE ( 'NONE', *, *, #92897, .T. ) ;
#79645 = CARTESIAN_POINT ( 'NONE',  ( -4.800000000000024691, 2.500000000000000000, 4.776537180435972196 ) ) ;
#79646 = DIRECTION ( 'NONE',  ( -0.000000000000000000, 1.000000000000000000, -0.000000000000000000 ) ) ;
#79647 = DIRECTION ( 'NONE',  ( 0.000000000000000000, 0.000000000000000000, 1.000000000000000000 ) ) ;
#79648 = CARTESIAN_POINT ( 'NONE',  ( 7.499999999999923617, 2.500000000000000000, 0.6928203230275494784 ) ) ;
#79649 = AXIS2_PLACEMENT_3D ( 'NONE', #54984, #113263, #54343 ) ;
#79650 = VERTEX_POINT ( 'NONE', #114964 ) ;
#79651 = CIRCLE ( 'NONE', #77677, 0.06509327318403745899 ) ;
#79653 = CARTESIAN_POINT ( 'NONE',  ( 14.79999999999989235, 2.500000000000000000, 0.3464101615137735735 ) ) ;
#79652 = B_SPLINE_CURVE_WITH_KNOTS ( 'NONE', 3,
 ( #117346, #85970, #67625, #8068 ),
 .UNSPECIFIED., .F., .F.,
 ( 4, 4 ),
 ( 0.0001556283592076939662, 0.002283789722394891780 ),
 .UNSPECIFIED. ) ;
#79654 = ORIENTED_EDGE ( 'NONE', *, *, #189, .F. ) ;
#79655 = DIRECTION ( 'NONE',  ( 0.000000000000000000, 1.000000000000000000, 0.000000000000000000 ) ) ;
#79656 = CARTESIAN_POINT ( 'NONE',  ( 18.78720903128151321, 2.539625591034162078, 4.564429507519030871 ) ) ;
#79657 = DIRECTION ( 'NONE',  ( -0.000000000000000000, -1.000000000000000000, -0.000000000000000000 ) ) ;
#79658 = EDGE_CURVE ( 'NONE', #24306, #34557, #78067, .T. ) ;
#79659 = CARTESIAN_POINT ( 'NONE',  ( 12.09999999999990550, 2.500000000000000000, 4.330127018922196314 ) ) ;
#79660 = VECTOR ( 'NONE', #99736, 1000.000000000000000 ) ;
#79661 = ORIENTED_EDGE ( 'NONE', *, *, #96861, .F. ) ;
#79662 = CIRCLE ( 'NONE', #19007, 0.1000000000000002554 ) ;
#79663 = VERTEX_POINT ( 'NONE', #5653 ) ;
#79664 = ORIENTED_EDGE ( 'NONE', *, *, #93171, .T. ) ;
#79665 = EDGE_LOOP ( 'NONE', ( #44119, #9352 ) ) ;
#79666 = VERTEX_POINT ( 'NONE', #2590 ) ;
#79667 = DIRECTION ( 'NONE',  ( -0.000000000000000000, 1.000000000000000000, -0.000000000000000000 ) ) ;
#79668 = CARTESIAN_POINT ( 'NONE',  ( -5.650000000000023448, 2.500000000000000000, -6.048780366869526581 ) ) ;
#79669 = EDGE_CURVE ( 'NONE', #41193, #64688, #81803, .T. ) ;
#79670 = FACE_OUTER_BOUND ( 'NONE', #90620, .T. ) ;
#79671 = FACE_BOUND ( 'NONE', #75373, .T. ) ;
#79672 = DIRECTION ( 'NONE',  ( 0.000000000000000000, -0.9999939076577903929, 0.003490651415223739937 ) ) ;
#79673 = CARTESIAN_POINT ( 'NONE',  ( 179.5000000000000000, -1.375000000000002442, 6.000000000000000000 ) ) ;
#79674 = DIRECTION ( 'NONE',  ( 0.000000000000000000, 1.000000000000000000, 0.000000000000000000 ) ) ;
#79675 = CONICAL_SURFACE ( 'NONE', #81812, 0.09999999999999982514, 0.003490658503988666988 ) ;
#79676 = AXIS2_PLACEMENT_3D ( 'NONE', #57951, #129289, #46845 ) ;
#79677 = PLANE ( 'NONE',  #17158 ) ;
#79678 = DIRECTION ( 'NONE',  ( 0.000000000000000000, 0.000000000000000000, 1.000000000000000000 ) ) ;
#79679 = CARTESIAN_POINT ( 'NONE',  ( 11.89999999999990798, 12.50000000000000000, 3.983716857408420964 ) ) ;
#79680 = CIRCLE ( 'NONE', #25377, 0.06509327318403745899 ) ;
#79681 = CARTESIAN_POINT ( 'NONE',  ( -8.750000000000010658, 12.50000000000000000, -1.472243186433550122 ) ) ;
#79682 = ADVANCED_FACE ( 'NONE', ( #44965 ), #92266, .T. ) ;
#79683 = ORIENTED_EDGE ( 'NONE', *, *, #2530, .F. ) ;
#79684 = AXIS2_PLACEMENT_3D ( 'NONE', #57966, #40263, #30456 ) ;
#79685 = ORIENTED_EDGE ( 'NONE', *, *, #39223, .F. ) ;
#79686 = EDGE_LOOP ( 'NONE', ( #124654, #41345 ) ) ;
#79687 = ORIENTED_EDGE ( 'NONE', *, *, #7339, .T. ) ;
#79688 = DIRECTION ( 'NONE',  ( 0.000000000000000000, 0.000000000000000000, 1.000000000000000000 ) ) ;
#79689 = CARTESIAN_POINT ( 'NONE',  ( 5.799999999999933209, 12.50000000000000000, 0.06509327318403504425 ) ) ;
#79690 = FACE_BOUND ( 'NONE', #73325, .T. ) ;
#79691 = DIRECTION ( 'NONE',  ( 0.000000000000000000, 0.000000000000000000, 1.000000000000000000 ) ) ;
#79692 = EDGE_CURVE ( 'NONE', #24253, #44219, #32125, .T. ) ;
#79693 = VERTEX_POINT ( 'NONE', #105810 ) ;
#79694 = ADVANCED_FACE ( 'NONE', ( #115611 ), #19583, .T. ) ;
#79695 = LINE ( 'NONE', #99353, #50941 ) ;
#79696 = CARTESIAN_POINT ( 'NONE',  ( -9.400000000000007461, 2.500000000000000000, 4.676537180435972552 ) ) ;
#79697 = EDGE_CURVE ( 'NONE', #60583, #19106, #117756, .T. ) ;
#79698 = CARTESIAN_POINT ( 'NONE',  ( 10.39999999999991509, 2.500000000000000000, 0.6928203230275494784 ) ) ;
#79699 = EDGE_CURVE ( 'NONE', #87317, #107669, #96839, .T. ) ;
#79700 = CARTESIAN_POINT ( 'NONE',  ( 11.24999999999990585, 2.500000000000000000, -5.802370205355749988 ) ) ;
#79701 = ADVANCED_FACE ( 'NONE', ( #56047 ), #95347, .T. ) ;
#79702 = VERTEX_POINT ( 'NONE', #25291 ) ;
#79703 = LINE ( 'NONE', #29976, #76395 ) ;
#79704 = ORIENTED_EDGE ( 'NONE', *, *, #113737, .F. ) ;
#79705 = ADVANCED_FACE ( 'NONE', ( #22273 ), #103111, .T. ) ;
#79706 = AXIS2_PLACEMENT_3D ( 'NONE', #36643, #66070, #54963 ) ;
#79707 = EDGE_LOOP ( 'NONE', ( #110565, #36977 ) ) ;
#79708 = CIRCLE ( 'NONE', #37949, 0.06509327318403745899 ) ;
#79709 = DIRECTION ( 'NONE',  ( 0.000000000000000000, 1.000000000000000000, 0.000000000000000000 ) ) ;
#79710 = AXIS2_PLACEMENT_3D ( 'NONE', #36309, #97788, #76865 ) ;
#79711 = EDGE_CURVE ( 'NONE', #102673, #120910, #113583, .T. ) ;
#79712 = CARTESIAN_POINT ( 'NONE',  ( 3.549999999999943867, 12.50000000000000000, -1.818653347947326138 ) ) ;
#79713 = ORIENTED_EDGE ( 'NONE', *, *, #59194, .F. ) ;
#79714 = EDGE_CURVE ( 'NONE', #9888, #41869, #701, .T. ) ;
#79715 = EDGE_CURVE ( 'NONE', #39357, #77678, #9113, .T. ) ;
#79716 = FACE_OUTER_BOUND ( 'NONE', #69758, .T. ) ;
#79718 = EDGE_CURVE ( 'NONE', #92091, #29934, #111247, .T. ) ;
#79717 = AXIS2_PLACEMENT_3D ( 'NONE', #53093, #123737, #14430 ) ;
#79719 = DIRECTION ( 'NONE',  ( -0.000000000000000000, -1.000000000000000000, -0.000000000000000000 ) ) ;
#79720 = VERTEX_POINT ( 'NONE', #94689 ) ;
#79721 = DIRECTION ( 'NONE',  ( -0.000000000000000000, 1.000000000000000000, -0.000000000000000000 ) ) ;
#79722 = VERTEX_POINT ( 'NONE', #86140 ) ;
#79723 = CIRCLE ( 'NONE', #8595, 0.06509327318403745899 ) ;
#79724 = DIRECTION ( 'NONE',  ( 0.000000000000000000, 0.000000000000000000, 1.000000000000000000 ) ) ;
#79725 = EDGE_CURVE ( 'NONE', #11513, #36138, #38385, .T. ) ;
#79726 = VERTEX_POINT ( 'NONE', #106449 ) ;
#79727 = CARTESIAN_POINT ( 'NONE',  ( 13.74999999999993427, 12.50000000000000000, 2.165063509461097713 ) ) ;
#79728 = FACE_BOUND ( 'NONE', #113547, .T. ) ;
#79729 = VERTEX_POINT ( 'NONE', #108382 ) ;
#79730 = LINE ( 'NONE', #67294, #1589 ) ;
#79731 = VERTEX_POINT ( 'NONE', #37718 ) ;
#79732 = DIRECTION ( 'NONE',  ( -0.000000000000000000, 1.000000000000000000, -0.000000000000000000 ) ) ;
#79733 = DIRECTION ( 'NONE',  ( 0.000000000000000000, -0.9999939076577903929, 0.003490651415223739937 ) ) ;
#79734 = DIRECTION ( 'NONE',  ( -0.000000000000000000, -1.000000000000000000, -0.000000000000000000 ) ) ;
#79735 = CARTESIAN_POINT ( 'NONE',  ( 2.299999999999948752, 12.50000000000000000, -3.983716857408426293 ) ) ;
#79736 = DIRECTION ( 'NONE',  ( 0.000000000000000000, 1.000000000000000000, 0.000000000000000000 ) ) ;
#79737 = ORIENTED_EDGE ( 'NONE', *, *, #79711, .F. ) ;
#79738 = VERTEX_POINT ( 'NONE', #98542 ) ;
#79739 = VERTEX_POINT ( 'NONE', #7598 ) ;
#79740 = DIRECTION ( 'NONE',  ( -0.000000000000000000, 1.000000000000000000, -0.000000000000000000 ) ) ;
#79741 = CARTESIAN_POINT ( 'NONE',  ( 14.39999999999989555, 12.50000000000000000, 0.3464101615137736845 ) ) ;
#79742 = DIRECTION ( 'NONE',  ( -4.274815082592931898E-19, -0.9999939076577903929, -0.003490651415223739937 ) ) ;
#79744 = ORIENTED_EDGE ( 'NONE', *, *, #7568, .T. ) ;
#79743 = ORIENTED_EDGE ( 'NONE', *, *, #93980, .T. ) ;
#79745 = ORIENTED_EDGE ( 'NONE', *, *, #30810, .F. ) ;
#79746 = CARTESIAN_POINT ( 'NONE',  ( 12.49999999999990585, 12.50000000000000000, 3.637306695894644726 ) ) ;
#79748 = EDGE_LOOP ( 'NONE', ( #1143, #41263 ) ) ;
#79747 = CIRCLE ( 'NONE', #90190, 0.09999999999999982514 ) ;
#79749 = DIRECTION ( 'NONE',  ( 0.000000000000000000, 1.000000000000000000, 0.000000000000000000 ) ) ;
#79750 = AXIS2_PLACEMENT_3D ( 'NONE', #56565, #76233, #6173 ) ;
#79751 = CARTESIAN_POINT ( 'NONE',  ( -3.950000000000024603, 2.500000000000000000, -2.611473670974877592 ) ) ;
#79752 = DIRECTION ( 'NONE',  ( 0.000000000000000000, 1.000000000000000000, 0.000000000000000000 ) ) ;
#79753 = CARTESIAN_POINT ( 'NONE',  ( -0.4000000000000331624, 2.500000000000000000, 0.000000000000000000 ) ) ;
#79754 = CARTESIAN_POINT ( 'NONE',  ( 6.649999999999931966, 2.500000000000000000, -5.902370205355750521 ) ) ;
#79755 = CARTESIAN_POINT ( 'NONE',  ( 12.49999999999993605, 12.50000000000000000, -0.06509327318403970719 ) ) ;
#79757 = AXIS2_PLACEMENT_3D ( 'NONE', #118443, #102043, #71277 ) ;
#79756 = DIRECTION ( 'NONE',  ( 0.000000000000000000, 1.000000000000000000, 0.000000000000000000 ) ) ;
#79758 = VERTEX_POINT ( 'NONE', #47541 ) ;
#79759 = AXIS2_PLACEMENT_3D ( 'NONE', #6476, #27432, #115823 ) ;
#79760 = ORIENTED_EDGE ( 'NONE', *, *, #1476, .T. ) ;
#79761 = EDGE_CURVE ( 'NONE', #119463, #98563, #59319, .T. ) ;
#79762 = DIRECTION ( 'NONE',  ( 0.000000000000000000, 1.000000000000000000, 0.000000000000000000 ) ) ;
#79763 = EDGE_CURVE ( 'NONE', #84351, #76546, #77623, .T. ) ;
#79764 = ORIENTED_EDGE ( 'NONE', *, *, #11403, .F. ) ;
#79765 = ORIENTED_EDGE ( 'NONE', *, *, #20288, .T. ) ;
#79766 = CARTESIAN_POINT ( 'NONE',  ( 185.7343750003414016, 8.734944146203032389, 5.348610694689227483E-16 ) ) ;
#79767 = DIRECTION ( 'NONE',  ( -4.274815082592931898E-19, -0.9999939076577903929, -0.003490651415223739937 ) ) ;
#79768 = LINE ( 'NONE', #81070, #26953 ) ;
#79769 = CONICAL_SURFACE ( 'NONE', #327, 0.09999999999999999167, 0.003490658503988666988 ) ;
#79770 = ADVANCED_FACE ( 'NONE', ( #18060 ), #37080, .T. ) ;
#79771 = DIRECTION ( 'NONE',  ( -0.000000000000000000, -1.000000000000000000, -0.000000000000000000 ) ) ;
#79772 = AXIS2_PLACEMENT_3D ( 'NONE', #115804, #26147, #94231 ) ;
#79773 = AXIS2_PLACEMENT_3D ( 'NONE', #103011, #63093, #65004 ) ;
#79774 = CARTESIAN_POINT ( 'NONE',  ( -2.950000000000029932, 12.50000000000000000, 2.099970236277060032 ) ) ;
#79775 = DIRECTION ( 'NONE',  ( 0.000000000000000000, 0.000000000000000000, 1.000000000000000000 ) ) ;
#79776 = AXIS2_PLACEMENT_3D ( 'NONE', #122787, #52124, #33134 ) ;
#79777 = DIRECTION ( 'NONE',  ( 0.000000000000000000, 1.000000000000000000, 0.000000000000000000 ) ) ;
#79778 = AXIS2_PLACEMENT_3D ( 'NONE', #31711, #12686, #60548 ) ;
#79779 = CARTESIAN_POINT ( 'NONE',  ( 12.09999999999990195, 2.500000000000000000, -2.276824562219559311E-15 ) ) ;
#79780 = ORIENTED_EDGE ( 'NONE', *, *, #83449, .T. ) ;
#79781 = AXIS2_PLACEMENT_3D ( 'NONE', #121873, #83254, #72143 ) ;
#79782 = CONICAL_SURFACE ( 'NONE', #73511, 0.09999999999999982514, 0.003490658503988666988 ) ;
#79783 = ORIENTED_EDGE ( 'NONE', *, *, #30562, .T. ) ;
#79784 = ORIENTED_EDGE ( 'NONE', *, *, #13126, .T. ) ;
#79785 = ORIENTED_EDGE ( 'NONE', *, *, #46005, .F. ) ;
#79786 = CARTESIAN_POINT ( 'NONE',  ( 5.199999999999935341, 2.500000000000000000, -0.4464101615137783252 ) ) ;
#79787 = DIRECTION ( 'NONE',  ( 0.000000000000000000, 0.000000000000000000, 1.000000000000000000 ) ) ;
#79788 = ORIENTED_EDGE ( 'NONE', *, *, #6555, .F. ) ;
#79789 = DIRECTION ( 'NONE',  ( -0.000000000000000000, 1.000000000000000000, -0.000000000000000000 ) ) ;
#79790 = CARTESIAN_POINT ( 'NONE',  ( 3.749999999999978684, 12.50000000000000000, -6.560283801567339701 ) ) ;
#79791 = CARTESIAN_POINT ( 'NONE',  ( 10.84999999999991260, 2.500000000000000000, 6.495190528383297135 ) ) ;
#79793 = ORIENTED_EDGE ( 'NONE', *, *, #44260, .T. ) ;
#79792 = CARTESIAN_POINT ( 'NONE',  ( -5.000000000000022204, 2.500000000000000000, 3.537306695894645081 ) ) ;
#79794 = DIRECTION ( 'NONE',  ( 0.000000000000000000, 0.000000000000000000, 1.000000000000000000 ) ) ;
#79795 = DIRECTION ( 'NONE',  ( 0.000000000000000000, -0.9999939076577903929, 0.003490651415223739937 ) ) ;
#79796 = ADVANCED_FACE ( 'NONE', ( #49489 ), #44624, .T. ) ;
#79797 = EDGE_LOOP ( 'NONE', ( #63349, #49608, #25024, #61805 ) ) ;
#79798 = ORIENTED_EDGE ( 'NONE', *, *, #118086, .F. ) ;
#79799 = ORIENTED_EDGE ( 'NONE', *, *, #15607, .T. ) ;
#79800 = AXIS2_PLACEMENT_3D ( 'NONE', #6535, #28813, #108644 ) ;
#79801 = VERTEX_POINT ( 'NONE', #67811 ) ;
#79802 = DIRECTION ( 'NONE',  ( 0.000000000000000000, -0.9999939076577903929, 0.003490651415223739937 ) ) ;
#79803 = AXIS2_PLACEMENT_3D ( 'NONE', #100372, #110193, #71543 ) ;
#79804 = DIRECTION ( 'NONE',  ( -1.000000000000000000, 0.000000000000000000, 7.228014483236698281E-17 ) ) ;
#79805 = FACE_OUTER_BOUND ( 'NONE', #31950, .T. ) ;
#79806 = VECTOR ( 'NONE', #71946, 1000.000000000000000 ) ;
#79807 = AXIS2_PLACEMENT_3D ( 'NONE', #41606, #30502, #70401 ) ;
#79809 = ORIENTED_EDGE ( 'NONE', *, *, #120201, .T. ) ;
#79808 = EDGE_CURVE ( 'NONE', #88035, #110508, #107741, .T. ) ;
#79810 = DIRECTION ( 'NONE',  ( 0.000000000000000000, 1.000000000000000000, 0.000000000000000000 ) ) ;
#79811 = CARTESIAN_POINT ( 'NONE',  ( 6.849999999999927702, 2.500000000000000000, 2.411473670974873862 ) ) ;
#79812 = AXIS2_PLACEMENT_3D ( 'NONE', #114102, #24434, #103645 ) ;
#79813 = DIRECTION ( 'NONE',  ( -0.000000000000000000, 1.000000000000000000, -0.000000000000000000 ) ) ;
#79814 = CARTESIAN_POINT ( 'NONE',  ( 8.299999999999922551, 2.500000000000000000, 4.330127018922196314 ) ) ;
#79815 = EDGE_CURVE ( 'NONE', #57530, #95831, #105255, .T. ) ;
#79816 = AXIS2_PLACEMENT_3D ( 'NONE', #92743, #3074, #54100 ) ;
#79817 = VERTEX_POINT ( 'NONE', #76992 ) ;
#79818 = CARTESIAN_POINT ( 'NONE',  ( -2.050000000000033129, 2.500000000000000000, 6.495190528383297135 ) ) ;
#79819 = EDGE_LOOP ( 'NONE', ( #53555, #45838 ) ) ;
#79820 = ORIENTED_EDGE ( 'NONE', *, *, #75105, .F. ) ;
#79821 = CARTESIAN_POINT ( 'NONE',  ( -11.05000000000000071, 12.50000000000000000, 6.841600689897072485 ) ) ;
#79822 = ADVANCED_FACE ( 'NONE', ( #17404 ), #58010, .T. ) ;
#79823 = DIRECTION ( 'NONE',  ( -0.000000000000000000, -1.000000000000000000, -0.000000000000000000 ) ) ;
#79824 = FACE_BOUND ( 'NONE', #30730, .T. ) ;
#79825 = DIRECTION ( 'NONE',  ( 0.000000000000000000, 0.000000000000000000, 1.000000000000000000 ) ) ;
#79826 = DIRECTION ( 'NONE',  ( -0.000000000000000000, 1.000000000000000000, -0.000000000000000000 ) ) ;
#79827 = LINE ( 'NONE', #82431, #79279 ) ;
#79828 = LINE ( 'NONE', #2541, #71374 ) ;
#79829 = DIRECTION ( 'NONE',  ( 0.000000000000000000, -0.000000000000000000, 1.000000000000000000 ) ) ;
#79830 = CYLINDRICAL_SURFACE ( 'NONE', #48839, 3.000000000000000000 ) ;
#79831 = PLANE ( 'NONE',  #107496 ) ;
#79832 = ORIENTED_EDGE ( 'NONE', *, *, #33479, .F. ) ;
#79833 = VECTOR ( 'NONE', #43596, 1000.000000000000000 ) ;
#79834 = LINE ( 'NONE', #66782, #19782 ) ;
#79835 = CIRCLE ( 'NONE', #71414, 0.06509327318403745899 ) ;
#79836 = LINE ( 'NONE', #91596, #129058 ) ;
#79837 = ORIENTED_EDGE ( 'NONE', *, *, #27842, .T. ) ;
#79838 = ORIENTED_EDGE ( 'NONE', *, *, #64388, .F. ) ;
#79839 = DIRECTION ( 'NONE',  ( 0.000000000000000000, -0.000000000000000000, -1.000000000000000000 ) ) ;
#79840 = CARTESIAN_POINT ( 'NONE',  ( -5.200000000000024158, 12.50000000000000000, -4.741630453620015118 ) ) ;
#79841 = FACE_BOUND ( 'NONE', #48530, .T. ) ;
#79842 = VECTOR ( 'NONE', #121496, 1000.000000000000000 ) ;
#79843 = DIRECTION ( 'NONE',  ( 0.000000000000000000, 0.000000000000000000, 1.000000000000000000 ) ) ;
#79845 = EDGE_CURVE ( 'NONE', #71852, #68242, #97913, .T. ) ;
#79844 = AXIS2_PLACEMENT_3D ( 'NONE', #34889, #124542, #57068 ) ;
#79847 = DIRECTION ( 'NONE',  ( -0.000000000000000000, 1.000000000000000000, -0.000000000000000000 ) ) ;
#79846 = CIRCLE ( 'NONE', #77776, 0.06509327318403745899 ) ;
#79848 = ORIENTED_EDGE ( 'NONE', *, *, #24614, .T. ) ;
#79849 = CARTESIAN_POINT ( 'NONE',  ( 10.19999999999991580, 2.500000000000000000, -0.2464101615137783419 ) ) ;
#79850 = EDGE_CURVE ( 'NONE', #15541, #66128, #73865, .T. ) ;
#79851 = DIRECTION ( 'NONE',  ( 0.000000000000000000, 0.000000000000000000, 1.000000000000000000 ) ) ;
#79852 = EDGE_CURVE ( 'NONE', #14663, #59275, #57352, .T. ) ;
#79853 = ORIENTED_EDGE ( 'NONE', *, *, #18056, .T. ) ;
#79855 = LINE ( 'NONE', #108023, #103267 ) ;
#79854 = VECTOR ( 'NONE', #125062, 1000.000000000000000 ) ;
#79856 = DIRECTION ( 'NONE',  ( -4.274815082592931898E-19, -0.9999939076577903929, -0.003490651415223739937 ) ) ;
#79857 = CIRCLE ( 'NONE', #17126, 0.06509327318403745899 ) ;
#79858 = CIRCLE ( 'NONE', #17129, 0.06509327318403745899 ) ;
#79859 = VECTOR ( 'NONE', #90529, 1000.000000000000000 ) ;
#79860 = AXIS2_PLACEMENT_3D ( 'NONE', #62980, #93100, #11940 ) ;
#79861 = ADVANCED_FACE ( 'NONE', ( #59310 ), #67140, .T. ) ;
#79862 = EDGE_CURVE ( 'NONE', #85603, #96773, #34169, .T. ) ;
#79863 = CARTESIAN_POINT ( 'NONE',  ( 10.39999999999990976, 12.50000000000000000, -4.265033745738164406 ) ) ;
#79864 = EDGE_CURVE ( 'NONE', #73360, #57691, #17410, .T. ) ;
#79865 = CARTESIAN_POINT ( 'NONE',  ( 9.599999999999914380, 2.500000000000000000, 3.737306695894644371 ) ) ;
#79866 = AXIS2_PLACEMENT_3D ( 'NONE', #37358, #18342, #126372 ) ;
#79867 = ORIENTED_EDGE ( 'NONE', *, *, #55614, .T. ) ;
#79868 = DIRECTION ( 'NONE',  ( 0.000000000000000000, 0.000000000000000000, 1.000000000000000000 ) ) ;
#79869 = ADVANCED_FACE ( 'NONE', ( #128027 ), #61356, .T. ) ;
#79870 = AXIS2_PLACEMENT_3D ( 'NONE', #76646, #26262, #126392 ) ;
#79871 = CARTESIAN_POINT ( 'NONE',  ( 8.149999999999920419, 2.500000000000000000, -2.411473670974877859 ) ) ;
#79872 = CARTESIAN_POINT ( 'NONE',  ( -5.450000000000019718, 12.50000000000000000, 6.495190528383297135 ) ) ;
#79873 = CARTESIAN_POINT ( 'NONE',  ( 6.649999999999931966, 2.500000000000000000, -7.188010851410854052 ) ) ;
#79874 = VERTEX_POINT ( 'NONE', #97274 ) ;
#79875 = EDGE_LOOP ( 'NONE', ( #102256, #112794 ) ) ;
#79876 = CARTESIAN_POINT ( 'NONE',  ( 1.899999999999951283, 12.50000000000000000, -4.676537180435977881 ) ) ;
#79877 = EDGE_CURVE ( 'NONE', #1361, #112572, #11163, .T. ) ;
#79878 = ORIENTED_EDGE ( 'NONE', *, *, #37157, .T. ) ;
#79879 = CARTESIAN_POINT ( 'NONE',  ( -3.300000000000027800, 12.50000000000000000, -2.276824562219559311E-15 ) ) ;
#79880 = CARTESIAN_POINT ( 'NONE',  ( 17.50000000000000000, -2.499999999999999556, 0.3333333333333385884 ) ) ;
#79881 = FACE_OUTER_BOUND ( 'NONE', #75958, .T. ) ;
#79882 = ORIENTED_EDGE ( 'NONE', *, *, #99658, .F. ) ;
#79883 = DIRECTION ( 'NONE',  ( 1.000000000000000000, 0.000000000000000000, 0.000000000000000000 ) ) ;
#79884 = DIRECTION ( 'NONE',  ( 0.000000000000000000, 0.000000000000000000, 1.000000000000000000 ) ) ;
#79885 = FACE_OUTER_BOUND ( 'NONE', #64101, .T. ) ;
#79886 = DIRECTION ( 'NONE',  ( -0.000000000000000000, 1.000000000000000000, -0.000000000000000000 ) ) ;
#79887 = CARTESIAN_POINT ( 'NONE',  ( 13.54999999999989946, 12.50000000000000000, 2.446380397790835826 ) ) ;
#79888 = CARTESIAN_POINT ( 'NONE',  ( -10.85000000000000142, 2.500000000000000000, 2.065063509461097624 ) ) ;
#79889 = ORIENTED_EDGE ( 'NONE', *, *, #4841, .F. ) ;
#79890 = ORIENTED_EDGE ( 'NONE', *, *, #114616, .T. ) ;
#79891 = DIRECTION ( 'NONE',  ( 0.000000000000000000, 0.000000000000000000, -1.000000000000000000 ) ) ;
#79892 = ORIENTED_EDGE ( 'NONE', *, *, #49495, .F. ) ;
#79893 = AXIS2_PLACEMENT_3D ( 'NONE', #50235, #9652, #49596 ) ;
#79894 = CARTESIAN_POINT ( 'NONE',  ( 12.89999999999989910, 2.500000000000000000, -0.6928203230275542523 ) ) ;
#79895 = AXIS2_PLACEMENT_3D ( 'NONE', #126508, #85284, #66291 ) ;
#79896 = CIRCLE ( 'NONE', #31788, 0.06509327318403745899 ) ;
#79898 = EDGE_LOOP ( 'NONE', ( #103568, #10862 ) ) ;
#79897 = ORIENTED_EDGE ( 'NONE', *, *, #81459, .F. ) ;
#79899 = VERTEX_POINT ( 'NONE', #78301 ) ;
#79900 = CARTESIAN_POINT ( 'NONE',  ( 17.50000000000000000, 0.4166666666666715146, -3.999999999999996447 ) ) ;
#79901 = DIRECTION ( 'NONE',  ( -4.274815082592931898E-19, -0.9999939076577903929, -0.003490651415223739937 ) ) ;
#79902 = AXIS2_PLACEMENT_3D ( 'NONE', #129438, #107832, #99308 ) ;
#79904 = DIRECTION ( 'NONE',  ( 0.000000000000000000, 0.000000000000000000, 1.000000000000000000 ) ) ;
#79903 = VECTOR ( 'NONE', #63534, 1000.000000000000000 ) ;
#79905 = CONICAL_SURFACE ( 'NONE', #67347, 0.09999999999999982514, 0.003490658503988666988 ) ;
#79906 = DIRECTION ( 'NONE',  ( 0.000000000000000000, 0.000000000000000000, 1.000000000000000000 ) ) ;
#79907 = DIRECTION ( 'NONE',  ( 0.000000000000000000, -0.000000000000000000, 1.000000000000000000 ) ) ;
#79908 = DIRECTION ( 'NONE',  ( -0.000000000000000000, -1.000000000000000000, -0.000000000000000000 ) ) ;
#79909 = AXIS2_PLACEMENT_3D ( 'NONE', #48031, #128540, #9384 ) ;
#79910 = FACE_OUTER_BOUND ( 'NONE', #53659, .T. ) ;
#79911 = FACE_OUTER_BOUND ( 'NONE', #71874, .T. ) ;
#79912 = CONICAL_SURFACE ( 'NONE', #84101, 0.09999999999999982514, 0.003490658503988666988 ) ;
#79913 = CARTESIAN_POINT ( 'NONE',  ( 9.149999999999915090, 2.500000000000000000, 6.395190528383296602 ) ) ;
#79915 = ORIENTED_EDGE ( 'NONE', *, *, #66583, .T. ) ;
#79914 = CIRCLE ( 'NONE', #12989, 0.06509327318403743123 ) ;
#79916 = VERTEX_POINT ( 'NONE', #51424 ) ;
#79917 = ADVANCED_FACE ( 'NONE', ( #110321 ), #91970, .T. ) ;
#79918 = DIRECTION ( 'NONE',  ( 0.000000000000000000, 0.000000000000000000, 1.000000000000000000 ) ) ;
#79919 = VERTEX_POINT ( 'NONE', #91323 ) ;
#79920 = VERTEX_POINT ( 'NONE', #20660 ) ;
#79921 = CARTESIAN_POINT ( 'NONE',  ( 4.599999999999936584, 2.500000000000000000, 3.537306695894645081 ) ) ;
#79922 = ADVANCED_FACE ( 'NONE', ( #22608 ), #84330, .T. ) ;
#79923 = FACE_OUTER_BOUND ( 'NONE', #120795, .T. ) ;
#79924 = DIRECTION ( 'NONE',  ( 0.000000000000000000, 0.000000000000000000, 1.000000000000000000 ) ) ;
#79925 = CARTESIAN_POINT ( 'NONE',  ( -13.14999999999999147, 2.500000000000000000, -1.918653347947324006 ) ) ;
#79926 = CARTESIAN_POINT ( 'NONE',  ( 12.49999999999993960, 12.50000000000000000, -4.330127018922201643 ) ) ;
#79927 = ORIENTED_EDGE ( 'NONE', *, *, #29583, .T. ) ;
#79928 = AXIS2_PLACEMENT_3D ( 'NONE', #107659, #67051, #48093 ) ;
#79929 = VERTEX_POINT ( 'NONE', #21963 ) ;
#79930 = DIRECTION ( 'NONE',  ( 0.000000000000000000, 0.000000000000000000, 1.000000000000000000 ) ) ;
#79931 = ORIENTED_EDGE ( 'NONE', *, *, #9519, .F. ) ;
#79932 = CARTESIAN_POINT ( 'NONE',  ( 13.54999999999989591, 12.50000000000000000, -1.818653347947326138 ) ) ;
#79933 = ORIENTED_EDGE ( 'NONE', *, *, #109678, .T. ) ;
#79934 = ORIENTED_EDGE ( 'NONE', *, *, #100125, .T. ) ;
#79935 = CIRCLE ( 'NONE', #17207, 0.09999999999999999167 ) ;
#79936 = CARTESIAN_POINT ( 'NONE',  ( 11.84999999999990727, 12.50000000000000000, 6.083687093685482772 ) ) ;
#79937 = CARTESIAN_POINT ( 'NONE',  ( 3.149999999999946176, 2.500000000000000000, -2.611473670974877592 ) ) ;
#79938 = AXIS2_PLACEMENT_3D ( 'NONE', #31009, #70910, #101003 ) ;
#79939 = CARTESIAN_POINT ( 'NONE',  ( -6.650000000000014566, 12.50000000000000000, 6.495190528383297135 ) ) ;
#79940 = CIRCLE ( 'NONE', #21449, 0.1000000000000002554 ) ;
#79941 = CARTESIAN_POINT ( 'NONE',  ( -1.250000000000001554, 2.500000000000000000, 6.495190528383297135 ) ) ;
#79942 = CARTESIAN_POINT ( 'NONE',  ( 17.50000000000000000, -0.4166666666666683505, 4.000000000000001776 ) ) ;
#79943 = EDGE_LOOP ( 'NONE', ( #37791, #29843 ) ) ;
#79944 = CARTESIAN_POINT ( 'NONE',  ( -1.700000000000035261, 12.50000000000000000, 4.330127018922196314 ) ) ;
#79945 = CARTESIAN_POINT ( 'NONE',  ( -7.900000000000011013, 2.500000000000000000, 5.122947341949749323 ) ) ;
#79946 = DIRECTION ( 'NONE',  ( -4.274815082592931898E-19, -0.9999939076577903929, -0.003490651415223739937 ) ) ;
#79947 = DIRECTION ( 'NONE',  ( 0.000000000000000000, 0.000000000000000000, 1.000000000000000000 ) ) ;
#79948 = VECTOR ( 'NONE', #111204, 1000.000000000000000 ) ;
#79949 = AXIS2_PLACEMENT_3D ( 'NONE', #70189, #110743, #10593 ) ;
#79950 = CARTESIAN_POINT ( 'NONE',  ( -12.89999999999999147, 2.500000000000000000, -0.6928203230275500335 ) ) ;
#79951 = ADVANCED_FACE ( 'NONE', ( #31139 ), #69755, .T. ) ;
#79952 = ORIENTED_EDGE ( 'NONE', *, *, #35621, .T. ) ;
#79953 = AXIS2_PLACEMENT_3D ( 'NONE', #108570, #80412, #60764 ) ;
#79954 = AXIS2_PLACEMENT_3D ( 'NONE', #12453, #1349, #52388 ) ;
#79955 = VECTOR ( 'NONE', #28869, 1000.000000000000000 ) ;
#79956 = VERTEX_POINT ( 'NONE', #71044 ) ;
#79957 = LINE ( 'NONE', #12500, #54945 ) ;
#79958 = CIRCLE ( 'NONE', #23516, 0.06509327318403745899 ) ;
#79959 = VERTEX_POINT ( 'NONE', #109683 ) ;
#79960 = DIRECTION ( 'NONE',  ( -0.000000000000000000, 1.000000000000000000, -0.000000000000000000 ) ) ;
#79962 = EDGE_CURVE ( 'NONE', #65030, #102327, #101057, .T. ) ;
#79961 = DIRECTION ( 'NONE',  ( -0.000000000000000000, 1.000000000000000000, -0.000000000000000000 ) ) ;
#79963 = AXIS2_PLACEMENT_3D ( 'NONE', #60249, #72632, #62810 ) ;
#79965 = ORIENTED_EDGE ( 'NONE', *, *, #77345, .T. ) ;
#79964 = ADVANCED_FACE ( 'NONE', ( #71683 ), #55183, .T. ) ;
#79966 = DIRECTION ( 'NONE',  ( 0.000000000000000000, 0.000000000000000000, 1.000000000000000000 ) ) ;
#79967 = CARTESIAN_POINT ( 'NONE',  ( 15.19999999999989093, 2.500000000000000000, 0.3464101615137735735 ) ) ;
#79968 = EDGE_CURVE ( 'NONE', #224, #91651, #53040, .T. ) ;
#79969 = CARTESIAN_POINT ( 'NONE',  ( -3.950000000000029932, 12.50000000000000000, -6.148780366869526226 ) ) ;
#79970 = CARTESIAN_POINT ( 'NONE',  ( -10.80000000000000249, 12.50000000000000000, -4.395220292106235327 ) ) ;
#79971 = EDGE_CURVE ( 'NONE', #125180, #66966, #2283, .T. ) ;
#79972 = EDGE_LOOP ( 'NONE', ( #41772, #73219, #35622, #107973 ) ) ;
#79973 = VECTOR ( 'NONE', #102168, 1000.000000000000000 ) ;
#79974 = EDGE_CURVE ( 'NONE', #101819, #102850, #110944, .T. ) ;
#79975 = CARTESIAN_POINT ( 'NONE',  ( 23.85228139349051091, 2.660541499546454247, -4.258215071919995154 ) ) ;
#79976 = FACE_OUTER_BOUND ( 'NONE', #14304, .T. ) ;
#79977 = FACE_OUTER_BOUND ( 'NONE', #69529, .T. ) ;
#79978 = VERTEX_POINT ( 'NONE', #82154 ) ;
#79979 = DIRECTION ( 'NONE',  ( 0.000000000000000000, 0.000000000000000000, 1.000000000000000000 ) ) ;
#79980 = VECTOR ( 'NONE', #19303, 1000.000000000000000 ) ;
#79981 = CIRCLE ( 'NONE', #23547, 2.000000000000000000 ) ;
#79982 = AXIS2_PLACEMENT_3D ( 'NONE', #42272, #101830, #122121 ) ;
#79983 = VERTEX_POINT ( 'NONE', #101151 ) ;
#79984 = CARTESIAN_POINT ( 'NONE',  ( 10.79999999999991367, 2.500000000000000000, -0.1000000000000023925 ) ) ;
#79985 = DIRECTION ( 'NONE',  ( 0.000000000000000000, 1.000000000000000000, 0.000000000000000000 ) ) ;
#79986 = LINE ( 'NONE', #120561, #81020 ) ;
#79987 = VERTEX_POINT ( 'NONE', #62527 ) ;
#79989 = LINE ( 'NONE', #27646, #40548 ) ;
#79988 = VECTOR ( 'NONE', #72688, 1000.000000000000000 ) ;
#79990 = AXIS2_PLACEMENT_3D ( 'NONE', #1865, #62745, #111158 ) ;
#79991 = VECTOR ( 'NONE', #125975, 1000.000000000000000 ) ;
#79992 = DIRECTION ( 'NONE',  ( -4.274815082592931898E-19, -0.9999939076577903929, -0.003490651415223739937 ) ) ;
#79993 = CIRCLE ( 'NONE', #8878, 0.06509327318403745899 ) ;
#79994 = VERTEX_POINT ( 'NONE', #119484 ) ;
#79995 = CIRCLE ( 'NONE', #31991, 0.06509327318403745899 ) ;
#79996 = DIRECTION ( 'NONE',  ( 0.000000000000000000, 1.000000000000000000, 0.000000000000000000 ) ) ;
#79997 = ORIENTED_EDGE ( 'NONE', *, *, #24033, .T. ) ;
#79998 = CIRCLE ( 'NONE', #125965, 0.06509327318403745899 ) ;
#79999 = CARTESIAN_POINT ( 'NONE',  ( -10.20000000000000284, 2.500000000000000000, -0.4464101615137782142 ) ) ;
#80000 = EDGE_CURVE ( 'NONE', #29710, #55568, #21733, .T. ) ;
#80001 = ORIENTED_EDGE ( 'NONE', *, *, #27576, .F. ) ;
#80002 = DIRECTION ( 'NONE',  ( -0.000000000000000000, 1.000000000000000000, -0.000000000000000000 ) ) ;
#80003 = DIRECTION ( 'NONE',  ( -0.000000000000000000, -1.000000000000000000, -0.000000000000000000 ) ) ;
#80004 = EDGE_LOOP ( 'NONE', ( #63458, #25864 ) ) ;
#80005 = ORIENTED_EDGE ( 'NONE', *, *, #71246, .F. ) ;
#80006 = DIRECTION ( 'NONE',  ( 0.000000000000000000, 1.000000000000000000, 0.000000000000000000 ) ) ;
#80007 = DIRECTION ( 'NONE',  ( -0.000000000000000000, 1.000000000000000000, -0.000000000000000000 ) ) ;
#80008 = ORIENTED_EDGE ( 'NONE', *, *, #29625, .F. ) ;
#80009 = ADVANCED_FACE ( 'NONE', ( #122084 ), #29831, .T. ) ;
#80010 = CIRCLE ( 'NONE', #71698, 0.09999999999999999167 ) ;
#80011 = DIRECTION ( 'NONE',  ( 0.000000000000000000, 0.000000000000000000, 1.000000000000000000 ) ) ;
#80012 = FACE_OUTER_BOUND ( 'NONE', #84450, .T. ) ;
#80013 = CARTESIAN_POINT ( 'NONE',  ( -4.150000000000025224, 2.500000000000000000, 6.495190528383297135 ) ) ;
#80014 = DIRECTION ( 'NONE',  ( 0.000000000000000000, 0.000000000000000000, 1.000000000000000000 ) ) ;
#80015 = PLANE ( 'NONE',  #15342 ) ;
#80016 = EDGE_CURVE ( 'NONE', #123447, #69623, #39675, .T. ) ;
#80017 = DIRECTION ( 'NONE',  ( 0.000000000000000000, -0.9999939076577903929, 0.003490651415223739937 ) ) ;
#80018 = FACE_OUTER_BOUND ( 'NONE', #14845, .T. ) ;
#80019 = EDGE_CURVE ( 'NONE', #103166, #122201, #52689, .T. ) ;
#80020 = EDGE_CURVE ( 'NONE', #119523, #23602, #34270, .T. ) ;
#80021 = AXIS2_PLACEMENT_3D ( 'NONE', #75446, #115353, #25709 ) ;
#80022 = AXIS2_PLACEMENT_3D ( 'NONE', #10148, #89981, #78259 ) ;
#80023 = VERTEX_POINT ( 'NONE', #59964 ) ;
#80024 = ORIENTED_EDGE ( 'NONE', *, *, #84833, .F. ) ;
#80025 = EDGE_CURVE ( 'NONE', #26527, #3072, #126188, .T. ) ;
#80026 = ORIENTED_EDGE ( 'NONE', *, *, #93004, .F. ) ;
#80027 = CARTESIAN_POINT ( 'NONE',  ( 7.049999999999930544, 12.50000000000000000, -6.560283801567339701 ) ) ;
#80028 = FACE_OUTER_BOUND ( 'NONE', #63953, .T. ) ;
#80029 = DIRECTION ( 'NONE',  ( 0.000000000000000000, 0.000000000000000000, -1.000000000000000000 ) ) ;
#80030 = ORIENTED_EDGE ( 'NONE', *, *, #2270, .F. ) ;
#80031 = FACE_BOUND ( 'NONE', #23189, .T. ) ;
#80032 = EDGE_LOOP ( 'NONE', ( #1736, #1665 ) ) ;
#80033 = AXIS2_PLACEMENT_3D ( 'NONE', #38650, #119757, #80500 ) ;
#80034 = DIRECTION ( 'NONE',  ( 0.000000000000000000, -0.000000000000000000, 1.000000000000000000 ) ) ;
#80035 = DIRECTION ( 'NONE',  ( 0.000000000000000000, 0.000000000000000000, -1.000000000000000000 ) ) ;
#80036 = ADVANCED_FACE ( 'NONE', ( #10191 ), #17507, .T. ) ;
#80037 = LINE ( 'NONE', #120606, #30491 ) ;
#80038 = EDGE_CURVE ( 'NONE', #50530, #124116, #33072, .T. ) ;
#80039 = CONICAL_SURFACE ( 'NONE', #25740, 0.1000000000000002554, 0.003490658503988666988 ) ;
#80040 = DIRECTION ( 'NONE',  ( 0.000000000000000000, 0.000000000000000000, -1.000000000000000000 ) ) ;
#80041 = DIRECTION ( 'NONE',  ( -4.274815082592931898E-19, -0.9999939076577903929, -0.003490651415223739937 ) ) ;
#80042 = DIRECTION ( 'NONE',  ( -4.274815082592931898E-19, -0.9999939076577903929, -0.003490651415223739937 ) ) ;
#80043 = CARTESIAN_POINT ( 'NONE',  ( 11.89999999999990798, 12.50000000000000000, 3.983716857408420964 ) ) ;
#80044 = LINE ( 'NONE', #87905, #53651 ) ;
#80045 = VECTOR ( 'NONE', #103988, 1000.000000000000000 ) ;
#80046 = CARTESIAN_POINT ( 'NONE',  ( 8.299999999999922551, 2.500000000000000000, -4.330127018922201643 ) ) ;
#80047 = AXIS2_PLACEMENT_3D ( 'NONE', #6559, #107378, #46510 ) ;
#80048 = ORIENTED_EDGE ( 'NONE', *, *, #90174, .F. ) ;
#80049 = ORIENTED_EDGE ( 'NONE', *, *, #53627, .F. ) ;
#80050 = VERTEX_POINT ( 'NONE', #75534 ) ;
#80052 = ORIENTED_EDGE ( 'NONE', *, *, #70151, .F. ) ;
#80051 = AXIS2_PLACEMENT_3D ( 'NONE', #62706, #61426, #52237 ) ;
#80053 = CIRCLE ( 'NONE', #123949, 0.1000000000000002554 ) ;
#80054 = CONICAL_SURFACE ( 'NONE', #117583, 0.09999999999999982514, 0.003490658503988666988 ) ;
#80055 = CARTESIAN_POINT ( 'NONE',  ( -4.150000000000025224, 2.500000000000000000, 5.802370205355744659 ) ) ;
#80056 = LINE ( 'NONE', #2779, #13078 ) ;
#80058 = ORIENTED_EDGE ( 'NONE', *, *, #66152, .F. ) ;
#80057 = ORIENTED_EDGE ( 'NONE', *, *, #24851, .T. ) ;
#80059 = VERTEX_POINT ( 'NONE', #105663 ) ;
#80060 = VECTOR ( 'NONE', #73727, 1000.000000000000000 ) ;
#80061 = CARTESIAN_POINT ( 'NONE',  ( -4.999999999999986677, 2.500000000000000000, -0.1000000000000022815 ) ) ;
#80062 = DIRECTION ( 'NONE',  ( 0.000000000000000000, 0.000000000000000000, 1.000000000000000000 ) ) ;
#80063 = VECTOR ( 'NONE', #129488, 1000.000000000000000 ) ;
#80064 = CARTESIAN_POINT ( 'NONE',  ( 5.599999999999933031, 2.500000000000000000, 0.3464101615137735735 ) ) ;
#80065 = DIRECTION ( 'NONE',  ( 0.000000000000000000, 0.000000000000000000, 1.000000000000000000 ) ) ;
#80066 = DIRECTION ( 'NONE',  ( 0.000000000000000000, -1.846105847067148515E-16, -1.000000000000000000 ) ) ;
#80067 = CARTESIAN_POINT ( 'NONE',  ( 133.2169897921533845, 2.500000000000000000, -2.337293474289257933 ) ) ;
#80068 = LINE ( 'NONE', #9399, #46846 ) ;
#80069 = EDGE_LOOP ( 'NONE', ( #37073, #106041, #71327, #75926 ) ) ;
#80070 = DIRECTION ( 'NONE',  ( 0.000000000000000000, -0.000000000000000000, 1.000000000000000000 ) ) ;
#80071 = ORIENTED_EDGE ( 'NONE', *, *, #69957, .F. ) ;
#80072 = EDGE_LOOP ( 'NONE', ( #87592, #77591, #83923, #9104 ) ) ;
#80073 = ADVANCED_FACE ( 'NONE', ( #124661 ), #63151, .T. ) ;
#80074 = ORIENTED_EDGE ( 'NONE', *, *, #25808, .F. ) ;
#80075 = CARTESIAN_POINT ( 'NONE',  ( -3.950000000000026379, 2.500000000000000000, 6.841600689897072485 ) ) ;
#80076 = AXIS2_PLACEMENT_3D ( 'NONE', #54615, #64443, #114824 ) ;
#80077 = VECTOR ( 'NONE', #66741, 1000.000000000000000 ) ;
#80078 = EDGE_LOOP ( 'NONE', ( #42168, #6969, #29144, #21118, #48149 ) ) ;
#80079 = VERTEX_POINT ( 'NONE', #2952 ) ;
#80080 = DIRECTION ( 'NONE',  ( 0.000000000000000000, 0.000000000000000000, -1.000000000000000000 ) ) ;
#80081 = ADVANCED_FACE ( 'NONE', ( #14676 ), #117852, .T. ) ;
#80083 = CARTESIAN_POINT ( 'NONE',  ( 2.049999999999948308, 2.500000000000000000, 6.395190528383296602 ) ) ;
#80082 = CIRCLE ( 'NONE', #86609, 0.06509327318403745899 ) ;
#80084 = DIRECTION ( 'NONE',  ( -0.000000000000000000, -1.000000000000000000, -0.000000000000000000 ) ) ;
#80086 = DIRECTION ( 'NONE',  ( 0.000000000000000000, 1.000000000000000000, 0.000000000000000000 ) ) ;
#80085 = CIRCLE ( 'NONE', #103059, 0.06509327318403745899 ) ;
#80087 = VECTOR ( 'NONE', #128196, 1000.000000000000000 ) ;
#80088 = CIRCLE ( 'NONE', #88370, 0.06509327318403741736 ) ;
#80089 = DIRECTION ( 'NONE',  ( 0.000000000000000000, 1.000000000000000000, 0.000000000000000000 ) ) ;
#80090 = VERTEX_POINT ( 'NONE', #115449 ) ;
#80091 = CARTESIAN_POINT ( 'NONE',  ( -5.650000000000019895, 12.50000000000000000, 2.511473670974873507 ) ) ;
#80092 = AXIS2_PLACEMENT_3D ( 'NONE', #88273, #46431, #128244 ) ;
#80094 = ORIENTED_EDGE ( 'NONE', *, *, #40736, .F. ) ;
#80093 = CIRCLE ( 'NONE', #40393, 0.1000000000000000472 ) ;
#80095 = FACE_OUTER_BOUND ( 'NONE', #1839, .T. ) ;
#80096 = CIRCLE ( 'NONE', #4857, 0.06509327318403745899 ) ;
#80097 = ORIENTED_EDGE ( 'NONE', *, *, #41947, .T. ) ;
#80098 = DIRECTION ( 'NONE',  ( 0.000000000000000000, 0.000000000000000000, -1.000000000000000000 ) ) ;
#80099 = DIRECTION ( 'NONE',  ( -4.274815082592931898E-19, -0.9999939076577903929, -0.003490651415223739937 ) ) ;
#80100 = CIRCLE ( 'NONE', #103077, 0.06509327318403745899 ) ;
#80101 = ORIENTED_EDGE ( 'NONE', *, *, #18016, .F. ) ;
#80102 = AXIS2_PLACEMENT_3D ( 'NONE', #38747, #97634, #77994 ) ;
#80103 = CARTESIAN_POINT ( 'NONE',  ( 3.099999999999945466, 12.50000000000000000, 0.3464101615137735735 ) ) ;
#80104 = LINE ( 'NONE', #8756, #125174 ) ;
#80105 = EDGE_LOOP ( 'NONE', ( #57948, #4146, #47791, #13959 ) ) ;
#80106 = AXIS2_PLACEMENT_3D ( 'NONE', #37459, #117926, #46612 ) ;
#80107 = CARTESIAN_POINT ( 'NONE',  ( -7.100000000000017408, 2.500000000000000000, 0.7928203230275495672 ) ) ;
#80108 = ORIENTED_EDGE ( 'NONE', *, *, #69046, .T. ) ;
#80109 = ORIENTED_EDGE ( 'NONE', *, *, #13520, .F. ) ;
#80110 = DIRECTION ( 'NONE',  ( 0.000000000000000000, -0.9999939076577903929, 0.003490651415223739937 ) ) ;
#80111 = DIRECTION ( 'NONE',  ( 0.000000000000000000, -0.9999939076577903929, 0.003490651415223739937 ) ) ;
#80112 = CARTESIAN_POINT ( 'NONE',  ( 184.8385416670080872, 6.551208109652274736, 3.782341765625001351 ) ) ;
#80113 = DIRECTION ( 'NONE',  ( -0.000000000000000000, -1.000000000000000000, -0.000000000000000000 ) ) ;
#80114 = CONICAL_SURFACE ( 'NONE', #69643, 0.09999999999999982514, 0.003490658503988666988 ) ;
#80115 = DIRECTION ( 'NONE',  ( 0.000000000000000000, 0.000000000000000000, -1.000000000000000000 ) ) ;
#80116 = VERTEX_POINT ( 'NONE', #85369 ) ;
#80117 = DIRECTION ( 'NONE',  ( 0.000000000000000000, 0.000000000000000000, -1.000000000000000000 ) ) ;
#80118 = ORIENTED_EDGE ( 'NONE', *, *, #129442, .F. ) ;
#80119 = AXIS2_PLACEMENT_3D ( 'NONE', #112862, #61182, #2911 ) ;
#80120 = DIRECTION ( 'NONE',  ( 0.000000000000000000, 0.000000000000000000, 1.000000000000000000 ) ) ;
#80122 = EDGE_CURVE ( 'NONE', #17444, #43807, #74267, .T. ) ;
#80121 = DIRECTION ( 'NONE',  ( 0.000000000000000000, 0.000000000000000000, 1.000000000000000000 ) ) ;
#80123 = CIRCLE ( 'NONE', #96830, 0.06509327318403745899 ) ;
#80124 = EDGE_CURVE ( 'NONE', #117313, #38438, #25807, .T. ) ;
#80125 = DIRECTION ( 'NONE',  ( 0.000000000000000000, 0.000000000000000000, 1.000000000000000000 ) ) ;
#80126 = FACE_OUTER_BOUND ( 'NONE', #51809, .T. ) ;
#80127 = CARTESIAN_POINT ( 'NONE',  ( -8.100000000000013856, 2.500000000000000000, 0.3464101615137736845 ) ) ;
#80128 = DIRECTION ( 'NONE',  ( -0.000000000000000000, -1.000000000000000000, -0.000000000000000000 ) ) ;
#80129 = CIRCLE ( 'NONE', #73863, 0.06509327318403745899 ) ;
#80130 = EDGE_CURVE ( 'NONE', #66886, #107927, #44815, .T. ) ;
#80132 = CIRCLE ( 'NONE', #82285, 0.06509327318403745899 ) ;
#80131 = LINE ( 'NONE', #260, #49615 ) ;
#80133 = VERTEX_POINT ( 'NONE', #84722 ) ;
#80134 = VECTOR ( 'NONE', #51722, 1000.000000000000000 ) ;
#80135 = CIRCLE ( 'NONE', #13214, 0.06509327318403745899 ) ;
#80136 = DIRECTION ( 'NONE',  ( 0.000000000000000000, 0.000000000000000000, -1.000000000000000000 ) ) ;
#80137 = CARTESIAN_POINT ( 'NONE',  ( 13.94999999999989448, 2.500000000000000000, -2.411473670974877859 ) ) ;
#80138 = CARTESIAN_POINT ( 'NONE',  ( 13.54999999999989768, 12.50000000000000000, -2.511473670974877948 ) ) ;
#80139 = EDGE_CURVE ( 'NONE', #32427, #91045, #30059, .T. ) ;
#80140 = EDGE_CURVE ( 'NONE', #32930, #92950, #82385, .T. ) ;
#80141 = EDGE_CURVE ( 'NONE', #45961, #11906, #122089, .T. ) ;
#80142 = ORIENTED_EDGE ( 'NONE', *, *, #31755, .T. ) ;
#80143 = CARTESIAN_POINT ( 'NONE',  ( -4.350000000000023626, 2.500000000000000000, 6.248780366869521430 ) ) ;
#80144 = EDGE_LOOP ( 'NONE', ( #14400, #6159 ) ) ;
#80146 = VERTEX_POINT ( 'NONE', #72976 ) ;
#80145 = CIRCLE ( 'NONE', #84345, 0.06509327318403745899 ) ;
#80147 = CIRCLE ( 'NONE', #121912, 0.06509327318403745899 ) ;
#80148 = DIRECTION ( 'NONE',  ( -0.000000000000000000, -1.000000000000000000, -0.000000000000000000 ) ) ;
#80150 = ORIENTED_EDGE ( 'NONE', *, *, #9910, .T. ) ;
#80149 = VECTOR ( 'NONE', #107713, 1000.000000000000000 ) ;
#80151 = CARTESIAN_POINT ( 'NONE',  ( -7.100000000000018296, 2.500000000000000000, -0.1000000000000023925 ) ) ;
#80152 = CARTESIAN_POINT ( 'NONE',  ( -3.100000000000028511, 12.50000000000000000, 0.3464101615137736845 ) ) ;
#80153 = ORIENTED_EDGE ( 'NONE', *, *, #23426, .T. ) ;
#80154 = DIRECTION ( 'NONE',  ( 0.000000000000000000, -0.9999939076577903929, 0.003490651415223739937 ) ) ;
#80155 = CARTESIAN_POINT ( 'NONE',  ( -9.150000000000009237, 2.500000000000000000, 2.857883832488649301 ) ) ;
#80156 = ORIENTED_EDGE ( 'NONE', *, *, #114205, .F. ) ;
#80157 = EDGE_LOOP ( 'NONE', ( #48395, #89825 ) ) ;
#80158 = ORIENTED_EDGE ( 'NONE', *, *, #61293, .T. ) ;
#80159 = DIRECTION ( 'NONE',  ( 0.000000000000000000, 0.000000000000000000, 1.000000000000000000 ) ) ;
#80160 = CARTESIAN_POINT ( 'NONE',  ( 6.699999999999930012, 2.500000000000000000, 4.330127018922196314 ) ) ;
#80162 = PLANE ( 'NONE',  #54718 ) ;
#80161 = AXIS2_PLACEMENT_3D ( 'NONE', #105353, #47090, #37895 ) ;
#80163 = CIRCLE ( 'NONE', #67723, 0.06509327318403745899 ) ;
#80164 = FACE_BOUND ( 'NONE', #61692, .T. ) ;
#80165 = ORIENTED_EDGE ( 'NONE', *, *, #76594, .T. ) ;
#80166 = DIRECTION ( 'NONE',  ( 0.000000000000000000, 0.000000000000000000, -1.000000000000000000 ) ) ;
#80167 = DIRECTION ( 'NONE',  ( 0.000000000000000000, 0.000000000000000000, 1.000000000000000000 ) ) ;
#80168 = ORIENTED_EDGE ( 'NONE', *, *, #37048, .F. ) ;
#80169 = DIRECTION ( 'NONE',  ( 0.000000000000000000, 1.000000000000000000, 0.000000000000000000 ) ) ;
#80171 = DIRECTION ( 'NONE',  ( 0.000000000000000000, 1.000000000000000000, 0.000000000000000000 ) ) ;
#80170 = AXIS2_PLACEMENT_3D ( 'NONE', #12175, #61952, #92040 ) ;
#80172 = AXIS2_PLACEMENT_3D ( 'NONE', #88451, #7962, #47910 ) ;
#80173 = CONICAL_SURFACE ( 'NONE', #98955, 0.1000000000000000472, 0.003490658503988666988 ) ;
#80176 = EDGE_CURVE ( 'NONE', #56205, #83060, #4986, .T. ) ;
#80175 = AXIS2_PLACEMENT_3D ( 'NONE', #38922, #98434, #59189 ) ;
#80174 = CARTESIAN_POINT ( 'NONE',  ( 14.99999999999989164, 2.500000000000000000, 0.7928203230275495672 ) ) ;
#80177 = PLANE ( 'NONE',  #57151 ) ;
#80178 = CARTESIAN_POINT ( 'NONE',  ( 1.649999999999949729, 2.500000000000000000, 5.802370205355744659 ) ) ;
#80179 = ADVANCED_FACE ( 'NONE', ( #25152 ), #80230, .T. ) ;
#80180 = FACE_OUTER_BOUND ( 'NONE', #69689, .T. ) ;
#80181 = DIRECTION ( 'NONE',  ( -0.000000000000000000, 1.000000000000000000, -0.000000000000000000 ) ) ;
#80182 = ADVANCED_FACE ( 'NONE', ( #33695 ), #38475, .T. ) ;
#80183 = AXIS2_PLACEMENT_3D ( 'NONE', #14422, #74010, #66752 ) ;
#80184 = AXIS2_PLACEMENT_3D ( 'NONE', #39522, #21133, #108227 ) ;
#80185 = CIRCLE ( 'NONE', #11215, 0.06509327318403745899 ) ;
#80186 = VERTEX_POINT ( 'NONE', #42898 ) ;
#80187 = ORIENTED_EDGE ( 'NONE', *, *, #77544, .T. ) ;
#80189 = VERTEX_POINT ( 'NONE', #82811 ) ;
#80188 = EDGE_CURVE ( 'NONE', #120463, #84952, #23795, .T. ) ;
#80191 = ORIENTED_EDGE ( 'NONE', *, *, #59026, .T. ) ;
#80190 = CIRCLE ( 'NONE', #96340, 1.000000000000000000 ) ;
#80192 = CARTESIAN_POINT ( 'NONE',  ( -3.750000000000027978, 2.500000000000000000, 7.188010851410848723 ) ) ;
#80193 = EDGE_CURVE ( 'NONE', #66198, #64623, #45466, .T. ) ;
#80194 = CIRCLE ( 'NONE', #105318, 0.06509327318403745899 ) ;
#80195 = FACE_OUTER_BOUND ( 'NONE', #40781, .T. ) ;
#80197 = EDGE_CURVE ( 'NONE', #30016, #13274, #59407, .T. ) ;
#80196 = VERTEX_POINT ( 'NONE', #35636 ) ;
#80198 = FACE_BOUND ( 'NONE', #37997, .T. ) ;
#80199 = DIRECTION ( 'NONE',  ( 0.000000000000000000, 0.000000000000000000, -1.000000000000000000 ) ) ;
#80200 = EDGE_CURVE ( 'NONE', #97088, #76654, #23889, .T. ) ;
#80201 = DIRECTION ( 'NONE',  ( 0.000000000000000000, 1.000000000000000000, 0.000000000000000000 ) ) ;
#80202 = EDGE_CURVE ( 'NONE', #99291, #47871, #34357, .T. ) ;
#80203 = FACE_OUTER_BOUND ( 'NONE', #6493, .T. ) ;
#80204 = DIRECTION ( 'NONE',  ( 0.000000000000000000, 1.000000000000000000, 0.000000000000000000 ) ) ;
#80205 = CARTESIAN_POINT ( 'NONE',  ( -9.999999999999969802, 2.500000000000000000, -2.276824562219559311E-15 ) ) ;
#80206 = CARTESIAN_POINT ( 'NONE',  ( 0.3999999999999568345, 12.50000000000000000, -3.637306695894650055 ) ) ;
#80207 = DIRECTION ( 'NONE',  ( 0.000000000000000000, 0.000000000000000000, 1.000000000000000000 ) ) ;
#80208 = VERTEX_POINT ( 'NONE', #56543 ) ;
#80209 = EDGE_CURVE ( 'NONE', #23974, #82534, #19675, .T. ) ;
#80210 = AXIS2_PLACEMENT_3D ( 'NONE', #3361, #113310, #23645 ) ;
#80211 = ORIENTED_EDGE ( 'NONE', *, *, #95102, .F. ) ;
#80212 = ORIENTED_EDGE ( 'NONE', *, *, #63182, .F. ) ;
#80213 = ORIENTED_EDGE ( 'NONE', *, *, #72482, .T. ) ;
#80214 = VERTEX_POINT ( 'NONE', #48038 ) ;
#80215 = EDGE_LOOP ( 'NONE', ( #48719, #100364 ) ) ;
#80216 = DIRECTION ( 'NONE',  ( -4.274815082592931898E-19, -0.9999939076577903929, -0.003490651415223739937 ) ) ;
#80217 = DIRECTION ( 'NONE',  ( 0.000000000000000000, 0.000000000000000000, 1.000000000000000000 ) ) ;
#80218 = EDGE_LOOP ( 'NONE', ( #63843, #55390 ) ) ;
#80219 = CARTESIAN_POINT ( 'NONE',  ( -8.350000000000013856, 2.500000000000000000, -2.165063509461101710 ) ) ;
#80220 = CIRCLE ( 'NONE', #50673, 0.1000000000000000472 ) ;
#80221 = CIRCLE ( 'NONE', #42578, 0.06509327318403745899 ) ;
#80222 = CARTESIAN_POINT ( 'NONE',  ( -11.84999999999999787, 2.500000000000000000, -1.818653347947321919 ) ) ;
#80223 = CARTESIAN_POINT ( 'NONE',  ( 185.3177083336747160, 4.367472073101515306, 7.564683531250000925 ) ) ;
#80224 = DIRECTION ( 'NONE',  ( -0.000000000000000000, -1.000000000000000000, -0.000000000000000000 ) ) ;
#80225 = CARTESIAN_POINT ( 'NONE',  ( 1.449999999999952660, 12.50000000000000000, -6.841600689897078702 ) ) ;
#80226 = CIRCLE ( 'NONE', #115810, 0.09999999999999982514 ) ;
#80227 = VERTEX_POINT ( 'NONE', #76203 ) ;
#80228 = DIRECTION ( 'NONE',  ( 0.000000000000000000, 0.000000000000000000, 1.000000000000000000 ) ) ;
#80229 = CIRCLE ( 'NONE', #123832, 0.06509327318403745899 ) ;
#80230 = CONICAL_SURFACE ( 'NONE', #115812, 0.09999999999999982514, 0.003490658503988666988 ) ;
#80231 = VERTEX_POINT ( 'NONE', #6777 ) ;
#80232 = VERTEX_POINT ( 'NONE', #16612 ) ;
#80233 = LINE ( 'NONE', #48847, #78222 ) ;
#80234 = DIRECTION ( 'NONE',  ( -0.000000000000000000, -1.000000000000000000, -0.000000000000000000 ) ) ;
#80235 = DIRECTION ( 'NONE',  ( 0.000000000000000000, 0.000000000000000000, 1.000000000000000000 ) ) ;
#80236 = VECTOR ( 'NONE', #97902, 1000.000000000000000 ) ;
#80237 = EDGE_LOOP ( 'NONE', ( #49009, #128109, #17872, #95370 ) ) ;
#80238 = ORIENTED_EDGE ( 'NONE', *, *, #117330, .F. ) ;
#80239 = DIRECTION ( 'NONE',  ( -0.000000000000000000, 1.000000000000000000, -0.000000000000000000 ) ) ;
#80240 = EDGE_CURVE ( 'NONE', #41669, #122705, #92846, .T. ) ;
#80242 = AXIS2_PLACEMENT_3D ( 'NONE', #18490, #58435, #8649 ) ;
#80241 = CARTESIAN_POINT ( 'NONE',  ( 106.0514428414850272, 9.000000000000001776, -1.125000000000000222 ) ) ;
#80244 = AXIS2_PLACEMENT_3D ( 'NONE', #18993, #50398, #98851 ) ;
#80243 = CARTESIAN_POINT ( 'NONE',  ( 7.949999999999922018, 2.500000000000000000, 6.595190528383296780 ) ) ;
#80245 = CONICAL_SURFACE ( 'NONE', #57253, 0.1000000000000002554, 0.003490658503988666988 ) ;
#80246 = DIRECTION ( 'NONE',  ( -0.000000000000000000, -1.000000000000000000, -0.000000000000000000 ) ) ;
#80247 = VERTEX_POINT ( 'NONE', #18564 ) ;
#80248 = DIRECTION ( 'NONE',  ( 0.000000000000000000, 0.000000000000000000, 1.000000000000000000 ) ) ;
#80249 = CIRCLE ( 'NONE', #51012, 0.06509327318403743123 ) ;
#80250 = ORIENTED_EDGE ( 'NONE', *, *, #107484, .F. ) ;
#80251 = CONICAL_SURFACE ( 'NONE', #7058, 0.1000000000000002554, 0.003490658503988666988 ) ;
#80252 = DIRECTION ( 'NONE',  ( 0.000000000000000000, 1.000000000000000000, 0.000000000000000000 ) ) ;
#80253 = EDGE_LOOP ( 'NONE', ( #82138, #32191, #4977, #106669 ) ) ;
#80254 = CARTESIAN_POINT ( 'NONE',  ( 186.4583333333333428, 4.445597072760147483, 7.699999999999948663 ) ) ;
#80255 = CARTESIAN_POINT ( 'NONE',  ( -11.24999999999996270, 2.500000000000000000, 2.265063509461097357 ) ) ;
#80256 = DIRECTION ( 'NONE',  ( -0.000000000000000000, -1.000000000000000000, -0.000000000000000000 ) ) ;
#80257 = CARTESIAN_POINT ( 'NONE',  ( -14.14999999999998792, 2.500000000000000000, -1.572243186433547990 ) ) ;
#80258 = ORIENTED_EDGE ( 'NONE', *, *, #43784, .T. ) ;
#80259 = DIRECTION ( 'NONE',  ( 0.000000000000000000, 0.000000000000000000, 1.000000000000000000 ) ) ;
#80260 = DIRECTION ( 'NONE',  ( 0.000000000000000000, 0.000000000000000000, 1.000000000000000000 ) ) ;
#80261 = VERTEX_POINT ( 'NONE', #7442 ) ;
#80262 = ORIENTED_EDGE ( 'NONE', *, *, #46912, .F. ) ;
#80263 = VECTOR ( 'NONE', #93444, 1000.000000000000000 ) ;
#80264 = AXIS2_PLACEMENT_3D ( 'NONE', #71323, #121719, #83106 ) ;
#80265 = ORIENTED_EDGE ( 'NONE', *, *, #22881, .T. ) ;
#80266 = LINE ( 'NONE', #58687, #31145 ) ;
#80267 = CARTESIAN_POINT ( 'NONE',  ( -1.250000000000037526, 2.500000000000000000, -5.702370205355749455 ) ) ;
#80268 = DIRECTION ( 'NONE',  ( 0.000000000000000000, 0.000000000000000000, -1.000000000000000000 ) ) ;
#80269 = CARTESIAN_POINT ( 'NONE',  ( 187.0677083336747444, -4.367472073101514418, -7.564683531250002702 ) ) ;
#80270 = LINE ( 'NONE', #20066, #9329 ) ;
#80271 = FACE_OUTER_BOUND ( 'NONE', #106789, .T. ) ;
#80272 = CIRCLE ( 'NONE', #46819, 0.1000000000000002554 ) ;
#80273 = AXIS2_PLACEMENT_3D ( 'NONE', #60644, #19395, #78995 ) ;
#80274 = DIRECTION ( 'NONE',  ( 0.000000000000000000, -0.000000000000000000, 1.000000000000000000 ) ) ;
#80275 = CARTESIAN_POINT ( 'NONE',  ( 7.949999999999925571, 12.50000000000000000, 2.230156782645134950 ) ) ;
#80277 = VECTOR ( 'NONE', #117888, 1000.000000000000000 ) ;
#80276 = CARTESIAN_POINT ( 'NONE',  ( -12.04999999999999716, 2.500000000000000000, -2.265063509461097802 ) ) ;
#80278 = CIRCLE ( 'NONE', #74013, 0.1000000000000002554 ) ;
#80279 = AXIS2_PLACEMENT_3D ( 'NONE', #116458, #13740, #55616 ) ;
#80281 = ADVANCED_FACE ( 'NONE', ( #106927 ), #46741, .T. ) ;
#80280 = VECTOR ( 'NONE', #41396, 1000.000000000000000 ) ;
#80282 = ORIENTED_EDGE ( 'NONE', *, *, #12622, .T. ) ;
#80283 = CARTESIAN_POINT ( 'NONE',  ( -0.6500000000000389910, 2.500000000000000000, -6.148780366869526226 ) ) ;
#80284 = AXIS2_PLACEMENT_3D ( 'NONE', #46435, #77829, #126304 ) ;
#80285 = EDGE_CURVE ( 'NONE', #106593, #73695, #107592, .T. ) ;
#80286 = DIRECTION ( 'NONE',  ( -0.000000000000000000, -1.000000000000000000, -0.000000000000000000 ) ) ;
#80287 = DIRECTION ( 'NONE',  ( 0.000000000000000000, 0.000000000000000000, 1.000000000000000000 ) ) ;
#80288 = CARTESIAN_POINT ( 'NONE',  ( -11.05000000000000071, 2.500000000000000000, -6.841600689897075149 ) ) ;
#80289 = LINE ( 'NONE', #120209, #100197 ) ;
#80290 = EDGE_CURVE ( 'NONE', #109720, #115027, #113674, .T. ) ;
#80291 = ORIENTED_EDGE ( 'NONE', *, *, #94645, .T. ) ;
#80292 = CARTESIAN_POINT ( 'NONE',  ( 8.099999999999923261, 12.50000000000000000, 3.918623584224382839 ) ) ;
#80293 = CARTESIAN_POINT ( 'NONE',  ( 3.099999999999945466, 12.50000000000000000, -3.983716857408426293 ) ) ;
#80295 = ORIENTED_EDGE ( 'NONE', *, *, #60956, .F. ) ;
#80294 = CARTESIAN_POINT ( 'NONE',  ( 14.59999999999989484, 2.500000000000000000, 0.09999999999999772959 ) ) ;
#80296 = ADVANCED_FACE ( 'NONE', ( #58512 ), #107404, .T. ) ;
#80297 = EDGE_CURVE ( 'NONE', #46288, #86969, #50993, .T. ) ;
#80298 = EDGE_CURVE ( 'NONE', #56576, #21325, #38218, .T. ) ;
#80299 = EDGE_CURVE ( 'NONE', #30852, #57931, #97361, .T. ) ;
#80300 = EDGE_CURVE ( 'NONE', #53342, #112224, #88596, .T. ) ;
#80301 = CIRCLE ( 'NONE', #19655, 0.1000000000000000056 ) ;
#80302 = VERTEX_POINT ( 'NONE', #29047 ) ;
#80303 = CARTESIAN_POINT ( 'NONE',  ( 14.14999999999989555, 2.500000000000000000, 2.065063509461097624 ) ) ;
#80304 = ORIENTED_EDGE ( 'NONE', *, *, #52680, .F. ) ;
#80305 = ORIENTED_EDGE ( 'NONE', *, *, #48450, .T. ) ;
#80306 = CARTESIAN_POINT ( 'NONE',  ( 8.349999999999923261, 2.500000000000000000, -6.395190528383301931 ) ) ;
#80307 = EDGE_CURVE ( 'NONE', #89533, #75765, #17944, .T. ) ;
#80308 = CARTESIAN_POINT ( 'NONE',  ( 18.98912670146724579, 2.543039972613466482, -4.488908218019479257 ) ) ;
#80309 = DIRECTION ( 'NONE',  ( 0.000000000000000000, -0.000000000000000000, 1.000000000000000000 ) ) ;
#80310 = AXIS2_PLACEMENT_3D ( 'NONE', #31264, #39163, #36731 ) ;
#80311 = DIRECTION ( 'NONE',  ( 0.000000000000000000, 0.000000000000000000, -1.000000000000000000 ) ) ;
#80312 = CIRCLE ( 'NONE', #55175, 0.1000000000000002554 ) ;
#80314 = ORIENTED_EDGE ( 'NONE', *, *, #76888, .T. ) ;
#80313 = EDGE_CURVE ( 'NONE', #115346, #70210, #34605, .T. ) ;
#80315 = DIRECTION ( 'NONE',  ( 0.000000000000000000, -0.000000000000000000, 1.000000000000000000 ) ) ;
#80316 = ORIENTED_EDGE ( 'NONE', *, *, #96378, .T. ) ;
#80317 = CARTESIAN_POINT ( 'NONE',  ( 0.8499999999999545697, 2.500000000000000000, 2.857883832488649301 ) ) ;
#80318 = CARTESIAN_POINT ( 'NONE',  ( 17.17276927100807526, 1.352216491748947202, 5.266219974090748934 ) ) ;
#80319 = CARTESIAN_POINT ( 'NONE',  ( -1.650000000000034328, 12.50000000000000000, -2.165063509461101710 ) ) ;
#80320 = ORIENTED_EDGE ( 'NONE', *, *, #58862, .F. ) ;
#80321 = AXIS2_PLACEMENT_3D ( 'NONE', #20578, #2202, #60520 ) ;
#80322 = VERTEX_POINT ( 'NONE', #55904 ) ;
#80323 = ORIENTED_EDGE ( 'NONE', *, *, #93907, .F. ) ;
#80324 = ORIENTED_EDGE ( 'NONE', *, *, #109861, .F. ) ;
#80325 = ORIENTED_EDGE ( 'NONE', *, *, #104369, .T. ) ;
#80326 = CARTESIAN_POINT ( 'NONE',  ( 11.64999999999990621, 12.50000000000000000, -2.099970236277064473 ) ) ;
#80327 = CARTESIAN_POINT ( 'NONE',  ( 12.07106445316774135, 2.500000000000126121, 8.629160867384618072 ) ) ;
#80328 = LINE ( 'NONE', #97376, #85842 ) ;
#80329 = FACE_BOUND ( 'NONE', #62043, .T. ) ;
#80330 = CARTESIAN_POINT ( 'NONE',  ( 10.59999999999990905, 2.500000000000000000, -4.083716857408426826 ) ) ;
#80331 = CARTESIAN_POINT ( 'NONE',  ( 186.4062500006828031, -8.891194145520236347, -1.633285867636356693E-15 ) ) ;
#80332 = CARTESIAN_POINT ( 'NONE',  ( 9.149999999999915090, 2.500000000000000000, -2.165063509461101710 ) ) ;
#80333 = CARTESIAN_POINT ( 'NONE',  ( -6.850000000000013856, 12.50000000000000000, 6.083687093685483660 ) ) ;
#80334 = AXIS2_PLACEMENT_3D ( 'NONE', #2708, #72118, #11889 ) ;
#80335 = AXIS2_PLACEMENT_3D ( 'NONE', #62933, #60996, #2066 ) ;
#80337 = EDGE_CURVE ( 'NONE', #76614, #23241, #6150, .T. ) ;
#80336 = DIRECTION ( 'NONE',  ( 0.000000000000000000, 0.000000000000000000, 1.000000000000000000 ) ) ;
#80338 = DIRECTION ( 'NONE',  ( 0.000000000000000000, 0.000000000000000000, -1.000000000000000000 ) ) ;
#80339 = EDGE_CURVE ( 'NONE', #82216, #28777, #17243, .T. ) ;
#80340 = DIRECTION ( 'NONE',  ( -4.274815082592931898E-19, -0.9999939076577903929, -0.003490651415223739937 ) ) ;
#80341 = EDGE_CURVE ( 'NONE', #70524, #120770, #57200, .T. ) ;
#80342 = DIRECTION ( 'NONE',  ( 0.000000000000000000, 0.000000000000000000, -1.000000000000000000 ) ) ;
#80343 = EDGE_CURVE ( 'NONE', #29645, #29366, #97123, .T. ) ;
#80344 = EDGE_LOOP ( 'NONE', ( #46247, #77960, #13223, #119661 ) ) ;
#80345 = EDGE_LOOP ( 'NONE', ( #1593, #11117 ) ) ;
#80346 = ORIENTED_EDGE ( 'NONE', *, *, #25022, .F. ) ;
#80347 = ORIENTED_EDGE ( 'NONE', *, *, #8048, .F. ) ;
#80348 = CARTESIAN_POINT ( 'NONE',  ( -11.89999999999999680, 2.500000000000000000, 0.2464101615137776757 ) ) ;
#80349 = DIRECTION ( 'NONE',  ( 0.000000000000000000, 1.000000000000000000, 0.000000000000000000 ) ) ;
#80350 = ADVANCED_FACE ( 'NONE', ( #77480 ), #99440, .T. ) ;
#80351 = FACE_BOUND ( 'NONE', #415, .T. ) ;
#80352 = DIRECTION ( 'NONE',  ( 0.000000000000000000, 0.000000000000000000, 1.000000000000000000 ) ) ;
#80353 = EDGE_CURVE ( 'NONE', #129332, #89461, #76439, .T. ) ;
#80354 = EDGE_CURVE ( 'NONE', #126313, #59594, #51904, .T. ) ;
#80355 = AXIS2_PLACEMENT_3D ( 'NONE', #19729, #119850, #60314 ) ;
#80356 = AXIS2_PLACEMENT_3D ( 'NONE', #21495, #61441, #104563 ) ;
#80358 = ORIENTED_EDGE ( 'NONE', *, *, #11310, .F. ) ;
#80357 = VECTOR ( 'NONE', #20051, 1000.000000000000000 ) ;
#80360 = CIRCLE ( 'NONE', #40666, 0.06509327318403745899 ) ;
#80359 = CARTESIAN_POINT ( 'NONE',  ( -9.600000000000006750, 2.500000000000000000, 3.637306695894644726 ) ) ;
#80361 = CARTESIAN_POINT ( 'NONE',  ( 11.89999999999990443, 2.500000000000000000, -0.3464101615137782364 ) ) ;
#80362 = DIRECTION ( 'NONE',  ( -0.000000000000000000, -1.000000000000000000, -0.000000000000000000 ) ) ;
#80363 = PLANE ( 'NONE',  #62088 ) ;
#80364 = VERTEX_POINT ( 'NONE', #121924 ) ;
#80365 = DIRECTION ( 'NONE',  ( -1.000000000000000000, -0.000000000000000000, -0.000000000000000000 ) ) ;
#80366 = EDGE_CURVE ( 'NONE', #103956, #20627, #21136, .T. ) ;
#80367 = CONICAL_SURFACE ( 'NONE', #21786, 0.1000000000000002554, 0.003490658503988666988 ) ;
#80368 = AXIS2_PLACEMENT_3D ( 'NONE', #52874, #43720, #61424 ) ;
#80369 = AXIS2_PLACEMENT_3D ( 'NONE', #32342, #102978, #35548 ) ;
#80370 = ORIENTED_EDGE ( 'NONE', *, *, #58709, .T. ) ;
#80371 = EDGE_LOOP ( 'NONE', ( #48321, #123940, #15518, #115143 ) ) ;
#80372 = FACE_OUTER_BOUND ( 'NONE', #50114, .T. ) ;
#80373 = DIRECTION ( 'NONE',  ( -0.000000000000000000, 1.000000000000000000, -0.000000000000000000 ) ) ;
#80374 = ORIENTED_EDGE ( 'NONE', *, *, #324, .F. ) ;
#80375 = VECTOR ( 'NONE', #79767, 1000.000000000000000 ) ;
#80376 = CIRCLE ( 'NONE', #944, 0.09999999999999982514 ) ;
#80377 = CARTESIAN_POINT ( 'NONE',  ( -9.800000000000007816, 2.500000000000000000, -4.083716857408422385 ) ) ;
#80378 = FACE_OUTER_BOUND ( 'NONE', #8494, .T. ) ;
#80379 = DIRECTION ( 'NONE',  ( 0.000000000000000000, 0.000000000000000000, 1.000000000000000000 ) ) ;
#80381 = EDGE_LOOP ( 'NONE', ( #93236, #46378, #73412, #88898 ) ) ;
#80380 = CONICAL_SURFACE ( 'NONE', #53198, 0.1000000000000002554, 0.003490658503988666988 ) ;
#80382 = CARTESIAN_POINT ( 'NONE',  ( 3.349999999999945466, 12.50000000000000000, -7.188010851410854052 ) ) ;
#80383 = EDGE_CURVE ( 'NONE', #127915, #47419, #111441, .T. ) ;
#80384 = VERTEX_POINT ( 'NONE', #2140 ) ;
#80385 = DIRECTION ( 'NONE',  ( 0.000000000000000000, -0.9999939076577903929, 0.003490651415223739937 ) ) ;
#80386 = VERTEX_POINT ( 'NONE', #10646 ) ;
#80387 = DIRECTION ( 'NONE',  ( 0.000000000000000000, 1.000000000000000000, 0.000000000000000000 ) ) ;
#80388 = ORIENTED_EDGE ( 'NONE', *, *, #105921, .F. ) ;
#80389 = DIRECTION ( 'NONE',  ( -0.000000000000000000, -1.000000000000000000, -0.000000000000000000 ) ) ;
#80390 = CARTESIAN_POINT ( 'NONE',  ( -2.500000000000032863, 2.500000000000000000, 5.122947341949749323 ) ) ;
#80391 =( BOUNDED_SURFACE ( )  B_SPLINE_SURFACE ( 3, 2, ( 
 ( #120429, #75191, #43175 ),
 ( #92916, #115748, #115086 ),
 ( #25423, #3237, #43818 ),
 ( #83090, #13019, #114464 ),
 ( #123007, #105297, #93542 ),
 ( #14941, #64718, #26101 ),
 ( #113172, #73256, #65353 ),
 ( #94829, #124935, #15609 ),
 ( #33358, #23503, #75822 ),
 ( #54896, #4484, #63439 ),
 ( #104636, #103369, #5149 ),
 ( #33981, #24805, #45100 ) ),
 .UNSPECIFIED., .F., .F., .F. ) 
 B_SPLINE_SURFACE_WITH_KNOTS ( ( 4, 2, 2, 2, 2, 4 ),
 ( 3, 3 ),
 ( -5.075233897202870062E-05, 0.01652955890749032222, 0.03310987015395267657, 0.04969018140041503440, 0.05798033702364620984, 0.06627049264687738528 ),
 ( 0.000000000000000000, 1.000000000000000000 ),
 .UNSPECIFIED. ) 
 GEOMETRIC_REPRESENTATION_ITEM ( )  RATIONAL_B_SPLINE_SURFACE ( (
 ( 1.000000000000000000, 1.000000000000000000, 1.000000000000000000),
 ( 1.000000000000000000, 0.9999962913217402827, 1.000000000000000000),
 ( 1.000000000000000000, 0.9967432547753130034, 1.000000000000000000),
 ( 1.000000000000000000, 0.9780629203681809880, 1.000000000000000000),
 ( 1.000000000000000000, 0.9624374449453717562, 1.000000000000000000),
 ( 1.000000000000000000, 0.9156028756800554946, 1.000000000000000000),
 ( 1.000000000000000000, 0.8842425818992938336, 1.000000000000000000),
 ( 1.000000000000000000, 0.8293059173961181418, 1.000000000000000000),
 ( 1.000000000000000000, 0.8097380764746227033, 1.000000000000000000),
 ( 1.000000000000000000, 0.7702514575415626563, 1.000000000000000000),
 ( 1.000000000000000000, 0.7503390841280456192, 1.000000000000000000),
 ( 1.000000000000000000, 0.7318752858502178826, 1.000000000000000000) ) ) 
 REPRESENTATION_ITEM ( '' )  SURFACE ( )  );
#80392 = FACE_OUTER_BOUND ( 'NONE', #127042, .T. ) ;
#80393 = FACE_OUTER_BOUND ( 'NONE', #111706, .T. ) ;
#80394 = LINE ( 'NONE', #103890, #126874 ) ;
#80395 = ORIENTED_EDGE ( 'NONE', *, *, #105424, .T. ) ;
#80396 = EDGE_LOOP ( 'NONE', ( #11591, #85669 ) ) ;
#80397 = ORIENTED_EDGE ( 'NONE', *, *, #123031, .F. ) ;
#80398 = DIRECTION ( 'NONE',  ( 0.000000000000000000, 1.000000000000000000, 0.000000000000000000 ) ) ;
#80399 = ADVANCED_FACE ( 'NONE', ( #61734 ), #20013, .T. ) ;
#80400 = DIRECTION ( 'NONE',  ( 0.000000000000000000, 1.000000000000000000, 0.000000000000000000 ) ) ;
#80401 = DIRECTION ( 'NONE',  ( 0.000000000000000000, 0.000000000000000000, -1.000000000000000000 ) ) ;
#80403 = ORIENTED_EDGE ( 'NONE', *, *, #129392, .T. ) ;
#80402 = VERTEX_POINT ( 'NONE', #81369 ) ;
#80404 = ORIENTED_EDGE ( 'NONE', *, *, #31835, .T. ) ;
#80405 = DIRECTION ( 'NONE',  ( -0.000000000000000000, -1.000000000000000000, -0.000000000000000000 ) ) ;
#80406 = CIRCLE ( 'NONE', #13475, 0.06509327318403745899 ) ;
#80407 = EDGE_LOOP ( 'NONE', ( #35932, #14022, #44577, #103972 ) ) ;
#80408 = CARTESIAN_POINT ( 'NONE',  ( 2.899999999999946620, 2.500000000000000000, -3.737306695894649700 ) ) ;
#80409 = CIRCLE ( 'NONE', #53220, 0.06509327318403745899 ) ;
#80410 = CARTESIAN_POINT ( 'NONE',  ( 10.84999999999991260, 2.500000000000000000, 7.088010851410848190 ) ) ;
#80411 = DIRECTION ( 'NONE',  ( 0.000000000000000000, -0.9999939076577903929, 0.003490651415223739937 ) ) ;
#80412 = DIRECTION ( 'NONE',  ( 0.000000000000000000, 1.000000000000000000, 0.000000000000000000 ) ) ;
#80413 = DIRECTION ( 'NONE',  ( 0.000000000000000000, 0.000000000000000000, -1.000000000000000000 ) ) ;
#80414 = CARTESIAN_POINT ( 'NONE',  ( 13.29999999999990301, 12.50000000000000000, 4.330127018922196314 ) ) ;
#80415 = EDGE_CURVE ( 'NONE', #122496, #93275, #28325, .T. ) ;
#80416 = DIRECTION ( 'NONE',  ( 0.000000000000000000, -0.9999939076577903929, 0.003490651415223739937 ) ) ;
#80417 = VERTEX_POINT ( 'NONE', #72192 ) ;
#80418 = EDGE_LOOP ( 'NONE', ( #65652, #91004 ) ) ;
#80419 = AXIS2_PLACEMENT_3D ( 'NONE', #82735, #74831, #122641 ) ;
#80420 = DIRECTION ( 'NONE',  ( -4.274815082592931898E-19, -0.9999939076577903929, -0.003490651415223739937 ) ) ;
#80422 = AXIS2_PLACEMENT_3D ( 'NONE', #106099, #4641, #66799 ) ;
#80421 = DIRECTION ( 'NONE',  ( 0.000000000000000000, 1.000000000000000000, 0.000000000000000000 ) ) ;
#80423 = ORIENTED_EDGE ( 'NONE', *, *, #100529, .F. ) ;
#80424 = ORIENTED_EDGE ( 'NONE', *, *, #72486, .T. ) ;
#80425 = CARTESIAN_POINT ( 'NONE',  ( 187.3177083336747444, 4.367472073101515306, 7.564683531250000925 ) ) ;
#80426 = CARTESIAN_POINT ( 'NONE',  ( 5.649999999999936406, 12.50000000000000000, -6.213873640053564351 ) ) ;
#80427 = FACE_OUTER_BOUND ( 'NONE', #88912, .T. ) ;
#80428 = CARTESIAN_POINT ( 'NONE',  ( 4.599999999999940137, 2.500000000000000000, -5.022947341949754119 ) ) ;
#80429 = CIRCLE ( 'NONE', #126388, 0.1000000000000002554 ) ;
#80430 = DIRECTION ( 'NONE',  ( 0.000000000000000000, 0.000000000000000000, 1.000000000000000000 ) ) ;
#80431 = CIRCLE ( 'NONE', #55289, 0.06509327318403745899 ) ;
#80432 = CARTESIAN_POINT ( 'NONE',  ( 5.449999999999936229, 12.50000000000000000, 6.495190528383297135 ) ) ;
#80433 = FACE_OUTER_BOUND ( 'NONE', #32297, .T. ) ;
#80434 = CIRCLE ( 'NONE', #99216, 0.1000000000000000056 ) ;
#80435 = CARTESIAN_POINT ( 'NONE',  ( 10.84999999999991260, 2.500000000000000000, 6.595190528383296780 ) ) ;
#80436 = EDGE_LOOP ( 'NONE', ( #64690, #72580 ) ) ;
#80437 = ORIENTED_EDGE ( 'NONE', *, *, #104937, .T. ) ;
#80438 = EDGE_CURVE ( 'NONE', #89530, #121486, #36739, .T. ) ;
#80439 = ORIENTED_EDGE ( 'NONE', *, *, #25209, .F. ) ;
#80440 = VERTEX_POINT ( 'NONE', #21805 ) ;
#80441 = ORIENTED_EDGE ( 'NONE', *, *, #30355, .T. ) ;
#80442 = DIRECTION ( 'NONE',  ( 0.000000000000000000, -0.000000000000000000, 1.000000000000000000 ) ) ;
#80443 = CARTESIAN_POINT ( 'NONE',  ( 2.899999999999944844, 12.50000000000000000, 3.702399969078682407 ) ) ;
#80444 = ADVANCED_FACE ( 'NONE', ( #20509 ), #40960, .T. ) ;
#80445 = ORIENTED_EDGE ( 'NONE', *, *, #53577, .F. ) ;
#80446 = CARTESIAN_POINT ( 'NONE',  ( 11.89999999999990798, 2.500000000000000000, 3.983716857408420964 ) ) ;
#80447 = CARTESIAN_POINT ( 'NONE',  ( 6.699999999999930012, 2.500000000000000000, 4.330127018922196314 ) ) ;
#80448 = AXIS2_PLACEMENT_3D ( 'NONE', #41165, #20214, #19565 ) ;
#80449 = CONICAL_SURFACE ( 'NONE', #34486, 0.1000000000000002554, 0.003490658503988666988 ) ;
#80450 = CARTESIAN_POINT ( 'NONE',  ( 12.49999999999990230, 2.500000000000000000, -0.5928203230275541635 ) ) ;
#80452 = ORIENTED_EDGE ( 'NONE', *, *, #100391, .T. ) ;
#80451 = DIRECTION ( 'NONE',  ( -0.000000000000000000, 1.000000000000000000, -0.000000000000000000 ) ) ;
#80453 = AXIS2_PLACEMENT_3D ( 'NONE', #14059, #24546, #95869 ) ;
#80454 = ADVANCED_FACE ( 'NONE', ( #70248 ), #119335, .T. ) ;
#80455 = CONICAL_SURFACE ( 'NONE', #34489, 0.1000000000000002554, 0.003490658503988666988 ) ;
#80456 = EDGE_CURVE ( 'NONE', #84030, #60931, #59148, .T. ) ;
#80457 = EDGE_CURVE ( 'NONE', #85577, #70277, #7471, .T. ) ;
#80458 = DIRECTION ( 'NONE',  ( 0.000000000000000000, 1.000000000000000000, 0.000000000000000000 ) ) ;
#80459 = EDGE_CURVE ( 'NONE', #62448, #59275, #126624, .T. ) ;
#80460 = FACE_OUTER_BOUND ( 'NONE', #9023, .T. ) ;
#80461 = ORIENTED_EDGE ( 'NONE', *, *, #23445, .F. ) ;
#80462 = AXIS2_PLACEMENT_3D ( 'NONE', #120654, #101007, #41473 ) ;
#80463 = CONICAL_SURFACE ( 'NONE', #28310, 0.09999999999999982514, 0.003490658503988666988 ) ;
#80464 = CONICAL_SURFACE ( 'NONE', #32455, 0.09999999999999982514, 0.003490658503988666988 ) ;
#80465 = EDGE_CURVE ( 'NONE', #93446, #60636, #86891, .T. ) ;
#80466 = VERTEX_POINT ( 'NONE', #59814 ) ;
#80468 = ORIENTED_EDGE ( 'NONE', *, *, #46757, .T. ) ;
#80467 = EDGE_CURVE ( 'NONE', #97708, #93625, #11588, .T. ) ;
#80469 = EDGE_LOOP ( 'NONE', ( #16822, #115106 ) ) ;
#80470 = FACE_OUTER_BOUND ( 'NONE', #57915, .T. ) ;
#80471 = CONICAL_SURFACE ( 'NONE', #78417, 0.1000000000000002554, 0.003490658503988666988 ) ;
#80472 = ADVANCED_FACE ( 'NONE', ( #120633 ), #120363, .T. ) ;
#80473 = DIRECTION ( 'NONE',  ( 0.000000000000000000, -0.9999939076577903929, 0.003490651415223739937 ) ) ;
#80474 = DIRECTION ( 'NONE',  ( 0.000000000000000000, 0.000000000000000000, 1.000000000000000000 ) ) ;
#80475 = EDGE_CURVE ( 'NONE', #72217, #74701, #45061, .T. ) ;
#80476 = AXIS2_PLACEMENT_3D ( 'NONE', #115007, #56095, #33269 ) ;
#80477 = AXIS2_PLACEMENT_3D ( 'NONE', #55249, #45431, #55876 ) ;
#80478 = ADVANCED_FACE ( 'NONE', ( #119994 ), #110176, .T. ) ;
#80480 = CIRCLE ( 'NONE', #40776, 0.09999999999999982514 ) ;
#80479 = CARTESIAN_POINT ( 'NONE',  ( 3.749999999999942268, 2.500000000000000000, -1.372243186433550033 ) ) ;
#80481 = EDGE_LOOP ( 'NONE', ( #286, #40010, #47270, #127189 ) ) ;
#80482 = CARTESIAN_POINT ( 'NONE',  ( -5.650000000000019895, 2.500000000000000000, 6.148780366869520009 ) ) ;
#80483 = CARTESIAN_POINT ( 'NONE',  ( 16.86635082839119804, -0.4716143926291150867, -5.778906370536186721 ) ) ;
#80484 = CARTESIAN_POINT ( 'NONE',  ( 4.349999999999941025, 12.50000000000000000, -6.213873640053564351 ) ) ;
#80485 = DIRECTION ( 'NONE',  ( -0.000000000000000000, -1.000000000000000000, -0.000000000000000000 ) ) ;
#80486 = EDGE_CURVE ( 'NONE', #97220, #86499, #33386, .T. ) ;
#80487 = ORIENTED_EDGE ( 'NONE', *, *, #86348, .T. ) ;
#80488 = DIRECTION ( 'NONE',  ( -0.000000000000000000, -1.000000000000000000, -0.000000000000000000 ) ) ;
#80489 = EDGE_LOOP ( 'NONE', ( #116284, #124517 ) ) ;
#80490 = ORIENTED_EDGE ( 'NONE', *, *, #109078, .T. ) ;
#80491 = DIRECTION ( 'NONE',  ( 0.000000000000000000, 1.000000000000000000, 0.000000000000000000 ) ) ;
#80492 = DIRECTION ( 'NONE',  ( -0.000000000000000000, 1.000000000000000000, -0.000000000000000000 ) ) ;
#80493 = FACE_BOUND ( 'NONE', #120042, .T. ) ;
#80494 = CARTESIAN_POINT ( 'NONE',  ( -14.54999999999998472, 2.500000000000000000, -2.165063509461099489 ) ) ;
#80495 = DIRECTION ( 'NONE',  ( -0.000000000000000000, 1.000000000000000000, -0.000000000000000000 ) ) ;
#80496 = DIRECTION ( 'NONE',  ( -4.274815082592931898E-19, -0.9999939076577903929, -0.003490651415223739937 ) ) ;
#80498 = ADVANCED_FACE ( 'NONE', ( #34198 ), #45307, .T. ) ;
#80497 = CARTESIAN_POINT ( 'NONE',  ( 9.149999999999918643, 12.50000000000000000, -6.560283801567339701 ) ) ;
#80499 = CARTESIAN_POINT ( 'NONE',  ( 11.84999999999990372, 12.50000000000000000, -6.906693963081115939 ) ) ;
#80500 = DIRECTION ( 'NONE',  ( 0.000000000000000000, -0.000000000000000000, 1.000000000000000000 ) ) ;
#80501 = CARTESIAN_POINT ( 'NONE',  ( 12.29999999999990479, 2.500000000000000000, -3.883716857408426648 ) ) ;
#80502 = VERTEX_POINT ( 'NONE', #104840 ) ;
#80503 = AXIS2_PLACEMENT_3D ( 'NONE', #54876, #46347, #115073 ) ;
#80504 = DIRECTION ( 'NONE',  ( 0.000000000000000000, 0.000000000000000000, -1.000000000000000000 ) ) ;
#80505 = CARTESIAN_POINT ( 'NONE',  ( -6.250000000000015987, 2.500000000000000000, 1.572243186433545548 ) ) ;
#80506 = ORIENTED_EDGE ( 'NONE', *, *, #101028, .T. ) ;
#80507 = VERTEX_POINT ( 'NONE', #74119 ) ;
#80508 = DIRECTION ( 'NONE',  ( -0.000000000000000000, 1.000000000000000000, -0.000000000000000000 ) ) ;
#80509 = DIRECTION ( 'NONE',  ( 0.000000000000000000, 1.000000000000000000, 0.000000000000000000 ) ) ;
#80510 = FACE_BOUND ( 'NONE', #27716, .T. ) ;
#80511 = DIRECTION ( 'NONE',  ( 0.000000000000000000, 0.000000000000000000, -1.000000000000000000 ) ) ;
#80512 = CIRCLE ( 'NONE', #59688, 0.1000000000000002554 ) ;
#80513 = EDGE_CURVE ( 'NONE', #15869, #46460, #94381, .T. ) ;
#80514 = CARTESIAN_POINT ( 'NONE',  ( -10.40000000000000213, 2.500000000000000000, -4.330127018922197202 ) ) ;
#80516 = EDGE_CURVE ( 'NONE', #91809, #21509, #91104, .T. ) ;
#80515 = CIRCLE ( 'NONE', #13585, 0.06509327318403745899 ) ;
#80517 = ORIENTED_EDGE ( 'NONE', *, *, #112839, .F. ) ;
#80518 = CARTESIAN_POINT ( 'NONE',  ( -2.700000000000029932, 2.500000000000000000, -4.776537180435977525 ) ) ;
#80519 = ORIENTED_EDGE ( 'NONE', *, *, #15701, .F. ) ;
#80520 = DIRECTION ( 'NONE',  ( 0.000000000000000000, 0.000000000000000000, 1.000000000000000000 ) ) ;
#80521 = DIRECTION ( 'NONE',  ( 0.000000000000000000, -0.000000000000000000, 1.000000000000000000 ) ) ;
#80522 = EDGE_CURVE ( 'NONE', #40128, #96204, #12595, .T. ) ;
#80523 = VECTOR ( 'NONE', #78254, 1000.000000000000000 ) ;
#80524 = CIRCLE ( 'NONE', #42888, 0.06509327318403745899 ) ;
#80525 = DIRECTION ( 'NONE',  ( 0.000000000000000000, 0.000000000000000000, 1.000000000000000000 ) ) ;
#80526 = PLANE ( 'NONE',  #19596 ) ;
#80527 = ORIENTED_EDGE ( 'NONE', *, *, #95401, .T. ) ;
#80528 = CARTESIAN_POINT ( 'NONE',  ( 4.349999999999936584, 2.500000000000000000, 6.148780366869520009 ) ) ;
#80529 = DIRECTION ( 'NONE',  ( 0.000000000000000000, -0.000000000000000000, 1.000000000000000000 ) ) ;
#80530 = CARTESIAN_POINT ( 'NONE',  ( 184.7812500006828031, 0.000000000000000000, 7.700000000000000178 ) ) ;
#80531 = VERTEX_POINT ( 'NONE', #64282 ) ;
#80532 = EDGE_LOOP ( 'NONE', ( #60952, #67515, #118479, #76620 ) ) ;
#80533 = DIRECTION ( 'NONE',  ( 0.000000000000000000, 0.000000000000000000, 1.000000000000000000 ) ) ;
#80534 = EDGE_LOOP ( 'NONE', ( #90847, #116106, #81724, #102793 ) ) ;
#80535 = CARTESIAN_POINT ( 'NONE',  ( 11.89999999999990443, 12.50000000000000000, 0.2813168883297362810 ) ) ;
#80536 = CARTESIAN_POINT ( 'NONE',  ( 87.50000000000000000, -7.402262750143061787, 1.385127402881718650 ) ) ;
#80538 = DIRECTION ( 'NONE',  ( -0.000000000000000000, 1.000000000000000000, -0.000000000000000000 ) ) ;
#80537 = AXIS2_PLACEMENT_3D ( 'NONE', #82791, #104345, #93884 ) ;
#80539 = EDGE_LOOP ( 'NONE', ( #53310, #10048 ) ) ;
#80540 = CIRCLE ( 'NONE', #68002, 0.1000000000000002554 ) ;
#80541 = DIRECTION ( 'NONE',  ( -4.274815082592931898E-19, -0.9999939076577903929, -0.003490651415223739937 ) ) ;
#80542 = DIRECTION ( 'NONE',  ( 0.000000000000000000, 0.000000000000000000, -1.000000000000000000 ) ) ;
#80543 = CARTESIAN_POINT ( 'NONE',  ( -9.999999999999971578, 2.500000000000000000, -4.330127018922197202 ) ) ;
#80544 = CIRCLE ( 'NONE', #120252, 0.06509327318403745899 ) ;
#80545 = DIRECTION ( 'NONE',  ( 0.000000000000000000, -0.9999939076577903929, 0.003490651415223739937 ) ) ;
#80546 = CARTESIAN_POINT ( 'NONE',  ( 3.349999999999942801, 12.50000000000000000, 2.857883832488649301 ) ) ;
#80547 = CARTESIAN_POINT ( 'NONE',  ( -0.8500000000000386136, 12.50000000000000000, 5.867463478539781896 ) ) ;
#80548 = ORIENTED_EDGE ( 'NONE', *, *, #3207, .F. ) ;
#80549 = ORIENTED_EDGE ( 'NONE', *, *, #38814, .F. ) ;
#80551 = CARTESIAN_POINT ( 'NONE',  ( 10.84999999999991260, 2.500000000000000000, -1.472243186433550122 ) ) ;
#80550 = VECTOR ( 'NONE', #81393, 1000.000000000000000 ) ;
#80552 = VERTEX_POINT ( 'NONE', #53821 ) ;
#80553 = CARTESIAN_POINT ( 'NONE',  ( 104.9453507214960695, 6.600323588196552294, 3.971150466560552150 ) ) ;
#80556 = ORIENTED_EDGE ( 'NONE', *, *, #63013, .T. ) ;
#80555 = ORIENTED_EDGE ( 'NONE', *, *, #110778, .F. ) ;
#80554 = AXIS2_PLACEMENT_3D ( 'NONE', #26521, #86059, #17310 ) ;
#80557 = ORIENTED_EDGE ( 'NONE', *, *, #127023, .T. ) ;
#80558 = CARTESIAN_POINT ( 'NONE',  ( -5.650000000000023448, 12.50000000000000000, -6.148780366869526226 ) ) ;
#80560 = CONICAL_SURFACE ( 'NONE', #26264, 0.1000000000000000472, 0.003490658503988666988 ) ;
#80559 = FACE_OUTER_BOUND ( 'NONE', #49302, .T. ) ;
#80561 = DIRECTION ( 'NONE',  ( 0.000000000000000000, -0.000000000000000000, 1.000000000000000000 ) ) ;
#80562 =( LENGTH_UNIT ( ) NAMED_UNIT ( * ) SI_UNIT ( .MILLI., .METRE. ) );
#80563 = LINE ( 'NONE', #90355, #109979 ) ;
#80564 = CARTESIAN_POINT ( 'NONE',  ( 0.000000000000000000, -2.500000000000000000, 0.000000000000000000 ) ) ;
#80565 = DIRECTION ( 'NONE',  ( 0.000000000000000000, 0.000000000000000000, -1.000000000000000000 ) ) ;
#80566 = AXIS2_PLACEMENT_3D ( 'NONE', #117929, #7974, #87815 ) ;
#80567 = EDGE_CURVE ( 'NONE', #62966, #82761, #49265, .T. ) ;
#80568 = FACE_OUTER_BOUND ( 'NONE', #77953, .T. ) ;
#80569 = DIRECTION ( 'NONE',  ( -4.274815082592931898E-19, -0.9999939076577903929, -0.003490651415223739937 ) ) ;
#80570 = ADVANCED_FACE ( 'NONE', ( #104209 ), #95227, .T. ) ;
#80571 = DIRECTION ( 'NONE',  ( 0.000000000000000000, 1.000000000000000000, 0.000000000000000000 ) ) ;
#80572 = ORIENTED_EDGE ( 'NONE', *, *, #111809, .F. ) ;
#80573 = CARTESIAN_POINT ( 'NONE',  ( 8.099999999999923261, 2.500000000000000000, -3.983716857408426293 ) ) ;
#80574 = VERTEX_POINT ( 'NONE', #102914 ) ;
#80575 = ADVANCED_FACE ( 'NONE', ( #13234 ), #122420, .T. ) ;
#80576 = VERTEX_POINT ( 'NONE', #2788 ) ;
#80577 = CARTESIAN_POINT ( 'NONE',  ( 9.349999999999916156, 2.500000000000000000, -1.918653347947326004 ) ) ;
#80578 = AXIS2_PLACEMENT_3D ( 'NONE', #62962, #93713, #91779 ) ;
#80579 = DIRECTION ( 'NONE',  ( -4.274815082592931898E-19, -0.9999939076577903929, -0.003490651415223739937 ) ) ;
#80580 = CARTESIAN_POINT ( 'NONE',  ( 3.749999999999942268, 12.50000000000000000, -1.537336459617587581 ) ) ;
#80581 = CARTESIAN_POINT ( 'NONE',  ( 13.74999999999989519, 2.500000000000000000, -2.857883832488653741 ) ) ;
#80582 = CARTESIAN_POINT ( 'NONE',  ( -11.84999999999999787, 12.50000000000000000, -1.818653347947321919 ) ) ;
#80583 = DIRECTION ( 'NONE',  ( 0.000000000000000000, -0.9999939076577903929, 0.003490651415223739937 ) ) ;
#80584 = ORIENTED_EDGE ( 'NONE', *, *, #25745, .T. ) ;
#80585 = AXIS2_PLACEMENT_3D ( 'NONE', #90480, #72161, #100326 ) ;
#80586 = CIRCLE ( 'NONE', #118228, 0.1000000000000000056 ) ;
#80587 = CIRCLE ( 'NONE', #111885, 0.06509327318403745899 ) ;
#80588 = ORIENTED_EDGE ( 'NONE', *, *, #25019, .T. ) ;
#80589 = DIRECTION ( 'NONE',  ( 0.000000000000000000, 1.000000000000000000, 0.000000000000000000 ) ) ;
#80590 = ORIENTED_EDGE ( 'NONE', *, *, #19892, .T. ) ;
#80592 = EDGE_CURVE ( 'NONE', #28605, #59465, #65968, .T. ) ;
#80591 = DIRECTION ( 'NONE',  ( -0.000000000000000000, -1.000000000000000000, -0.000000000000000000 ) ) ;
#80593 = ORIENTED_EDGE ( 'NONE', *, *, #119017, .T. ) ;
#80594 = ORIENTED_EDGE ( 'NONE', *, *, #58775, .F. ) ;
#80595 = DIRECTION ( 'NONE',  ( 0.000000000000000000, 0.000000000000000000, 1.000000000000000000 ) ) ;
#80596 = LINE ( 'NONE', #79937, #12931 ) ;
#80597 = CIRCLE ( 'NONE', #3316, 0.1000000000000002554 ) ;
#80598 = EDGE_CURVE ( 'NONE', #57867, #68264, #32546, .T. ) ;
#80599 = DIRECTION ( 'NONE',  ( 1.000000000000000000, 0.000000000000000000, 0.000000000000000000 ) ) ;
#80600 = CARTESIAN_POINT ( 'NONE',  ( -11.25000000000000000, 12.50000000000000000, 7.188010851410848723 ) ) ;
#80601 = CARTESIAN_POINT ( 'NONE',  ( 10.59999999999990905, 2.500000000000000000, -4.776537180435978414 ) ) ;
#80602 = ORIENTED_EDGE ( 'NONE', *, *, #34209, .F. ) ;
#80603 = CARTESIAN_POINT ( 'NONE',  ( -6.850000000000013856, 12.50000000000000000, 1.818653347947321475 ) ) ;
#80604 = DIRECTION ( 'NONE',  ( -0.000000000000000000, -1.000000000000000000, -0.000000000000000000 ) ) ;
#80605 = ADVANCED_FACE ( 'NONE', ( #102288 ), #3367, .T. ) ;
#80606 = EDGE_CURVE ( 'NONE', #124839, #30668, #58385, .T. ) ;
#80607 = DIRECTION ( 'NONE',  ( 0.000000000000000000, -0.000000000000000000, 1.000000000000000000 ) ) ;
#80608 = EDGE_CURVE ( 'NONE', #106259, #5504, #38912, .T. ) ;
#80609 = DIRECTION ( 'NONE',  ( 0.000000000000000000, 1.000000000000000000, 0.000000000000000000 ) ) ;
#80610 = ADVANCED_FACE ( 'NONE', ( #43381 ), #99525, .T. ) ;
#80611 = CARTESIAN_POINT ( 'NONE',  ( 1.049999999999952971, 12.50000000000000000, 6.148780366869520897 ) ) ;
#80612 = ORIENTED_EDGE ( 'NONE', *, *, #25929, .T. ) ;
#80613 = CIRCLE ( 'NONE', #24166, 0.06509327318403745899 ) ;
#80614 = ORIENTED_EDGE ( 'NONE', *, *, #129330, .T. ) ;
#80615 = ADVANCED_FACE ( 'NONE', ( #97611 ), #7554, .T. ) ;
#80616 = DIRECTION ( 'NONE',  ( 0.000000000000000000, 0.000000000000000000, 1.000000000000000000 ) ) ;
#80617 = EDGE_CURVE ( 'NONE', #63390, #79899, #28421, .T. ) ;
#80618 = EDGE_LOOP ( 'NONE', ( #118321, #100585 ) ) ;
#80619 = CARTESIAN_POINT ( 'NONE',  ( -8.950000000000011724, 12.50000000000000000, -6.148780366869520897 ) ) ;
#80620 = CARTESIAN_POINT ( 'NONE',  ( -11.84999999999999609, 2.500000000000000000, 1.818653347947321475 ) ) ;
#80621 = EDGE_CURVE ( 'NONE', #5812, #90572, #128389, .T. ) ;
#80622 = ADVANCED_FACE ( 'NONE', ( #116598 ), #107918, .T. ) ;
#80623 = AXIS2_PLACEMENT_3D ( 'NONE', #40472, #29999, #10961 ) ;
#80624 = ORIENTED_EDGE ( 'NONE', *, *, #11569, .T. ) ;
#80625 = CARTESIAN_POINT ( 'NONE',  ( 4.799999999999935874, 2.500000000000000000, 3.983716857408420964 ) ) ;
#80626 = DIRECTION ( 'NONE',  ( 0.000000000000000000, 0.000000000000000000, 1.000000000000000000 ) ) ;
#80627 = EDGE_CURVE ( 'NONE', #87583, #120916, #47884, .T. ) ;
#80628 = DIRECTION ( 'NONE',  ( -0.000000000000000000, 1.000000000000000000, -0.000000000000000000 ) ) ;
#80629 = CIRCLE ( 'NONE', #40936, 0.06509327318403745899 ) ;
#80630 = CARTESIAN_POINT ( 'NONE',  ( -1.250000000000001554, 12.50000000000000000, 2.165063509461097713 ) ) ;
#80631 = EDGE_CURVE ( 'NONE', #92009, #15907, #43112, .T. ) ;
#80632 = AXIS2_PLACEMENT_3D ( 'NONE', #7415, #25777, #66973 ) ;
#80633 = DIRECTION ( 'NONE',  ( 0.000000000000000000, 1.000000000000000000, 0.000000000000000000 ) ) ;
#80634 = CIRCLE ( 'NONE', #57643, 0.1000000000000000472 ) ;
#80635 = VERTEX_POINT ( 'NONE', #88424 ) ;
#80636 = CARTESIAN_POINT ( 'NONE',  ( 65.40766660093524365, 3.109053433052308968, -5.794607793964218878 ) ) ;
#80637 = FACE_OUTER_BOUND ( 'NONE', #21451, .T. ) ;
#80638 = CARTESIAN_POINT ( 'NONE',  ( -4.550000000000022915, 2.500000000000000000, -2.265063509461101798 ) ) ;
#80639 = AXIS2_PLACEMENT_3D ( 'NONE', #75257, #123080, #74618 ) ;
#80640 = DIRECTION ( 'NONE',  ( 0.000000000000000000, 1.000000000000000000, 0.000000000000000000 ) ) ;
#80641 = EDGE_LOOP ( 'NONE', ( #98403, #69549, #87789, #54203 ) ) ;
#80642 = CONICAL_SURFACE ( 'NONE', #66050, 0.09999999999999982514, 0.003490658503988666988 ) ;
#80643 = EDGE_LOOP ( 'NONE', ( #18876, #117490 ) ) ;
#80644 = CARTESIAN_POINT ( 'NONE',  ( -2.050000000000033129, 2.500000000000000000, 6.395190528383296602 ) ) ;
#80645 = CARTESIAN_POINT ( 'NONE',  ( -2.300000000000032685, 12.50000000000000000, -4.676537180435978769 ) ) ;
#80646 = DIRECTION ( 'NONE',  ( -0.000000000000000000, -1.000000000000000000, -0.000000000000000000 ) ) ;
#80647 = ORIENTED_EDGE ( 'NONE', *, *, #101309, .F. ) ;
#80648 = CONICAL_SURFACE ( 'NONE', #22174, 0.1000000000000000472, 0.003490658503988666988 ) ;
#80649 = AXIS2_PLACEMENT_3D ( 'NONE', #96934, #24980, #95019 ) ;
#80650 = CARTESIAN_POINT ( 'NONE',  ( -4.350000000000023626, 2.500000000000000000, -2.511473670974877948 ) ) ;
#80651 = AXIS2_PLACEMENT_3D ( 'NONE', #1492, #49984, #71522 ) ;
#80652 = FACE_OUTER_BOUND ( 'NONE', #97430, .T. ) ;
#80653 = CIRCLE ( 'NONE', #24217, 0.1000000000000002554 ) ;
#80654 = ORIENTED_EDGE ( 'NONE', *, *, #65212, .F. ) ;
#80655 = CARTESIAN_POINT ( 'NONE',  ( 9.149999999999920419, 2.500000000000000000, 1.372243186433545370 ) ) ;
#80656 = EDGE_LOOP ( 'NONE', ( #79798, #69104, #61715, #104642 ) ) ;
#80657 = FACE_OUTER_BOUND ( 'NONE', #98162, .T. ) ;
#80658 = EDGE_CURVE ( 'NONE', #113873, #59573, #30579, .T. ) ;
#80659 = ORIENTED_EDGE ( 'NONE', *, *, #78409, .F. ) ;
#80660 = CARTESIAN_POINT ( 'NONE',  ( 1.249999999999986899, 2.500000000000000000, 6.495190528383297135 ) ) ;
#80661 = CARTESIAN_POINT ( 'NONE',  ( 12.89999999999990266, 2.500000000000000000, -3.637306695894650055 ) ) ;
#80662 = EDGE_CURVE ( 'NONE', #28046, #34246, #78602, .T. ) ;
#80663 = ORIENTED_EDGE ( 'NONE', *, *, #75879, .F. ) ;
#80664 = VERTEX_POINT ( 'NONE', #76688 ) ;
#80665 = CARTESIAN_POINT ( 'NONE',  ( 187.4218750003414016, 0.000000000000000000, 7.564683531250000925 ) ) ;
#80666 = CARTESIAN_POINT ( 'NONE',  ( -2.100000000000033396, 2.500000000000000000, 0.7928203230275495672 ) ) ;
#80667 = AXIS2_PLACEMENT_3D ( 'NONE', #123641, #32731, #34000 ) ;
#80668 = ORIENTED_EDGE ( 'NONE', *, *, #54109, .T. ) ;
#80669 = DIRECTION ( 'NONE',  ( 0.000000000000000000, 0.000000000000000000, -1.000000000000000000 ) ) ;
#80670 = LINE ( 'NONE', #20454, #93222 ) ;
#80671 = DIRECTION ( 'NONE',  ( 0.000000000000000000, 0.000000000000000000, 1.000000000000000000 ) ) ;
#80672 = CARTESIAN_POINT ( 'NONE',  ( 104.9394650928313553, 7.745629575256785415, 3.967022963969182747 ) ) ;
#80673 = DIRECTION ( 'NONE',  ( 0.000000000000000000, 1.000000000000000000, 0.000000000000000000 ) ) ;
#80674 = CARTESIAN_POINT ( 'NONE',  ( 14.14999999999989555, 2.500000000000000000, 2.165063509461097713 ) ) ;
#80675 = AXIS2_PLACEMENT_3D ( 'NONE', #117848, #109987, #91627 ) ;
#80676 = CARTESIAN_POINT ( 'NONE',  ( 1.649999999999951950, 2.500000000000000000, -7.288010851410854585 ) ) ;
#80677 = CIRCLE ( 'NONE', #9656, 0.06509327318403743123 ) ;
#80678 = AXIS2_PLACEMENT_3D ( 'NONE', #71007, #112863, #61183 ) ;
#80679 = ORIENTED_EDGE ( 'NONE', *, *, #63162, .T. ) ;
#80680 = AXIS2_PLACEMENT_3D ( 'NONE', #21576, #111219, #9178 ) ;
#80681 = VERTEX_POINT ( 'NONE', #27562 ) ;
#80682 = CARTESIAN_POINT ( 'NONE',  ( -2.500000000000030642, 12.50000000000000000, -4.957854068765716882 ) ) ;
#80683 = ORIENTED_EDGE ( 'NONE', *, *, #113973, .F. ) ;
#80684 = DIRECTION ( 'NONE',  ( 0.000000000000000000, 0.000000000000000000, 1.000000000000000000 ) ) ;
#80685 = CARTESIAN_POINT ( 'NONE',  ( 7.499999999999923617, 12.50000000000000000, 0.6928203230275494784 ) ) ;
#80686 = CARTESIAN_POINT ( 'NONE',  ( 8.099999999999923261, 12.50000000000000000, -3.983716857408426293 ) ) ;
#80688 = ORIENTED_EDGE ( 'NONE', *, *, #68777, .F. ) ;
#80687 = EDGE_LOOP ( 'NONE', ( #14375, #118799 ) ) ;
#80689 = FACE_BOUND ( 'NONE', #107883, .T. ) ;
#80690 = ORIENTED_EDGE ( 'NONE', *, *, #88253, .T. ) ;
#80691 = DIRECTION ( 'NONE',  ( 0.000000000000000000, 0.000000000000000000, 1.000000000000000000 ) ) ;
#80692 = CARTESIAN_POINT ( 'NONE',  ( 4.799999999999934097, 12.50000000000000000, 4.676537180435972552 ) ) ;
#80693 = CIRCLE ( 'NONE', #72380, 0.1000000000000002554 ) ;
#80694 = CARTESIAN_POINT ( 'NONE',  ( 7.299999999999927880, 12.50000000000000000, 3.918623584224383727 ) ) ;
#80695 = LINE ( 'NONE', #126063, #120400 ) ;
#80696 = CARTESIAN_POINT ( 'NONE',  ( 1.249999999999952038, 2.500000000000000000, 2.957883832488649389 ) ) ;
#80698 = VECTOR ( 'NONE', #72164, 1000.000000000000000 ) ;
#80697 = VECTOR ( 'NONE', #129029, 1000.000000000000000 ) ;
#80699 = DIRECTION ( 'NONE',  ( 0.000000000000000000, 1.000000000000000000, 0.000000000000000000 ) ) ;
#80700 = PLANE ( 'NONE',  #79000 ) ;
#80701 = DIRECTION ( 'NONE',  ( 0.000000000000000000, -0.000000000000000000, 1.000000000000000000 ) ) ;
#80702 = CARTESIAN_POINT ( 'NONE',  ( -11.64999999999999680, 12.50000000000000000, 2.230156782645134950 ) ) ;
#80703 = CARTESIAN_POINT ( 'NONE',  ( 2.499999999999947153, 2.500000000000000000, 0.7928203230275495672 ) ) ;
#80704 = EDGE_CURVE ( 'NONE', #87465, #11458, #49366, .T. ) ;
#80705 = AXIS2_PLACEMENT_3D ( 'NONE', #7888, #109315, #9187 ) ;
#80706 = ORIENTED_EDGE ( 'NONE', *, *, #127596, .F. ) ;
#80707 = ORIENTED_EDGE ( 'NONE', *, *, #70117, .F. ) ;
#80708 = AXIS2_PLACEMENT_3D ( 'NONE', #66822, #17720, #28860 ) ;
#80709 = ORIENTED_EDGE ( 'NONE', *, *, #24281, .F. ) ;
#80710 = ORIENTED_EDGE ( 'NONE', *, *, #15109, .T. ) ;
#80711 = CARTESIAN_POINT ( 'NONE',  ( -3.950000000000029932, 12.50000000000000000, -6.213873640053564351 ) ) ;
#80712 = PLANE ( 'NONE',  #105120 ) ;
#80714 = EDGE_LOOP ( 'NONE', ( #33195, #39070, #97402, #88980 ) ) ;
#80713 = ORIENTED_EDGE ( 'NONE', *, *, #18824, .T. ) ;
#80715 = ORIENTED_EDGE ( 'NONE', *, *, #107933, .T. ) ;
#80716 = CARTESIAN_POINT ( 'NONE',  ( -6.850000000000017408, 2.500000000000000000, -6.941600689897077459 ) ) ;
#80717 = LINE ( 'NONE', #19860, #82243 ) ;
#80718 = DIRECTION ( 'NONE',  ( 1.000000000000000000, 0.000000000000000000, 0.000000000000000000 ) ) ;
#80719 = DIRECTION ( 'NONE',  ( -0.000000000000000000, 1.000000000000000000, -0.000000000000000000 ) ) ;
#80720 = DIRECTION ( 'NONE',  ( -0.000000000000000000, 1.000000000000000000, -0.000000000000000000 ) ) ;
#80721 = CARTESIAN_POINT ( 'NONE',  ( -8.100000000000013856, 2.500000000000000000, 0.4464101615137736623 ) ) ;
#80722 = ADVANCED_FACE ( 'NONE', ( #107433 ), #68104, .T. ) ;
#80723 = DIRECTION ( 'NONE',  ( 0.000000000000000000, 0.000000000000000000, 1.000000000000000000 ) ) ;
#80724 = EDGE_CURVE ( 'NONE', #42654, #47060, #103731, .T. ) ;
#80725 = ORIENTED_EDGE ( 'NONE', *, *, #25902, .F. ) ;
#80726 = DIRECTION ( 'NONE',  ( -4.274815082592931898E-19, -0.9999939076577903929, -0.003490651415223739937 ) ) ;
#80727 = VERTEX_POINT ( 'NONE', #17750 ) ;
#80728 = VERTEX_POINT ( 'NONE', #66853 ) ;
#80729 = EDGE_LOOP ( 'NONE', ( #62047, #120173, #26895, #78808 ) ) ;
#80730 = AXIS2_PLACEMENT_3D ( 'NONE', #87179, #27608, #59029 ) ;
#80731 = DIRECTION ( 'NONE',  ( -0.000000000000000000, -1.000000000000000000, -0.000000000000000000 ) ) ;
#80732 = VERTEX_POINT ( 'NONE', #18408 ) ;
#80733 = ADVANCED_FACE ( 'NONE', ( #58353 ), #98249, .T. ) ;
#80734 = ORIENTED_EDGE ( 'NONE', *, *, #95102, .T. ) ;
#80735 = ORIENTED_EDGE ( 'NONE', *, *, #103325, .T. ) ;
#80736 = DIRECTION ( 'NONE',  ( 0.000000000000000000, 0.000000000000000000, 1.000000000000000000 ) ) ;
#80738 = AXIS2_PLACEMENT_3D ( 'NONE', #52162, #120892, #80342 ) ;
#80737 = AXIS2_PLACEMENT_3D ( 'NONE', #23278, #103135, #114244 ) ;
#80739 = CARTESIAN_POINT ( 'NONE',  ( -10.85000000000000142, 2.500000000000000000, -7.088010851410849966 ) ) ;
#80740 = CARTESIAN_POINT ( 'NONE',  ( 15.79999999999989058, 12.50000000000000000, -0.06509327318403980434 ) ) ;
#80741 = DIRECTION ( 'NONE',  ( 0.000000000000000000, 0.000000000000000000, 1.000000000000000000 ) ) ;
#80742 = DIRECTION ( 'NONE',  ( 0.000000000000000000, 0.000000000000000000, 1.000000000000000000 ) ) ;
#80743 = FACE_OUTER_BOUND ( 'NONE', #66331, .T. ) ;
#80744 = LINE ( 'NONE', #72216, #32537 ) ;
#80745 = AXIS2_PLACEMENT_3D ( 'NONE', #17122, #57076, #47281 ) ;
#80746 = EDGE_LOOP ( 'NONE', ( #42570, #98278, #85720, #124773 ) ) ;
#80747 = DIRECTION ( 'NONE',  ( 0.000000000000000000, -0.9999939076577903929, 0.003490651415223739937 ) ) ;
#80748 = CIRCLE ( 'NONE', #105774, 0.06509327318403745899 ) ;
#80749 = EDGE_LOOP ( 'NONE', ( #34361, #117140, #39058, #27305 ) ) ;
#80750 = CARTESIAN_POINT ( 'NONE',  ( 112.7324313128099220, 8.548364151789236587, -1.646368127929983327 ) ) ;
#80751 = CARTESIAN_POINT ( 'NONE',  ( 9.999999999999912959, 2.500000000000000000, -5.022947341949754119 ) ) ;
#80752 = VERTEX_POINT ( 'NONE', #75380 ) ;
#80753 = CARTESIAN_POINT ( 'NONE',  ( -0.2000000000000412836, 2.500000000000000000, 4.576537180435972019 ) ) ;
#80754 = DIRECTION ( 'NONE',  ( 0.000000000000000000, 0.000000000000000000, 1.000000000000000000 ) ) ;
#80755 = ORIENTED_EDGE ( 'NONE', *, *, #13761, .T. ) ;
#80756 = EDGE_CURVE ( 'NONE', #117090, #125178, #115287, .T. ) ;
#80757 = DIRECTION ( 'NONE',  ( 0.000000000000000000, 0.000000000000000000, 1.000000000000000000 ) ) ;
#80758 = EDGE_LOOP ( 'NONE', ( #7215, #60704 ) ) ;
#80759 = EDGE_LOOP ( 'NONE', ( #96679, #90592 ) ) ;
#80760 = CARTESIAN_POINT ( 'NONE',  ( 8.099999999999923261, 12.50000000000000000, -3.918623584224389056 ) ) ;
#80761 = FACE_OUTER_BOUND ( 'NONE', #67045, .T. ) ;
#80762 = ADVANCED_FACE ( 'NONE', ( #66209 ), #95310, .T. ) ;
#80763 = CARTESIAN_POINT ( 'NONE',  ( 184.6302083336747444, -4.367472073101514418, -7.564683531250002702 ) ) ;
#80764 = CONICAL_SURFACE ( 'NONE', #24313, 0.1000000000000002554, 0.003490658503988666988 ) ;
#80765 = CARTESIAN_POINT ( 'NONE',  ( -7.100000000000017408, 2.500000000000000000, -0.5928203230275542746 ) ) ;
#80766 = ADVANCED_FACE ( 'NONE', ( #106146 ), #66057, .T. ) ;
#80767 = DIRECTION ( 'NONE',  ( 0.000000000000000000, 0.000000000000000000, -1.000000000000000000 ) ) ;
#80768 = EDGE_LOOP ( 'NONE', ( #34359, #9867, #104490, #60666 ) ) ;
#80769 = AXIS2_PLACEMENT_3D ( 'NONE', #123385, #103757, #82180 ) ;
#80770 = DIRECTION ( 'NONE',  ( -0.000000000000000000, 1.000000000000000000, -0.000000000000000000 ) ) ;
#80771 = EDGE_CURVE ( 'NONE', #66014, #27399, #76536, .T. ) ;
#80772 = EDGE_CURVE ( 'NONE', #53677, #125527, #80563, .T. ) ;
#80773 = AXIS2_PLACEMENT_3D ( 'NONE', #117686, #37236, #56830 ) ;
#80774 = ADVANCED_FACE ( 'NONE', ( #60296 ), #39367, .T. ) ;
#80775 = CIRCLE ( 'NONE', #24323, 0.1000000000000002554 ) ;
#80776 = ADVANCED_FACE ( 'NONE', ( #129037 ), #114188, .T. ) ;
#80777 = VERTEX_POINT ( 'NONE', #100198 ) ;
#80778 = CONICAL_SURFACE ( 'NONE', #112161, 0.1000000000000002554, 0.003490658503988666988 ) ;
#80779 = CARTESIAN_POINT ( 'NONE',  ( -9.600000000000006750, 2.500000000000000000, 0.7928203230275495672 ) ) ;
#80780 = DIRECTION ( 'NONE',  ( 0.000000000000000000, 0.000000000000000000, 1.000000000000000000 ) ) ;
#80781 = AXIS2_PLACEMENT_3D ( 'NONE', #75185, #26099, #5775 ) ;
#80782 = EDGE_CURVE ( 'NONE', #53598, #115977, #19033, .T. ) ;
#80783 = CARTESIAN_POINT ( 'NONE',  ( 187.3802083336747444, 4.367472073101515306, 7.564683531250000925 ) ) ;
#80784 = DIRECTION ( 'NONE',  ( 1.000000000000000000, -0.000000000000000000, -0.000000000000000000 ) ) ;
#80785 = PLANE ( 'NONE',  #109156 ) ;
#80786 = CARTESIAN_POINT ( 'NONE',  ( -13.94999999999998685, 2.500000000000000000, 1.818653347947325472 ) ) ;
#80787 = FACE_OUTER_BOUND ( 'NONE', #11312, .T. ) ;
#80788 = EDGE_LOOP ( 'NONE', ( #64155, #54567, #85894, #127516 ) ) ;
#80789 = EDGE_CURVE ( 'NONE', #82278, #49764, #107827, .T. ) ;
#80790 = AXIS2_PLACEMENT_3D ( 'NONE', #93519, #92213, #21555 ) ;
#80791 = DIRECTION ( 'NONE',  ( 0.000000000000000000, 1.000000000000000000, 0.000000000000000000 ) ) ;
#80793 = AXIS2_PLACEMENT_3D ( 'NONE', #85822, #35461, #117193 ) ;
#80792 = AXIS2_PLACEMENT_3D ( 'NONE', #115122, #25464, #105339 ) ;
#80794 = CARTESIAN_POINT ( 'NONE',  ( 179.5000000000000000, 1.375000000000000000, 7.634788798650556707 ) ) ;
#80795 = CARTESIAN_POINT ( 'NONE',  ( -11.84999999999999609, 12.50000000000000000, 6.841600689897072485 ) ) ;
#80796 = EDGE_LOOP ( 'NONE', ( #89681, #19259 ) ) ;
#80797 = DIRECTION ( 'NONE',  ( 0.000000000000000000, 0.000000000000000000, 1.000000000000000000 ) ) ;
#80798 = ORIENTED_EDGE ( 'NONE', *, *, #15547, .T. ) ;
#80799 = ORIENTED_EDGE ( 'NONE', *, *, #5238, .T. ) ;
#80800 = DIRECTION ( 'NONE',  ( 0.000000000000000000, 0.000000000000000000, -1.000000000000000000 ) ) ;
#80801 = ORIENTED_EDGE ( 'NONE', *, *, #94895, .F. ) ;
#80802 = CARTESIAN_POINT ( 'NONE',  ( 17.34645602449680979, -0.4686430837605670696, -5.377443133682146659 ) ) ;
#80803 = DIRECTION ( 'NONE',  ( -0.000000000000000000, -1.000000000000000000, -0.000000000000000000 ) ) ;
#80804 = LINE ( 'NONE', #120715, #15070 ) ;
#80805 = ORIENTED_EDGE ( 'NONE', *, *, #55309, .T. ) ;
#80806 = DIRECTION ( 'NONE',  ( 0.000000000000000000, 0.000000000000000000, 1.000000000000000000 ) ) ;
#80807 = LINE ( 'NONE', #73537, #93463 ) ;
#80808 = FACE_OUTER_BOUND ( 'NONE', #7173, .T. ) ;
#80809 = ORIENTED_EDGE ( 'NONE', *, *, #13179, .F. ) ;
#80810 = AXIS2_PLACEMENT_3D ( 'NONE', #30815, #91641, #81810 ) ;
#80812 = ORIENTED_EDGE ( 'NONE', *, *, #55045, .F. ) ;
#80811 = EDGE_CURVE ( 'NONE', #59946, #65442, #79280, .T. ) ;
#80813 = CIRCLE ( 'NONE', #78771, 0.09999999999999982514 ) ;
#80814 = ORIENTED_EDGE ( 'NONE', *, *, #23932, .F. ) ;
#80815 = DIRECTION ( 'NONE',  ( 0.000000000000000000, 1.000000000000000000, 0.000000000000000000 ) ) ;
#80816 = CARTESIAN_POINT ( 'NONE',  ( 1.649999999999951505, 12.50000000000000000, 2.857883832488649301 ) ) ;
#80817 = CARTESIAN_POINT ( 'NONE',  ( -0.6000000000000383915, 2.500000000000000000, -4.083716857408426826 ) ) ;
#80818 = FACE_BOUND ( 'NONE', #52177, .T. ) ;
#80819 = EDGE_LOOP ( 'NONE', ( #125721, #22857, #82020, #114047 ) ) ;
#80820 = DIRECTION ( 'NONE',  ( 0.000000000000000000, 1.000000000000000000, 0.000000000000000000 ) ) ;
#80821 = DIRECTION ( 'NONE',  ( 0.000000000000000000, 0.000000000000000000, -1.000000000000000000 ) ) ;
#80822 = EDGE_LOOP ( 'NONE', ( #76189, #120503, #2200, #49705 ) ) ;
#80824 = VECTOR ( 'NONE', #73716, 1000.000000000000000 ) ;
#80823 = CIRCLE ( 'NONE', #26443, 0.06509327318403743123 ) ;
#80825 = ADVANCED_FACE ( 'NONE', ( #91020 ), #119190, .T. ) ;
#80826 = CARTESIAN_POINT ( 'NONE',  ( 5.199999999999937117, 2.500000000000000000, -4.576537180435978236 ) ) ;
#80827 = DIRECTION ( 'NONE',  ( 0.000000000000000000, 1.000000000000000000, 0.000000000000000000 ) ) ;
#80828 = CARTESIAN_POINT ( 'NONE',  ( 3.099999999999944134, 12.50000000000000000, 4.611443907251934426 ) ) ;
#80829 = DIRECTION ( 'NONE',  ( 0.000000000000000000, 0.000000000000000000, 1.000000000000000000 ) ) ;
#80830 = DIRECTION ( 'NONE',  ( 0.000000000000000000, 1.000000000000000000, 0.000000000000000000 ) ) ;
#80831 = CARTESIAN_POINT ( 'NONE',  ( 11.64999999999990798, 12.50000000000000000, 5.802370205355744659 ) ) ;
#80832 = DIRECTION ( 'NONE',  ( 0.000000000000000000, -0.9999939076577903929, 0.003490651415223739937 ) ) ;
#80834 = AXIS2_PLACEMENT_3D ( 'NONE', #21726, #22384, #72755 ) ;
#80833 = AXIS2_PLACEMENT_3D ( 'NONE', #40698, #120525, #70773 ) ;
#80835 = CONICAL_SURFACE ( 'NONE', #99617, 0.1000000000000002554, 0.003490658503988666988 ) ;
#80836 = VERTEX_POINT ( 'NONE', #51743 ) ;
#80837 = EDGE_LOOP ( 'NONE', ( #78446, #123944 ) ) ;
#80838 = ORIENTED_EDGE ( 'NONE', *, *, #75507, .F. ) ;
#80839 = ORIENTED_EDGE ( 'NONE', *, *, #55756, .F. ) ;
#80840 = CARTESIAN_POINT ( 'NONE',  ( -4.119968255444916849E-14, 2.500000000000000000, 3.737306695894644371 ) ) ;
#80841 = CARTESIAN_POINT ( 'NONE',  ( 1.849999999999950573, 2.500000000000000000, -1.718653347947326049 ) ) ;
#80842 = ORIENTED_EDGE ( 'NONE', *, *, #16341, .F. ) ;
#80843 = FACE_BOUND ( 'NONE', #46351, .T. ) ;
#80844 = DIRECTION ( 'NONE',  ( -0.000000000000000000, 1.000000000000000000, -0.000000000000000000 ) ) ;
#80845 = LINE ( 'NONE', #67263, #99336 ) ;
#80846 = DIRECTION ( 'NONE',  ( 0.000000000000000000, 0.000000000000000000, -1.000000000000000000 ) ) ;
#80847 = CARTESIAN_POINT ( 'NONE',  ( 5.799999999999931433, 12.50000000000000000, 4.265033745738159077 ) ) ;
#80848 = CARTESIAN_POINT ( 'NONE',  ( 4.399999999999937295, 2.500000000000000000, 3.983716857408420964 ) ) ;
#80849 = CARTESIAN_POINT ( 'NONE',  ( -10.40000000000000213, 2.500000000000000000, 0.6928203230275494784 ) ) ;
#80850 = CARTESIAN_POINT ( 'NONE',  ( -6.850000000000013856, 2.500000000000000000, 6.148780366869520897 ) ) ;
#80851 = DIRECTION ( 'NONE',  ( 0.000000000000000000, -0.9999939076577903929, 0.003490651415223739937 ) ) ;
#80853 = EDGE_LOOP ( 'NONE', ( #80439, #105472, #29543, #73069 ) ) ;
#80852 = CIRCLE ( 'NONE', #45352, 0.1000000000000000056 ) ;
#80854 = AXIS2_PLACEMENT_3D ( 'NONE', #77463, #38192, #28376 ) ;
#80855 = EDGE_LOOP ( 'NONE', ( #58067, #15281, #7814, #117340 ) ) ;
#80856 = EDGE_CURVE ( 'NONE', #25999, #102068, #80748, .T. ) ;
#80857 = VERTEX_POINT ( 'NONE', #120478 ) ;
#80859 = EDGE_LOOP ( 'NONE', ( #70849, #1810 ) ) ;
#80858 = AXIS2_PLACEMENT_3D ( 'NONE', #35088, #14751, #114903 ) ;
#80860 = ORIENTED_EDGE ( 'NONE', *, *, #24749, .T. ) ;
#80861 = ORIENTED_EDGE ( 'NONE', *, *, #41474, .F. ) ;
#80862 = DIRECTION ( 'NONE',  ( -0.000000000000000000, -1.000000000000000000, -0.000000000000000000 ) ) ;
#80863 = ORIENTED_EDGE ( 'NONE', *, *, #112943, .F. ) ;
#80864 = VECTOR ( 'NONE', #118984, 1000.000000000000000 ) ;
#80865 = ADVANCED_FACE ( 'NONE', ( #119829 ), #41047, .T. ) ;
#80866 = CIRCLE ( 'NONE', #57884, 0.1000000000000002554 ) ;
#80867 = CARTESIAN_POINT ( 'NONE',  ( 19.09982477502542153, 0.5559300837585670063, 4.454172625795878027 ) ) ;
#80868 = CARTESIAN_POINT ( 'NONE',  ( 183.9427083336747160, -6.551208109652278289, 3.782341765624995134 ) ) ;
#80869 = DIRECTION ( 'NONE',  ( 0.000000000000000000, 1.000000000000000000, 0.000000000000000000 ) ) ;
#80870 = DIRECTION ( 'NONE',  ( -0.000000000000000000, -1.000000000000000000, -0.000000000000000000 ) ) ;
#80871 = EDGE_CURVE ( 'NONE', #53276, #117920, #91201, .T. ) ;
#80872 = AXIS2_PLACEMENT_3D ( 'NONE', #128375, #38715, #78628 ) ;
#80873 = EDGE_CURVE ( 'NONE', #122009, #123754, #60905, .T. ) ;
#80874 = VERTEX_POINT ( 'NONE', #100817 ) ;
#80875 = LINE ( 'NONE', #2955, #86051 ) ;
#80876 = VECTOR ( 'NONE', #111714, 1000.000000000000000 ) ;
#80877 = ORIENTED_EDGE ( 'NONE', *, *, #42194, .T. ) ;
#80879 = CIRCLE ( 'NONE', #97585, 0.1000000000000002554 ) ;
#80878 = AXIS2_PLACEMENT_3D ( 'NONE', #27909, #59981, #58028 ) ;
#80880 = ORIENTED_EDGE ( 'NONE', *, *, #92235, .F. ) ;
#80881 = DIRECTION ( 'NONE',  ( 0.000000000000000000, -0.000000000000000000, 1.000000000000000000 ) ) ;
#80882 = ADVANCED_FACE ( 'NONE', ( #31461 ), #112038, .T. ) ;
#80883 = DIRECTION ( 'NONE',  ( 0.000000000000000000, 0.000000000000000000, 1.000000000000000000 ) ) ;
#80884 = CARTESIAN_POINT ( 'NONE',  ( -3.550000000000030909, 2.500000000000000000, -6.841600689897078702 ) ) ;
#80885 = ADVANCED_FACE ( 'NONE', ( #38728 ), #7649, .T. ) ;
#80886 = ORIENTED_EDGE ( 'NONE', *, *, #52059, .T. ) ;
#80887 = VERTEX_POINT ( 'NONE', #98897 ) ;
#80888 = FACE_OUTER_BOUND ( 'NONE', #15686, .T. ) ;
#80889 = DIRECTION ( 'NONE',  ( 0.000000000000000000, 1.000000000000000000, 0.000000000000000000 ) ) ;
#80890 = DIRECTION ( 'NONE',  ( 0.000000000000000000, 0.000000000000000000, 1.000000000000000000 ) ) ;
#80891 = PLANE ( 'NONE',  #23177 ) ;
#80892 = VERTEX_POINT ( 'NONE', #11804 ) ;
#80893 = DIRECTION ( 'NONE',  ( 0.000000000000000000, 1.000000000000000000, 0.000000000000000000 ) ) ;
#80894 = CIRCLE ( 'NONE', #18176, 0.06509327318403745899 ) ;
#80895 = ORIENTED_EDGE ( 'NONE', *, *, #66068, .T. ) ;
#80896 = CARTESIAN_POINT ( 'NONE',  ( 12.31005523242778210, -2.500000000000000000, 7.488833079370801116 ) ) ;
#80897 = EDGE_LOOP ( 'NONE', ( #77468, #91275, #69978, #27575 ) ) ;
#80898 = DIRECTION ( 'NONE',  ( 0.000000000000000000, 1.000000000000000000, 0.000000000000000000 ) ) ;
#80899 = CARTESIAN_POINT ( 'NONE',  ( -5.600000000000020073, 12.50000000000000000, 0.3464101615137736845 ) ) ;
#80900 = DIRECTION ( 'NONE',  ( 0.000000000000000000, 1.000000000000000000, 0.000000000000000000 ) ) ;
#80901 = CARTESIAN_POINT ( 'NONE',  ( 184.7812500006828031, 0.000000000000000000, 7.700000000000000178 ) ) ;
#80902 = ORIENTED_EDGE ( 'NONE', *, *, #121985, .T. ) ;
#80903 = DIRECTION ( 'NONE',  ( 0.000000000000000000, 1.000000000000000000, 0.000000000000000000 ) ) ;
#80904 = AXIS2_PLACEMENT_3D ( 'NONE', #20171, #60119, #100027 ) ;
#80905 = FACE_OUTER_BOUND ( 'NONE', #6228, .T. ) ;
#80906 = ORIENTED_EDGE ( 'NONE', *, *, #86209, .F. ) ;
#80907 = ORIENTED_EDGE ( 'NONE', *, *, #81198, .F. ) ;
#80908 = ORIENTED_EDGE ( 'NONE', *, *, #108092, .F. ) ;
#80909 = CARTESIAN_POINT ( 'NONE',  ( 17.50000000000000000, 2.750000000000000000, 4.000000000000001776 ) ) ;
#80910 = DIRECTION ( 'NONE',  ( -0.000000000000000000, 1.000000000000000000, -0.000000000000000000 ) ) ;
#80911 = CARTESIAN_POINT ( 'NONE',  ( -1.250000000000001554, 2.500000000000000000, 2.165063509461097713 ) ) ;
#80912 = DIRECTION ( 'NONE',  ( -0.000000000000000000, -1.000000000000000000, -0.000000000000000000 ) ) ;
#80913 = DIRECTION ( 'NONE',  ( 0.000000000000000000, 0.000000000000000000, 1.000000000000000000 ) ) ;
#80917 = ADVANCED_FACE ( 'NONE', ( #89090 ), #112138, .T. ) ;
#80916 = AXIS2_PLACEMENT_3D ( 'NONE', #50338, #117761, #9767 ) ;
#80915 = DIRECTION ( 'NONE',  ( 0.000000000000000000, 1.000000000000000000, 0.000000000000000000 ) ) ;
#80914 = AXIS2_PLACEMENT_3D ( 'NONE', #5890, #106684, #16979 ) ;
#80918 = CARTESIAN_POINT ( 'NONE',  ( 5.199999999999937117, 2.500000000000000000, -4.576537180435978236 ) ) ;
#80919 = CARTESIAN_POINT ( 'NONE',  ( -3.950000000000026379, 2.500000000000000000, 2.511473670974873507 ) ) ;
#80920 = LINE ( 'NONE', #59362, #90249 ) ;
#80921 = EDGE_CURVE ( 'NONE', #59130, #102506, #34882, .T. ) ;
#80922 = EDGE_CURVE ( 'NONE', #74443, #19888, #103813, .T. ) ;
#80923 = EDGE_CURVE ( 'NONE', #95802, #87020, #121755, .T. ) ;
#80926 = EDGE_CURVE ( 'NONE', #51891, #251, #61959, .T. ) ;
#80925 = CONICAL_SURFACE ( 'NONE', #34879, 0.09999999999999999167, 0.003490658503988666988 ) ;
#80924 = AXIS2_PLACEMENT_3D ( 'NONE', #97335, #125026, #79629 ) ;
#80927 = CONICAL_SURFACE ( 'NONE', #24481, 0.1000000000000002554, 0.003490658503988666988 ) ;
#80928 = ORIENTED_EDGE ( 'NONE', *, *, #48427, .T. ) ;
#80929 = ADVANCED_FACE ( 'NONE', ( #13075 ), #93347, .T. ) ;
#80930 = CARTESIAN_POINT ( 'NONE',  ( -14.59999999999998366, 12.50000000000000000, 0.7579135962115892688 ) ) ;
#80931 = DIRECTION ( 'NONE',  ( 0.000000000000000000, 0.000000000000000000, -1.000000000000000000 ) ) ;
#80932 = DIRECTION ( 'NONE',  ( -0.000000000000000000, -1.000000000000000000, -0.000000000000000000 ) ) ;
#80933 = CARTESIAN_POINT ( 'NONE',  ( 12.29999999999990656, 2.500000000000000000, 3.983716857408420964 ) ) ;
#80934 = ORIENTED_EDGE ( 'NONE', *, *, #113089, .F. ) ;
#80935 = EDGE_CURVE ( 'NONE', #76431, #18475, #74560, .T. ) ;
#80936 = CARTESIAN_POINT ( 'NONE',  ( 4.599999999999937472, 12.50000000000000000, 0.6928203230275494784 ) ) ;
#80937 = ADVANCED_FACE ( 'NONE', ( #24214 ), #76624, .T. ) ;
#80938 = CARTESIAN_POINT ( 'NONE',  ( 0.7999999999999612976, 2.500000000000000000, -1.084202172485504434E-16 ) ) ;
#80940 = ORIENTED_EDGE ( 'NONE', *, *, #125424, .T. ) ;
#80939 = CARTESIAN_POINT ( 'NONE',  ( 10.59999999999990905, 12.50000000000000000, -4.611443907251940644 ) ) ;
#80941 = CONICAL_SURFACE ( 'NONE', #66258, 0.09999999999999982514, 0.003490658503988666988 ) ;
#80942 = ORIENTED_EDGE ( 'NONE', *, *, #58402, .F. ) ;
#80943 = AXIS2_PLACEMENT_3D ( 'NONE', #62350, #102269, #83277 ) ;
#80944 = DIRECTION ( 'NONE',  ( 0.000000000000000000, -0.000000000000000000, 1.000000000000000000 ) ) ;
#80945 = AXIS2_PLACEMENT_3D ( 'NONE', #123928, #6080, #34936 ) ;
#80946 = ORIENTED_EDGE ( 'NONE', *, *, #59790, .F. ) ;
#80947 = ORIENTED_EDGE ( 'NONE', *, *, #54703, .T. ) ;
#80948 = CARTESIAN_POINT ( 'NONE',  ( 9.549999999999918998, 12.50000000000000000, 2.230156782645134950 ) ) ;
#80949 = CONICAL_SURFACE ( 'NONE', #16165, 0.09999999999999982514, 0.003490658503988666988 ) ;
#80950 = CARTESIAN_POINT ( 'NONE',  ( -6.450000000000016165, 2.500000000000000000, 2.411473670974873862 ) ) ;
#80951 = CARTESIAN_POINT ( 'NONE',  ( -13.94999999999998863, 2.500000000000000000, -1.818653347947323917 ) ) ;
#80952 = AXIS2_PLACEMENT_3D ( 'NONE', #7573, #84855, #96590 ) ;
#80953 = CARTESIAN_POINT ( 'NONE',  ( -1.850000000000033396, 12.50000000000000000, -6.083687093685488989 ) ) ;
#80954 = EDGE_LOOP ( 'NONE', ( #84605, #79176, #50967, #84896 ) ) ;
#80955 = AXIS2_PLACEMENT_3D ( 'NONE', #28792, #18306, #96212 ) ;
#80956 = EDGE_LOOP ( 'NONE', ( #49635, #95773, #43916, #101938 ) ) ;
#80957 = CARTESIAN_POINT ( 'NONE',  ( -2.700000000000030820, 2.500000000000000000, 0.3464101615137735735 ) ) ;
#80958 = AXIS2_PLACEMENT_3D ( 'NONE', #82976, #82330, #122257 ) ;
#80959 = DIRECTION ( 'NONE',  ( 0.000000000000000000, 0.000000000000000000, -1.000000000000000000 ) ) ;
#80960 = ORIENTED_EDGE ( 'NONE', *, *, #17474, .F. ) ;
#80962 = VECTOR ( 'NONE', #122871, 1000.000000000000000 ) ;
#80961 = CIRCLE ( 'NONE', #41266, 0.09999999999999982514 ) ;
#80963 = ORIENTED_EDGE ( 'NONE', *, *, #16702, .T. ) ;
#80964 = ORIENTED_EDGE ( 'NONE', *, *, #75133, .T. ) ;
#80965 = ORIENTED_EDGE ( 'NONE', *, *, #59636, .T. ) ;
#80966 = CARTESIAN_POINT ( 'NONE',  ( -7.499999999999980460, 2.500000000000000000, -2.276824562219559311E-15 ) ) ;
#80967 = CARTESIAN_POINT ( 'NONE',  ( 8.512291507236481536, 2.500000000000128786, 9.502944100472571876 ) ) ;
#80968 = PLANE ( 'NONE',  #92193 ) ;
#80969 = FACE_BOUND ( 'NONE', #10592, .T. ) ;
#80970 = CARTESIAN_POINT ( 'NONE',  ( 10.39999999999991331, 2.500000000000000000, 0.09999999999999761857 ) ) ;
#80971 = CARTESIAN_POINT ( 'NONE',  ( 184.2812500006828031, 0.000000000000000000, 7.700000000000000178 ) ) ;
#80972 = FACE_OUTER_BOUND ( 'NONE', #53203, .T. ) ;
#80973 = LINE ( 'NONE', #109787, #119066 ) ;
#80974 = ADVANCED_FACE ( 'NONE', ( #53031 ), #102128, .T. ) ;
#80975 = CARTESIAN_POINT ( 'NONE',  ( -2.300000000000033573, 12.50000000000000000, -3.983716857408426293 ) ) ;
#80976 = DIRECTION ( 'NONE',  ( -0.000000000000000000, 1.000000000000000000, -0.000000000000000000 ) ) ;
#80977 = AXIS2_PLACEMENT_3D ( 'NONE', #107519, #108789, #7369 ) ;
#80978 = DIRECTION ( 'NONE',  ( 0.000000000000000000, 0.000000000000000000, 1.000000000000000000 ) ) ;
#80979 = CARTESIAN_POINT ( 'NONE',  ( 12.04999999999990834, 2.500000000000000000, -2.165063509461101710 ) ) ;
#80980 = EDGE_LOOP ( 'NONE', ( #101789, #57926 ) ) ;
#80981 = ORIENTED_EDGE ( 'NONE', *, *, #53530, .F. ) ;
#80982 = VERTEX_POINT ( 'NONE', #103419 ) ;
#80983 = ORIENTED_EDGE ( 'NONE', *, *, #47093, .T. ) ;
#80984 = EDGE_LOOP ( 'NONE', ( #61228, #119171 ) ) ;
#80985 = DIRECTION ( 'NONE',  ( 0.000000000000000000, 0.000000000000000000, -1.000000000000000000 ) ) ;
#80986 = DIRECTION ( 'NONE',  ( 0.000000000000000000, 0.000000000000000000, 1.000000000000000000 ) ) ;
#80987 = ORIENTED_EDGE ( 'NONE', *, *, #69851, .F. ) ;
#80988 = FACE_BOUND ( 'NONE', #115279, .T. ) ;
#80989 = DIRECTION ( 'NONE',  ( 0.000000000000000000, -0.000000000000000000, 1.000000000000000000 ) ) ;
#80990 = CIRCLE ( 'NONE', #112389, 0.06509327318403745899 ) ;
#80991 = VECTOR ( 'NONE', #97034, 1000.000000000000000 ) ;
#80992 = ORIENTED_EDGE ( 'NONE', *, *, #30980, .T. ) ;
#80993 = FACE_OUTER_BOUND ( 'NONE', #6608, .T. ) ;
#80994 = LINE ( 'NONE', #111741, #7589 ) ;
#80995 = DIRECTION ( 'NONE',  ( 0.000000000000000000, -0.9999939076577903929, 0.003490651415223739937 ) ) ;
#80996 = CARTESIAN_POINT ( 'NONE',  ( 7.499999999999961808, 2.500000000000000000, -4.330127018922201643 ) ) ;
#80997 = ORIENTED_EDGE ( 'NONE', *, *, #118585, .F. ) ;
#80998 = LINE ( 'NONE', #71170, #103591 ) ;
#81000 = AXIS2_PLACEMENT_3D ( 'NONE', #34584, #74487, #65291 ) ;
#80999 = AXIS2_PLACEMENT_3D ( 'NONE', #18151, #69844, #109769 ) ;
#81001 = AXIS2_PLACEMENT_3D ( 'NONE', #70894, #2790, #100359 ) ;
#81002 = ORIENTED_EDGE ( 'NONE', *, *, #54265, .T. ) ;
#81003 = VERTEX_POINT ( 'NONE', #13728 ) ;
#81004 = CARTESIAN_POINT ( 'NONE',  ( 2.699999999999944666, 2.500000000000000000, 4.676537180435972552 ) ) ;
#81005 = DIRECTION ( 'NONE',  ( 0.000000000000000000, 1.000000000000000000, 0.000000000000000000 ) ) ;
#81006 = VERTEX_POINT ( 'NONE', #92294 ) ;
#81007 = DIRECTION ( 'NONE',  ( 0.000000000000000000, 0.000000000000000000, 1.000000000000000000 ) ) ;
#81008 = CONICAL_SURFACE ( 'NONE', #64087, 0.1000000000000000472, 0.003490658503988666988 ) ;
#81010 = EDGE_CURVE ( 'NONE', #115678, #13172, #114509, .T. ) ;
#81009 = AXIS2_PLACEMENT_3D ( 'NONE', #21099, #52491, #9998 ) ;
#81011 = CARTESIAN_POINT ( 'NONE',  ( 7.099999999999928590, 2.500000000000000000, 4.330127018922196314 ) ) ;
#81012 = CARTESIAN_POINT ( 'NONE',  ( -12.29999999999999716, 12.50000000000000000, -3.983716857408423628 ) ) ;
#81013 = CARTESIAN_POINT ( 'NONE',  ( -9.400000000000007461, 12.50000000000000000, 4.676537180435972552 ) ) ;
#81014 = ORIENTED_EDGE ( 'NONE', *, *, #73987, .F. ) ;
#81015 = ADVANCED_FACE ( 'NONE', ( #82500 ), #122421, .T. ) ;
#81016 = CARTESIAN_POINT ( 'NONE',  ( 12.49999999999990408, 2.500000000000000000, 5.022947341949748790 ) ) ;
#81017 = ADVANCED_FACE ( 'NONE', ( #44487 ), #18118, .T. ) ;
#81018 = VERTEX_POINT ( 'NONE', #3918 ) ;
#81019 = DIRECTION ( 'NONE',  ( 0.000000000000000000, 1.000000000000000000, 0.000000000000000000 ) ) ;
#81020 = VECTOR ( 'NONE', #11885, 1000.000000000000000 ) ;
#81021 = ORIENTED_EDGE ( 'NONE', *, *, #11035, .T. ) ;
#81022 = CARTESIAN_POINT ( 'NONE',  ( -4.200000000000029488, 12.50000000000000000, -4.265033745738164406 ) ) ;
#81023 = ORIENTED_EDGE ( 'NONE', *, *, #111947, .F. ) ;
#81024 = CARTESIAN_POINT ( 'NONE',  ( -7.900000000000011013, 2.500000000000000000, 4.330127018922196314 ) ) ;
#81025 = CIRCLE ( 'NONE', #49737, 0.06509327318403745899 ) ;
#81026 = DIRECTION ( 'NONE',  ( 0.000000000000000000, 1.000000000000000000, 0.000000000000000000 ) ) ;
#81027 = ADVANCED_FACE ( 'NONE', ( #81826 ), #43869, .T. ) ;
#81028 = EDGE_CURVE ( 'NONE', #58821, #94262, #11767, .T. ) ;
#81029 = DIRECTION ( 'NONE',  ( 0.000000000000000000, 1.000000000000000000, 0.000000000000000000 ) ) ;
#81030 = EDGE_CURVE ( 'NONE', #42019, #87160, #28509, .T. ) ;
#81031 = CARTESIAN_POINT ( 'NONE',  ( 10.39999999999991331, 12.50000000000000000, -2.385244779468109755E-15 ) ) ;
#81032 = EDGE_CURVE ( 'NONE', #67345, #49421, #34031, .T. ) ;
#81033 = EDGE_CURVE ( 'NONE', #127662, #66202, #104059, .T. ) ;
#81035 = AXIS2_PLACEMENT_3D ( 'NONE', #96142, #45125, #74575 ) ;
#81034 = CARTESIAN_POINT ( 'NONE',  ( -7.499999999999976907, 2.500000000000000000, 4.330127018922196314 ) ) ;
#81036 = VERTEX_POINT ( 'NONE', #72672 ) ;
#81037 = AXIS2_PLACEMENT_3D ( 'NONE', #39973, #79886, #70073 ) ;
#81038 = ORIENTED_EDGE ( 'NONE', *, *, #32070, .F. ) ;
#81039 = EDGE_LOOP ( 'NONE', ( #84751, #12909 ) ) ;
#81040 = PLANE ( 'NONE',  #3588 ) ;
#81041 = AXIS2_PLACEMENT_3D ( 'NONE', #108926, #8156, #77541 ) ;
#81042 = PLANE ( 'NONE',  #107967 ) ;
#81043 = DIRECTION ( 'NONE',  ( 0.000000000000000000, 1.000000000000000000, 0.000000000000000000 ) ) ;
#81045 = VERTEX_POINT ( 'NONE', #23561 ) ;
#81044 = VERTEX_POINT ( 'NONE', #104685 ) ;
#81046 = VERTEX_POINT ( 'NONE', #32115 ) ;
#81047 = ADVANCED_FACE ( 'NONE', ( #72033 ), #22300, .T. ) ;
#81048 = DIRECTION ( 'NONE',  ( -4.274815082592931898E-19, -0.9999939076577903929, -0.003490651415223739937 ) ) ;
#81049 = VECTOR ( 'NONE', #35614, 1000.000000000000000 ) ;
#81050 = CIRCLE ( 'NONE', #24602, 0.1000000000000000472 ) ;
#81051 = ORIENTED_EDGE ( 'NONE', *, *, #128051, .T. ) ;
#81052 = CARTESIAN_POINT ( 'NONE',  ( 10.84999999999990905, 2.500000000000000000, 2.165063509461097713 ) ) ;
#81053 = DIRECTION ( 'NONE',  ( 0.000000000000000000, 0.000000000000000000, -1.000000000000000000 ) ) ;
#81054 = DIRECTION ( 'NONE',  ( 0.000000000000000000, 1.000000000000000000, 0.000000000000000000 ) ) ;
#81055 = DIRECTION ( 'NONE',  ( -1.000000000000000000, -0.000000000000000000, -0.000000000000000000 ) ) ;
#81056 = CARTESIAN_POINT ( 'NONE',  ( 11.89999999999990798, 2.500000000000000000, 4.776537180435972196 ) ) ;
#81057 = DIRECTION ( 'NONE',  ( 0.000000000000000000, 0.000000000000000000, -1.000000000000000000 ) ) ;
#81058 = CARTESIAN_POINT ( 'NONE',  ( 9.599999999999914380, 2.500000000000000000, 4.922947341949748257 ) ) ;
#81059 = CONICAL_SURFACE ( 'NONE', #24613, 0.1000000000000000472, 0.003490658503988666988 ) ;
#81060 = DIRECTION ( 'NONE',  ( 0.000000000000000000, 0.000000000000000000, 1.000000000000000000 ) ) ;
#81061 = EDGE_LOOP ( 'NONE', ( #43000, #15493, #19549, #84011 ) ) ;
#81062 = DIRECTION ( 'NONE',  ( -0.000000000000000000, 1.000000000000000000, -0.000000000000000000 ) ) ;
#81064 = AXIS2_PLACEMENT_3D ( 'NONE', #107508, #117288, #7358 ) ;
#81063 = CONICAL_SURFACE ( 'NONE', #24618, 0.1000000000000002554, 0.003490658503988666988 ) ;
#81065 = CARTESIAN_POINT ( 'NONE',  ( -5.650000000000023448, 12.50000000000000000, -6.841600689897078702 ) ) ;
#81066 = ORIENTED_EDGE ( 'NONE', *, *, #107016, .T. ) ;
#81067 = EDGE_LOOP ( 'NONE', ( #102297, #61491 ) ) ;
#81068 = CARTESIAN_POINT ( 'NONE',  ( 186.6718750003414016, 9.264065473108010111E-16, -7.564683531250000925 ) ) ;
#81069 = DIRECTION ( 'NONE',  ( 0.000000000000000000, 1.000000000000000000, 0.000000000000000000 ) ) ;
#81070 = CARTESIAN_POINT ( 'NONE',  ( -0.4000000000000396572, 2.500000000000000000, 3.737306695894644371 ) ) ;
#81071 = CARTESIAN_POINT ( 'NONE',  ( 3.949999999999939782, 2.500000000000000000, 2.411473670974873862 ) ) ;
#81072 = LINE ( 'NONE', #72547, #40212 ) ;
#81073 = DIRECTION ( 'NONE',  ( 0.000000000000000000, -0.000000000000000000, 1.000000000000000000 ) ) ;
#81074 = DIRECTION ( 'NONE',  ( 0.000000000000000000, 1.000000000000000000, 0.000000000000000000 ) ) ;
#81075 = DIRECTION ( 'NONE',  ( 0.000000000000000000, -0.9999939076577903929, 0.003490651415223739937 ) ) ;
#81076 = EDGE_CURVE ( 'NONE', #54453, #12380, #117080, .T. ) ;
#81077 = EDGE_CURVE ( 'NONE', #71302, #108547, #110075, .T. ) ;
#81078 = FACE_OUTER_BOUND ( 'NONE', #96833, .T. ) ;
#81079 = VERTEX_POINT ( 'NONE', #5195 ) ;
#81080 = ORIENTED_EDGE ( 'NONE', *, *, #75964, .F. ) ;
#81081 = EDGE_CURVE ( 'NONE', #22283, #5141, #124735, .T. ) ;
#81082 = EDGE_LOOP ( 'NONE', ( #98260, #27659 ) ) ;
#81083 = CIRCLE ( 'NONE', #31025, 0.06509327318403745899 ) ;
#81084 = EDGE_LOOP ( 'NONE', ( #14857, #105047 ) ) ;
#81085 = ADVANCED_FACE ( 'NONE', ( #46414 ), #80835, .T. ) ;
#81086 = ORIENTED_EDGE ( 'NONE', *, *, #50875, .F. ) ;
#81087 = DIRECTION ( 'NONE',  ( 0.000000000000000000, 0.000000000000000000, 1.000000000000000000 ) ) ;
#81088 = DIRECTION ( 'NONE',  ( 0.000000000000000000, -0.000000000000000000, 1.000000000000000000 ) ) ;
#81089 = ADVANCED_FACE ( 'NONE', ( #126930 ), #51500, .T. ) ;
#81090 = EDGE_LOOP ( 'NONE', ( #113390, #45006 ) ) ;
#81092 = ADVANCED_FACE ( 'NONE', ( #7780 ), #120538, .T. ) ;
#81091 = CONICAL_SURFACE ( 'NONE', #79037, 0.1000000000000002554, 0.003490658503988666988 ) ;
#81093 = DIRECTION ( 'NONE',  ( 0.000000000000000000, 0.000000000000000000, -1.000000000000000000 ) ) ;
#81095 = DIRECTION ( 'NONE',  ( 0.000000000000000000, 0.000000000000000000, 1.000000000000000000 ) ) ;
#81094 = CONICAL_SURFACE ( 'NONE', #24649, 0.1000000000000002554, 0.003490658503988666988 ) ;
#81096 = ADVANCED_FACE ( 'NONE', ( #125613 ), #96161, .T. ) ;
#81097 = DIRECTION ( 'NONE',  ( 0.000000000000000000, 0.000000000000000000, 1.000000000000000000 ) ) ;
#81099 = EDGE_LOOP ( 'NONE', ( #38267, #37709 ) ) ;
#81098 = DIRECTION ( 'NONE',  ( 0.000000000000000000, 1.000000000000000000, 0.000000000000000000 ) ) ;
#81100 = CARTESIAN_POINT ( 'NONE',  ( -1.250000000000001554, 2.500000000000000000, 6.395190528383296602 ) ) ;
#81101 = EDGE_CURVE ( 'NONE', #46700, #87285, #78698, .T. ) ;
#81102 = VECTOR ( 'NONE', #21651, 1000.000000000000000 ) ;
#81103 = CARTESIAN_POINT ( 'NONE',  ( -0.8500000000000386136, 2.500000000000000000, 1.472243186433545459 ) ) ;
#81104 = ORIENTED_EDGE ( 'NONE', *, *, #80771, .T. ) ;
#81105 = AXIS2_PLACEMENT_3D ( 'NONE', #42585, #20987, #71362 ) ;
#81106 = CONICAL_SURFACE ( 'NONE', #118643, 0.1000000000000002554, 0.003490658503988666988 ) ;
#81107 = EDGE_LOOP ( 'NONE', ( #63744, #77035 ) ) ;
#81108 = ORIENTED_EDGE ( 'NONE', *, *, #110883, .T. ) ;
#81109 = ORIENTED_EDGE ( 'NONE', *, *, #106733, .F. ) ;
#81110 = FACE_OUTER_BOUND ( 'NONE', #77748, .T. ) ;
#81111 = DIRECTION ( 'NONE',  ( 0.000000000000000000, 0.000000000000000000, -1.000000000000000000 ) ) ;
#81112 = CARTESIAN_POINT ( 'NONE',  ( -11.44999999999999751, 2.500000000000000000, -6.741600689897073728 ) ) ;
#81113 = DIRECTION ( 'NONE',  ( 0.000000000000000000, 1.000000000000000000, 0.000000000000000000 ) ) ;
#81114 = ORIENTED_EDGE ( 'NONE', *, *, #18647, .F. ) ;
#81115 = CIRCLE ( 'NONE', #41413, 0.06509327318403745899 ) ;
#81116 = CARTESIAN_POINT ( 'NONE',  ( -13.54999999999998828, 12.50000000000000000, -2.511473670974875727 ) ) ;
#81117 = LINE ( 'NONE', #20897, #66366 ) ;
#81118 = DIRECTION ( 'NONE',  ( 0.000000000000000000, 0.000000000000000000, 1.000000000000000000 ) ) ;
#81119 = DIRECTION ( 'NONE',  ( 0.000000000000000000, 0.000000000000000000, 1.000000000000000000 ) ) ;
#81120 = EDGE_CURVE ( 'NONE', #118657, #28229, #47724, .T. ) ;
#81121 = EDGE_LOOP ( 'NONE', ( #92129, #58670 ) ) ;
#81122 = AXIS2_PLACEMENT_3D ( 'NONE', #9963, #91742, #2058 ) ;
#81123 = CIRCLE ( 'NONE', #87355, 0.1000000000000000472 ) ;
#81124 = ORIENTED_EDGE ( 'NONE', *, *, #17805, .T. ) ;
#81125 = EDGE_LOOP ( 'NONE', ( #41387, #106866 ) ) ;
#81126 = CARTESIAN_POINT ( 'NONE',  ( 5.199999999999931788, 2.500000000000000000, 4.676537180435972552 ) ) ;
#81127 = LINE ( 'NONE', #2535, #102489 ) ;
#81128 = FACE_BOUND ( 'NONE', #128603, .T. ) ;
#81129 = AXIS2_PLACEMENT_3D ( 'NONE', #50594, #90520, #859 ) ;
#81130 = DIRECTION ( 'NONE',  ( -0.000000000000000000, 1.000000000000000000, -0.000000000000000000 ) ) ;
#81131 = DIRECTION ( 'NONE',  ( 0.000000000000000000, 0.000000000000000000, 1.000000000000000000 ) ) ;
#81132 = CIRCLE ( 'NONE', #20490, 0.09999999999999999167 ) ;
#81133 = DIRECTION ( 'NONE',  ( -4.274815082592931898E-19, -0.9999939076577903929, -0.003490651415223739937 ) ) ;
#81134 = AXIS2_PLACEMENT_3D ( 'NONE', #95754, #114737, #23799 ) ;
#81135 = EDGE_CURVE ( 'NONE', #114764, #22907, #118380, .T. ) ;
#81136 = CARTESIAN_POINT ( 'NONE',  ( 2.099999999999947686, 2.500000000000000000, 5.122947341949749323 ) ) ;
#81138 = LINE ( 'NONE', #90276, #117655 ) ;
#81137 = CIRCLE ( 'NONE', #5600, 0.1000000000000002554 ) ;
#81139 = CARTESIAN_POINT ( 'NONE',  ( -1.250000000000035749, 12.50000000000000000, -2.792790559304616504 ) ) ;
#81140 = EDGE_LOOP ( 'NONE', ( #337, #19979 ) ) ;
#81141 = DIRECTION ( 'NONE',  ( -4.274815082592931898E-19, -0.9999939076577903929, -0.003490651415223739937 ) ) ;
#81142 = CARTESIAN_POINT ( 'NONE',  ( 183.8203125005121024, 0.000000000000000000, 7.632341765625000107 ) ) ;
#81143 = ORIENTED_EDGE ( 'NONE', *, *, #111742, .F. ) ;
#81144 = ORIENTED_EDGE ( 'NONE', *, *, #31447, .F. ) ;
#81145 = DIRECTION ( 'NONE',  ( 0.000000000000000000, 0.000000000000000000, -1.000000000000000000 ) ) ;
#81146 = AXIS2_PLACEMENT_3D ( 'NONE', #23668, #83246, #53135 ) ;
#81147 = EDGE_CURVE ( 'NONE', #25877, #42358, #49452, .T. ) ;
#81148 = DIRECTION ( 'NONE',  ( 0.000000000000000000, 0.000000000000000000, 1.000000000000000000 ) ) ;
#81149 = FACE_BOUND ( 'NONE', #8903, .T. ) ;
#81150 = CARTESIAN_POINT ( 'NONE',  ( 13.09999999999990195, 2.500000000000000000, -4.083716857408426826 ) ) ;
#81152 = CONICAL_SURFACE ( 'NONE', #16359, 0.09999999999999982514, 0.003490658503988666988 ) ;
#81151 = VECTOR ( 'NONE', #24071, 1000.000000000000000 ) ;
#81153 = FACE_BOUND ( 'NONE', #115387, .T. ) ;
#81154 = EDGE_LOOP ( 'NONE', ( #108240, #73479 ) ) ;
#81155 = CARTESIAN_POINT ( 'NONE',  ( 8.749999999999918288, 2.500000000000000000, -1.472243186433550122 ) ) ;
#81156 = CARTESIAN_POINT ( 'NONE',  ( 185.2500000000000000, 9.429780353434619030E-16, -7.700000000000000178 ) ) ;
#81157 = ORIENTED_EDGE ( 'NONE', *, *, #60426, .F. ) ;
#81158 = LINE ( 'NONE', #111228, #11402 ) ;
#81159 = DIRECTION ( 'NONE',  ( -0.000000000000000000, 1.000000000000000000, -0.000000000000000000 ) ) ;
#81160 = CARTESIAN_POINT ( 'NONE',  ( -10.20000000000000462, 2.500000000000000000, 4.576537180435972019 ) ) ;
#81161 = FACE_OUTER_BOUND ( 'NONE', #29531, .T. ) ;
#81162 = ORIENTED_EDGE ( 'NONE', *, *, #109271, .T. ) ;
#81163 = EDGE_CURVE ( 'NONE', #18723, #88124, #126801, .T. ) ;
#81164 = DIRECTION ( 'NONE',  ( 0.000000000000000000, 0.000000000000000000, 1.000000000000000000 ) ) ;
#81165 = CARTESIAN_POINT ( 'NONE',  ( 4.999999999999973355, 12.50000000000000000, -4.265033745738164406 ) ) ;
#81166 = AXIS2_PLACEMENT_3D ( 'NONE', #54943, #94875, #54308 ) ;
#81167 = CARTESIAN_POINT ( 'NONE',  ( 8.749999999999923617, 2.500000000000000000, 1.572243186433545548 ) ) ;
#81168 = ORIENTED_EDGE ( 'NONE', *, *, #67621, .F. ) ;
#81169 = ORIENTED_EDGE ( 'NONE', *, *, #57511, .F. ) ;
#81170 = LINE ( 'NONE', #42554, #24237 ) ;
#81171 = ADVANCED_FACE ( 'NONE', ( #77803 ), #114266, .T. ) ;
#81172 = EDGE_LOOP ( 'NONE', ( #52548, #107421 ) ) ;
#81173 = FACE_OUTER_BOUND ( 'NONE', #9845, .T. ) ;
#81174 = CARTESIAN_POINT ( 'NONE',  ( 1.249999999999988454, 2.500000000000000000, -2.165063509461101710 ) ) ;
#81175 = AXIS2_PLACEMENT_3D ( 'NONE', #66121, #24269, #125045 ) ;
#81176 = DIRECTION ( 'NONE',  ( 0.000000000000000000, 0.000000000000000000, 1.000000000000000000 ) ) ;
#81177 = ORIENTED_EDGE ( 'NONE', *, *, #14659, .F. ) ;
#81178 = DIRECTION ( 'NONE',  ( 0.000000000000000000, 0.000000000000000000, 1.000000000000000000 ) ) ;
#81179 = PLANE ( 'NONE',  #97879 ) ;
#81180 = CARTESIAN_POINT ( 'NONE',  ( 9.599999999999914380, 12.50000000000000000, -4.330127018922201643 ) ) ;
#81181 = EDGE_CURVE ( 'NONE', #3394, #63089, #17596, .T. ) ;
#81182 = ADVANCED_FACE ( 'NONE', ( #116442 ), #99239, .T. ) ;
#81183 = CARTESIAN_POINT ( 'NONE',  ( -6.249999999999981348, 2.500000000000000000, 2.065063509461097624 ) ) ;
#81184 = DIRECTION ( 'NONE',  ( 0.000000000000000000, 0.000000000000000000, 1.000000000000000000 ) ) ;
#81185 = EDGE_CURVE ( 'NONE', #89603, #71314, #103353, .T. ) ;
#81186 = EDGE_CURVE ( 'NONE', #16632, #4736, #25480, .T. ) ;
#81187 = DIRECTION ( 'NONE',  ( -0.000000000000000000, -1.000000000000000000, -0.000000000000000000 ) ) ;
#81188 = CIRCLE ( 'NONE', #26806, 0.1000000000000002554 ) ;
#81189 = EDGE_LOOP ( 'NONE', ( #88093, #44742, #57232, #15927 ) ) ;
#81191 = ORIENTED_EDGE ( 'NONE', *, *, #78946, .F. ) ;
#81190 = CIRCLE ( 'NONE', #62321, 0.06509327318403741736 ) ;
#81192 = DIRECTION ( 'NONE',  ( 0.000000000000000000, 0.000000000000000000, 1.000000000000000000 ) ) ;
#81193 = VERTEX_POINT ( 'NONE', #35964 ) ;
#81194 = FACE_OUTER_BOUND ( 'NONE', #50025, .T. ) ;
#81196 = ORIENTED_EDGE ( 'NONE', *, *, #124698, .T. ) ;
#81195 = ORIENTED_EDGE ( 'NONE', *, *, #8037, .F. ) ;
#81197 = ORIENTED_EDGE ( 'NONE', *, *, #124203, .F. ) ;
#81198 = EDGE_CURVE ( 'NONE', #113969, #91010, #75880, .T. ) ;
#81199 = DIRECTION ( 'NONE',  ( 0.000000000000000000, 0.000000000000000000, 1.000000000000000000 ) ) ;
#81200 = EDGE_CURVE ( 'NONE', #67150, #48754, #21879, .T. ) ;
#81202 = PLANE ( 'NONE',  #61125 ) ;
#81201 = CIRCLE ( 'NONE', #87438, 0.1000000000000002554 ) ;
#81203 = EDGE_CURVE ( 'NONE', #87409, #105515, #42823, .T. ) ;
#81204 = DIRECTION ( 'NONE',  ( 0.000000000000000000, 1.000000000000000000, 0.000000000000000000 ) ) ;
#81205 = SURFACE_STYLE_USAGE ( .BOTH. , #50440 ) ;
#81206 = CARTESIAN_POINT ( 'NONE',  ( 1.649999999999949729, 2.500000000000000000, 7.188010851410848723 ) ) ;
#81207 = LINE ( 'NONE', #69432, #96098 ) ;
#81208 = DIRECTION ( 'NONE',  ( 0.000000000000000000, 0.000000000000000000, -1.000000000000000000 ) ) ;
#81209 = CARTESIAN_POINT ( 'NONE',  ( -5.850000000000022737, 12.50000000000000000, -6.430097255199264339 ) ) ;
#81210 = VECTOR ( 'NONE', #66252, 1000.000000000000000 ) ;
#81211 = PLANE ( 'NONE',  #59453 ) ;
#81212 = CARTESIAN_POINT ( 'NONE',  ( 14.14999999999989377, 12.50000000000000000, -2.857883832488653741 ) ) ;
#81213 = CONICAL_SURFACE ( 'NONE', #31055, 0.1000000000000002554, 0.003490658503988666988 ) ;
#81214 = ORIENTED_EDGE ( 'NONE', *, *, #25458, .T. ) ;
#81215 =( GEOMETRIC_REPRESENTATION_CONTEXT ( 3 ) GLOBAL_UNCERTAINTY_ASSIGNED_CONTEXT ( ( #19173 ) ) GLOBAL_UNIT_ASSIGNED_CONTEXT ( ( #127086, #89723, #37417 ) ) REPRESENTATION_CONTEXT ( 'NONE', 'WORKASPACE' ) );
#81216 = CARTESIAN_POINT ( 'NONE',  ( -2.700000000000029932, 12.50000000000000000, -0.3464101615137782364 ) ) ;
#81217 = EDGE_LOOP ( 'NONE', ( #11632, #16774, #121334, #25000 ) ) ;
#81218 = ORIENTED_EDGE ( 'NONE', *, *, #75394, .T. ) ;
#81219 = CARTESIAN_POINT ( 'NONE',  ( 12.49999999999990052, 2.500000000000000000, 0.6928203230275494784 ) ) ;
#81220 = CIRCLE ( 'NONE', #129266, 0.1000000000000002554 ) ;
#81221 = DIRECTION ( 'NONE',  ( 0.000000000000000000, 1.000000000000000000, 0.000000000000000000 ) ) ;
#81223 = CONICAL_SURFACE ( 'NONE', #112529, 0.1000000000000002554, 0.003490658503988666988 ) ;
#81222 = DIRECTION ( 'NONE',  ( -0.000000000000000000, -1.000000000000000000, -0.000000000000000000 ) ) ;
#81224 = CARTESIAN_POINT ( 'NONE',  ( 11.44999999999990692, 12.50000000000000000, -6.906693963081115939 ) ) ;
#81225 = DIRECTION ( 'NONE',  ( 0.000000000000000000, -0.000000000000000000, 1.000000000000000000 ) ) ;
#81226 = DIRECTION ( 'NONE',  ( -0.000000000000000000, 1.000000000000000000, -0.000000000000000000 ) ) ;
#81227 = ORIENTED_EDGE ( 'NONE', *, *, #108531, .F. ) ;
#81228 = AXIS2_PLACEMENT_3D ( 'NONE', #59779, #30953, #29017 ) ;
#81229 = ORIENTED_EDGE ( 'NONE', *, *, #42685, .F. ) ;
#81230 = ORIENTED_EDGE ( 'NONE', *, *, #73, .T. ) ;
#81231 = CARTESIAN_POINT ( 'NONE',  ( 3.149999999999944400, 2.500000000000000000, 2.411473670974873862 ) ) ;
#81232 = ORIENTED_EDGE ( 'NONE', *, *, #9825, .T. ) ;
#81233 = AXIS2_PLACEMENT_3D ( 'NONE', #63279, #105128, #15448 ) ;
#81234 = ADVANCED_FACE ( 'NONE', ( #38567 ), #129529, .T. ) ;
#81235 = ORIENTED_EDGE ( 'NONE', *, *, #60668, .F. ) ;
#81236 = CARTESIAN_POINT ( 'NONE',  ( 5.599999999999934808, 2.500000000000000000, -4.676537180435978769 ) ) ;
#81237 = DIRECTION ( 'NONE',  ( 0.000000000000000000, 0.000000000000000000, 1.000000000000000000 ) ) ;
#81238 = ADVANCED_FACE ( 'NONE', ( #60762 ), #69270, .T. ) ;
#81240 = AXIS2_PLACEMENT_3D ( 'NONE', #46987, #107824, #116345 ) ;
#81239 = AXIS2_PLACEMENT_3D ( 'NONE', #12710, #22577, #62496 ) ;
#81241 = CARTESIAN_POINT ( 'NONE',  ( 4.999999999999935163, 2.500000000000000000, 0.7928203230275495672 ) ) ;
#81242 = CARTESIAN_POINT ( 'NONE',  ( 2.299999999999949640, 12.50000000000000000, -4.676537180435977881 ) ) ;
#81243 = EDGE_CURVE ( 'NONE', #59490, #73228, #17647, .T. ) ;
#81244 = CARTESIAN_POINT ( 'NONE',  ( 9.149999999999920419, 2.500000000000000000, -7.188010851410854052 ) ) ;
#81245 = EDGE_LOOP ( 'NONE', ( #109801, #98304 ) ) ;
#81246 = CARTESIAN_POINT ( 'NONE',  ( 9.149999999999915090, 12.50000000000000000, 6.430097255199259010 ) ) ;
#81247 = CARTESIAN_POINT ( 'NONE',  ( 1.049999999999954969, 12.50000000000000000, -6.841600689897077814 ) ) ;
#81248 = FACE_OUTER_BOUND ( 'NONE', #89467, .T. ) ;
#81249 = FACE_OUTER_BOUND ( 'NONE', #82486, .T. ) ;
#81250 = ADVANCED_FACE ( 'NONE', ( #118381 ), #59554, .T. ) ;
#81251 = CARTESIAN_POINT ( 'NONE',  ( 4.199999999999938005, 12.50000000000000000, 4.330127018922196314 ) ) ;
#81252 = ORIENTED_EDGE ( 'NONE', *, *, #114124, .F. ) ;
#81253 = VERTEX_POINT ( 'NONE', #532 ) ;
#81254 = VERTEX_POINT ( 'NONE', #68638 ) ;
#81255 = FACE_OUTER_BOUND ( 'NONE', #62212, .T. ) ;
#81256 = ORIENTED_EDGE ( 'NONE', *, *, #54866, .F. ) ;
#81257 = DIRECTION ( 'NONE',  ( 0.000000000000000000, -0.000000000000000000, 1.000000000000000000 ) ) ;
#81258 = DIRECTION ( 'NONE',  ( 0.000000000000000000, 0.000000000000000000, 1.000000000000000000 ) ) ;
#81259 = AXIS2_PLACEMENT_3D ( 'NONE', #24898, #65455, #126327 ) ;
#81260 = CIRCLE ( 'NONE', #49980, 0.09999999999999982514 ) ;
#81261 = CIRCLE ( 'NONE', #89574, 0.09999999999999982514 ) ;
#81262 = ORIENTED_EDGE ( 'NONE', *, *, #46022, .F. ) ;
#81263 = DIRECTION ( 'NONE',  ( -0.000000000000000000, -1.000000000000000000, -0.000000000000000000 ) ) ;
#81264 = DIRECTION ( 'NONE',  ( 0.000000000000000000, 0.000000000000000000, -1.000000000000000000 ) ) ;
#81265 = DIRECTION ( 'NONE',  ( 0.000000000000000000, 0.000000000000000000, -1.000000000000000000 ) ) ;
#81266 = ADVANCED_FACE ( 'NONE', ( #110498 ), #101286, .T. ) ;
#81267 = CARTESIAN_POINT ( 'NONE',  ( -1.650000000000035216, 12.50000000000000000, -1.472243186433550122 ) ) ;
#81268 = AXIS2_PLACEMENT_3D ( 'NONE', #118843, #88744, #99218 ) ;
#81269 = CONICAL_SURFACE ( 'NONE', #33263, 0.1000000000000002554, 0.003490658503988666988 ) ;
#81270 = FACE_OUTER_BOUND ( 'NONE', #89110, .T. ) ;
#81271 = AXIS2_PLACEMENT_3D ( 'NONE', #27706, #99039, #66976 ) ;
#81272 = VERTEX_POINT ( 'NONE', #88258 ) ;
#81273 = ORIENTED_EDGE ( 'NONE', *, *, #1867, .T. ) ;
#81274 = CARTESIAN_POINT ( 'NONE',  ( -0.4000000000000339950, 2.500000000000000000, 0.5928203230275517210 ) ) ;
#81275 = DIRECTION ( 'NONE',  ( -0.000000000000000000, 1.000000000000000000, -0.000000000000000000 ) ) ;
#81276 = VECTOR ( 'NONE', #48777, 1000.000000000000000 ) ;
#81277 = LINE ( 'NONE', #80638, #120302 ) ;
#81278 = DIRECTION ( 'NONE',  ( 0.000000000000000000, 0.000000000000000000, 1.000000000000000000 ) ) ;
#81279 = VECTOR ( 'NONE', #98131, 1000.000000000000000 ) ;
#81280 = ORIENTED_EDGE ( 'NONE', *, *, #72002, .T. ) ;
#81281 = ADVANCED_FACE ( 'NONE', ( #40500 ), #28731, .T. ) ;
#81282 = ORIENTED_EDGE ( 'NONE', *, *, #126690, .F. ) ;
#81283 = DIRECTION ( 'NONE',  ( 0.000000000000000000, 0.000000000000000000, -1.000000000000000000 ) ) ;
#81284 = CARTESIAN_POINT ( 'NONE',  ( -3.750000000000026201, 12.50000000000000000, 5.802370205355744659 ) ) ;
#81285 = DIRECTION ( 'NONE',  ( -0.000000000000000000, -1.000000000000000000, -0.000000000000000000 ) ) ;
#81286 = VERTEX_POINT ( 'NONE', #109197 ) ;
#81287 = CONICAL_SURFACE ( 'NONE', #64548, 0.1000000000000002554, 0.003490658503988666988 ) ;
#81288 = LINE ( 'NONE', #120564, #42696 ) ;
#81289 = DIRECTION ( 'NONE',  ( 0.000000000000000000, 0.000000000000000000, -1.000000000000000000 ) ) ;
#81290 = VECTOR ( 'NONE', #49865, 1000.000000000000000 ) ;
#81291 = VERTEX_POINT ( 'NONE', #80410 ) ;
#81292 = DIRECTION ( 'NONE',  ( -0.000000000000000000, 1.000000000000000000, -0.000000000000000000 ) ) ;
#81293 = EDGE_CURVE ( 'NONE', #30241, #61867, #46918, .T. ) ;
#81294 = EDGE_LOOP ( 'NONE', ( #85246, #88480, #69993, #70613 ) ) ;
#81295 = LINE ( 'NONE', #121207, #34918 ) ;
#81296 = ORIENTED_EDGE ( 'NONE', *, *, #67430, .F. ) ;
#81297 = ORIENTED_EDGE ( 'NONE', *, *, #74021, .F. ) ;
#81298 = CIRCLE ( 'NONE', #100083, 5.000000000000000000 ) ;
#81299 = CARTESIAN_POINT ( 'NONE',  ( 1.899999999999949507, 2.500000000000000000, 4.576537180435972019 ) ) ;
#81300 = CARTESIAN_POINT ( 'NONE',  ( 14.69205215198098102, 2.499999999999999556, -6.336420067969235959 ) ) ;
#81301 = ORIENTED_EDGE ( 'NONE', *, *, #46398, .F. ) ;
#81302 = EDGE_CURVE ( 'NONE', #36694, #124473, #34410, .T. ) ;
#81303 = EDGE_LOOP ( 'NONE', ( #116937, #84889, #55763, #129032 ) ) ;
#81304 = DIRECTION ( 'NONE',  ( 0.000000000000000000, 0.000000000000000000, -1.000000000000000000 ) ) ;
#81305 = DIRECTION ( 'NONE',  ( 0.000000000000000000, 0.000000000000000000, -1.000000000000000000 ) ) ;
#81306 = AXIS2_PLACEMENT_3D ( 'NONE', #122736, #33093, #114207 ) ;
#81307 = ORIENTED_EDGE ( 'NONE', *, *, #89940, .T. ) ;
#81308 = CARTESIAN_POINT ( 'NONE',  ( 187.4218750003414016, 0.000000000000000000, 7.564683531250000925 ) ) ;
#81309 = CARTESIAN_POINT ( 'NONE',  ( 184.5260416670080588, -6.551208109652273848, -3.782341765625003571 ) ) ;
#81310 = AXIS2_PLACEMENT_3D ( 'NONE', #93349, #92704, #3041 ) ;
#81311 = FACE_OUTER_BOUND ( 'NONE', #107541, .T. ) ;
#81312 = DIRECTION ( 'NONE',  ( 0.000000000000000000, 0.000000000000000000, 1.000000000000000000 ) ) ;
#81313 = CARTESIAN_POINT ( 'NONE',  ( 7.899999999999924860, 12.50000000000000000, 4.957854068765711553 ) ) ;
#81314 = DIRECTION ( 'NONE',  ( -0.000000000000000000, 1.000000000000000000, -0.000000000000000000 ) ) ;
#81315 = CARTESIAN_POINT ( 'NONE',  ( 187.5000000000000000, 0.000000000000000000, 0.000000000000000000 ) ) ;
#81316 = AXIS2_PLACEMENT_3D ( 'NONE', #91969, #109682, #122720 ) ;
#81317 = VERTEX_POINT ( 'NONE', #128223 ) ;
#81319 = ORIENTED_EDGE ( 'NONE', *, *, #6247, .T. ) ;
#81318 = ADVANCED_FACE ( 'NONE', ( #90860 ), #100663, .T. ) ;
#81320 = CARTESIAN_POINT ( 'NONE',  ( -12.69999999999999041, 2.500000000000000000, 4.083716857408421497 ) ) ;
#81322 = AXIS2_PLACEMENT_3D ( 'NONE', #72602, #5757, #103351 ) ;
#81321 = AXIS2_PLACEMENT_3D ( 'NONE', #41337, #100244, #21026 ) ;
#81323 = ORIENTED_EDGE ( 'NONE', *, *, #113241, .T. ) ;
#81324 = FACE_OUTER_BOUND ( 'NONE', #78370, .T. ) ;
#81325 = CARTESIAN_POINT ( 'NONE',  ( -5.450000000000019718, 2.500000000000000000, 6.395190528383296602 ) ) ;
#81326 = PLANE ( 'NONE',  #34381 ) ;
#81328 = ORIENTED_EDGE ( 'NONE', *, *, #82783, .T. ) ;
#81327 = ORIENTED_EDGE ( 'NONE', *, *, #72882, .T. ) ;
#81329 = FACE_BOUND ( 'NONE', #90148, .T. ) ;
#81330 = ORIENTED_EDGE ( 'NONE', *, *, #83711, .T. ) ;
#81331 = CARTESIAN_POINT ( 'NONE',  ( 6.049999999999930544, 2.500000000000000000, 2.511473670974873507 ) ) ;
#81332 = DIRECTION ( 'NONE',  ( 0.000000000000000000, 0.000000000000000000, -1.000000000000000000 ) ) ;
#81334 = ADVANCED_FACE ( 'NONE', ( #59503 ), #7180, .T. ) ;
#81333 = DIRECTION ( 'NONE',  ( -0.000000000000000000, 1.000000000000000000, -0.000000000000000000 ) ) ;
#81337 = DIRECTION ( 'NONE',  ( -0.000000000000000000, 1.000000000000000000, -0.000000000000000000 ) ) ;
#81336 = AXIS2_PLACEMENT_3D ( 'NONE', #82891, #23961, #12817 ) ;
#81335 = CIRCLE ( 'NONE', #6085, 0.1000000000000002554 ) ;
#81338 = DIRECTION ( 'NONE',  ( -0.000000000000000000, -1.000000000000000000, -0.000000000000000000 ) ) ;
#81339 = DIRECTION ( 'NONE',  ( 0.000000000000000000, 1.000000000000000000, 0.000000000000000000 ) ) ;
#81340 = CARTESIAN_POINT ( 'NONE',  ( 0.5999999999999555689, 12.50000000000000000, 4.741630453620009789 ) ) ;
#81341 = DIRECTION ( 'NONE',  ( 0.000000000000000000, 0.000000000000000000, -1.000000000000000000 ) ) ;
#81342 = EDGE_CURVE ( 'NONE', #76788, #20030, #1189, .T. ) ;
#81343 = EDGE_CURVE ( 'NONE', #120641, #80322, #97077, .T. ) ;
#81344 = DIRECTION ( 'NONE',  ( -0.000000000000000000, -1.000000000000000000, -0.000000000000000000 ) ) ;
#81345 = DIRECTION ( 'NONE',  ( -0.000000000000000000, 1.000000000000000000, -0.000000000000000000 ) ) ;
#81346 = EDGE_CURVE ( 'NONE', #27663, #86126, #44864, .T. ) ;
#81347 = EDGE_CURVE ( 'NONE', #47691, #68346, #39216, .T. ) ;
#81348 = CARTESIAN_POINT ( 'NONE',  ( 11.44999999999991047, 12.50000000000000000, -2.446380397790840266 ) ) ;
#81349 = EDGE_LOOP ( 'NONE', ( #43387, #5323 ) ) ;
#81350 = ORIENTED_EDGE ( 'NONE', *, *, #120857, .F. ) ;
#81351 = VERTEX_POINT ( 'NONE', #63335 ) ;
#81352 = ORIENTED_EDGE ( 'NONE', *, *, #120078, .T. ) ;
#81353 = CARTESIAN_POINT ( 'NONE',  ( 2.299999999999949640, 2.500000000000000000, -4.576537180435977348 ) ) ;
#81354 = EDGE_CURVE ( 'NONE', #32777, #104745, #117996, .T. ) ;
#81355 = AXIS2_PLACEMENT_3D ( 'NONE', #7722, #95475, #125565 ) ;
#81356 = DIRECTION ( 'NONE',  ( 0.000000000000000000, 1.000000000000000000, 0.000000000000000000 ) ) ;
#81359 = ORIENTED_EDGE ( 'NONE', *, *, #41877, .F. ) ;
#81358 = ORIENTED_EDGE ( 'NONE', *, *, #27989, .T. ) ;
#81357 = EDGE_CURVE ( 'NONE', #37854, #53973, #22146, .T. ) ;
#81360 = ORIENTED_EDGE ( 'NONE', *, *, #76862, .F. ) ;
#81361 = EDGE_CURVE ( 'NONE', #77956, #128073, #65766, .T. ) ;
#81362 = CARTESIAN_POINT ( 'NONE',  ( 8.749999999999953815, 12.50000000000000000, -2.165063509461101710 ) ) ;
#81363 = ADVANCED_FACE ( 'NONE', ( #33252 ), #3091, .T. ) ;
#81364 = AXIS2_PLACEMENT_3D ( 'NONE', #41192, #93492, #70623 ) ;
#81365 = EDGE_CURVE ( 'NONE', #75566, #40560, #72525, .T. ) ;
#81366 = DIRECTION ( 'NONE',  ( 0.000000000000000000, 0.000000000000000000, 1.000000000000000000 ) ) ;
#81367 = SURFACE_STYLE_FILL_AREA ( #41449 ) ;
#81368 = CARTESIAN_POINT ( 'NONE',  ( 14.59999999999989484, 12.50000000000000000, 0.6928203230275494784 ) ) ;
#81369 = CARTESIAN_POINT ( 'NONE',  ( 4.799999999999937650, 12.50000000000000000, -3.918623584224389056 ) ) ;
#81370 = CARTESIAN_POINT ( 'NONE',  ( -12.09999999999999609, 2.500000000000000000, -4.430127018922199511 ) ) ;
#81371 = CARTESIAN_POINT ( 'NONE',  ( 10.59999999999990905, 12.50000000000000000, 4.048810130592458201 ) ) ;
#81372 = EDGE_CURVE ( 'NONE', #59884, #88341, #5128, .T. ) ;
#81373 = ORIENTED_EDGE ( 'NONE', *, *, #74741, .F. ) ;
#81374 = ADVANCED_FACE ( 'NONE', ( #43081 ), #38612, .T. ) ;
#81375 = AXIS2_PLACEMENT_3D ( 'NONE', #39575, #128597, #121319 ) ;
#81376 = DIRECTION ( 'NONE',  ( -0.000000000000000000, 1.000000000000000000, -0.000000000000000000 ) ) ;
#81377 = EDGE_LOOP ( 'NONE', ( #10493, #33825 ) ) ;
#81378 = AXIS2_PLACEMENT_3D ( 'NONE', #40652, #28882, #68791 ) ;
#81379 = EDGE_LOOP ( 'NONE', ( #58876, #125826, #89541, #26749 ) ) ;
#81380 = EDGE_LOOP ( 'NONE', ( #102037, #77467 ) ) ;
#81381 = DIRECTION ( 'NONE',  ( -0.000000000000000000, -1.000000000000000000, -0.000000000000000000 ) ) ;
#81382 = VERTEX_POINT ( 'NONE', #23395 ) ;
#81383 = ORIENTED_EDGE ( 'NONE', *, *, #9051, .F. ) ;
#81384 = EDGE_LOOP ( 'NONE', ( #100941, #115251, #92259, #74825 ) ) ;
#81385 = VECTOR ( 'NONE', #74857, 1000.000000000000000 ) ;
#81386 = CARTESIAN_POINT ( 'NONE',  ( 3.949999999999939782, 12.50000000000000000, 2.511473670974873507 ) ) ;
#81387 = CONICAL_SURFACE ( 'NONE', #10265, 0.1000000000000000472, 0.003490658503988666988 ) ;
#81388 = DIRECTION ( 'NONE',  ( -0.000000000000000000, 1.000000000000000000, -0.000000000000000000 ) ) ;
#81389 = CARTESIAN_POINT ( 'NONE',  ( 15.39999999999989200, 12.50000000000000000, 0.6928203230275494784 ) ) ;
#81390 = DIRECTION ( 'NONE',  ( 0.000000000000000000, 0.000000000000000000, 1.000000000000000000 ) ) ;
#81391 = DIRECTION ( 'NONE',  ( 0.000000000000000000, -0.9999939076577903929, 0.003490651415223739937 ) ) ;
#81392 = FACE_OUTER_BOUND ( 'NONE', #13105, .T. ) ;
#81393 = DIRECTION ( 'NONE',  ( -1.000000000000000000, 0.000000000000000000, 0.000000000000000000 ) ) ;
#81394 = ORIENTED_EDGE ( 'NONE', *, *, #100088, .F. ) ;
#81395 = DIRECTION ( 'NONE',  ( 0.000000000000000000, 1.000000000000000000, 0.000000000000000000 ) ) ;
#81396 = ORIENTED_EDGE ( 'NONE', *, *, #37475, .T. ) ;
#81397 = CARTESIAN_POINT ( 'NONE',  ( 110.5209590753869406, 7.548722077129768060, 4.329966018956735496 ) ) ;
#81398 = DIRECTION ( 'NONE',  ( 0.000000000000000000, -0.000000000000000000, 1.000000000000000000 ) ) ;
#81399 = VECTOR ( 'NONE', #99280, 1000.000000000000000 ) ;
#81400 = ORIENTED_EDGE ( 'NONE', *, *, #56602, .T. ) ;
#81401 = CARTESIAN_POINT ( 'NONE',  ( 0.1999999999999567124, 2.500000000000000000, -4.083716857408426826 ) ) ;
#81402 = VERTEX_POINT ( 'NONE', #13574 ) ;
#81403 = CARTESIAN_POINT ( 'NONE',  ( 184.6093750003413732, 9.264065473108010111E-16, -7.564683531250000925 ) ) ;
#81404 = EDGE_CURVE ( 'NONE', #59320, #45275, #121597, .T. ) ;
#81405 = DIRECTION ( 'NONE',  ( 0.000000000000000000, 1.000000000000000000, 0.000000000000000000 ) ) ;
#81406 = EDGE_CURVE ( 'NONE', #74953, #4337, #30201, .T. ) ;
#81407 = ORIENTED_EDGE ( 'NONE', *, *, #97529, .F. ) ;
#81408 = EDGE_LOOP ( 'NONE', ( #91537, #39454 ) ) ;
#81409 = LINE ( 'NONE', #121315, #3829 ) ;
#81410 = CARTESIAN_POINT ( 'NONE',  ( -2.900000000000029221, 2.500000000000000000, -2.276824562219559311E-15 ) ) ;
#81411 = CARTESIAN_POINT ( 'NONE',  ( 185.1718750003414016, 9.264065473108010111E-16, -7.564683531250000925 ) ) ;
#81413 = CIRCLE ( 'NONE', #52466, 0.06509327318403745899 ) ;
#81412 = CARTESIAN_POINT ( 'NONE',  ( 1.849999999999950573, 2.500000000000000000, -1.818653347947326138 ) ) ;
#81414 = ADVANCED_FACE ( 'NONE', ( #71881 ), #55322, .T. ) ;
#81415 = CARTESIAN_POINT ( 'NONE',  ( 10.84999999999990905, 2.500000000000000000, 2.757883832488649656 ) ) ;
#81416 = ORIENTED_EDGE ( 'NONE', *, *, #25456, .F. ) ;
#81417 = CARTESIAN_POINT ( 'NONE',  ( 7.949999999999922018, 2.500000000000000000, 6.595190528383296780 ) ) ;
#81418 = ORIENTED_EDGE ( 'NONE', *, *, #36717, .T. ) ;
#81419 = DIRECTION ( 'NONE',  ( 0.000000000000000000, 0.000000000000000000, 1.000000000000000000 ) ) ;
#81420 = DIRECTION ( 'NONE',  ( 0.000000000000000000, 1.000000000000000000, 0.000000000000000000 ) ) ;
#81421 = AXIS2_PLACEMENT_3D ( 'NONE', #31196, #1066, #31824 ) ;
#81422 = CONICAL_SURFACE ( 'NONE', #98126, 0.1000000000000002554, 0.003490658503988666988 ) ;
#81423 = FACE_OUTER_BOUND ( 'NONE', #101083, .T. ) ;
#81424 = DIRECTION ( 'NONE',  ( -0.000000000000000000, 1.000000000000000000, -0.000000000000000000 ) ) ;
#81425 = FACE_OUTER_BOUND ( 'NONE', #52528, .T. ) ;
#81426 = FACE_OUTER_BOUND ( 'NONE', #69604, .T. ) ;
#81427 = CARTESIAN_POINT ( 'NONE',  ( 5.399999999999932854, 2.500000000000000000, 5.022947341949748790 ) ) ;
#81428 = EDGE_LOOP ( 'NONE', ( #43882, #5392, #35911, #92186 ) ) ;
#81429 = AXIS2_PLACEMENT_3D ( 'NONE', #62290, #1413, #78226 ) ;
#81430 = DIRECTION ( 'NONE',  ( 0.000000000000000000, 0.000000000000000000, 1.000000000000000000 ) ) ;
#81431 = PLANE ( 'NONE',  #84828 ) ;
#81432 = CARTESIAN_POINT ( 'NONE',  ( 0.7999999999999548583, 12.50000000000000000, 4.330127018922196314 ) ) ;
#81433 = ORIENTED_EDGE ( 'NONE', *, *, #99081, .F. ) ;
#81434 = DIRECTION ( 'NONE',  ( 0.000000000000000000, 0.000000000000000000, 1.000000000000000000 ) ) ;
#81435 = ADVANCED_FACE ( 'NONE', ( #83630 ), #111802, .F. ) ;
#81436 = ORIENTED_EDGE ( 'NONE', *, *, #43879, .T. ) ;
#81437 = EDGE_LOOP ( 'NONE', ( #44472, #91673 ) ) ;
#81438 = LINE ( 'NONE', #40220, #109508 ) ;
#81439 = AXIS2_PLACEMENT_3D ( 'NONE', #38178, #108194, #8061 ) ;
#81440 = ORIENTED_EDGE ( 'NONE', *, *, #44636, .F. ) ;
#81441 = EDGE_CURVE ( 'NONE', #99852, #13428, #122268, .T. ) ;
#81442 = CARTESIAN_POINT ( 'NONE',  ( 21.23528140090950345, -2.699413673072311948, -2.293764360948883141 ) ) ;
#81443 = DIRECTION ( 'NONE',  ( 0.000000000000000000, 0.000000000000000000, 1.000000000000000000 ) ) ;
#81444 = ORIENTED_EDGE ( 'NONE', *, *, #110104, .T. ) ;
#81445 = CIRCLE ( 'NONE', #12474, 0.1000000000000002554 ) ;
#81446 = DIRECTION ( 'NONE',  ( 0.000000000000000000, 1.000000000000000000, 0.000000000000000000 ) ) ;
#81447 = DIRECTION ( 'NONE',  ( 0.000000000000000000, 1.000000000000000000, 0.000000000000000000 ) ) ;
#81448 = EDGE_CURVE ( 'NONE', #121848, #23090, #73788, .T. ) ;
#81449 = VECTOR ( 'NONE', #12643, 1000.000000000000000 ) ;
#81450 = VERTEX_POINT ( 'NONE', #44329 ) ;
#81452 = VECTOR ( 'NONE', #98250, 1000.000000000000000 ) ;
#81451 = CIRCLE ( 'NONE', #56394, 0.1000000000000002554 ) ;
#81453 = AXIS2_PLACEMENT_3D ( 'NONE', #124983, #24848, #16292 ) ;
#81454 = EDGE_LOOP ( 'NONE', ( #18735, #6896 ) ) ;
#81455 = ORIENTED_EDGE ( 'NONE', *, *, #65421, .F. ) ;
#81456 = LINE ( 'NONE', #62472, #4426 ) ;
#81457 = CARTESIAN_POINT ( 'NONE',  ( 11.69999999999990870, 12.50000000000000000, -4.330127018922201643 ) ) ;
#81458 = DIRECTION ( 'NONE',  ( -0.000000000000000000, 1.000000000000000000, -0.000000000000000000 ) ) ;
#81459 = EDGE_CURVE ( 'NONE', #109667, #123049, #128496, .T. ) ;
#81460 = FACE_BOUND ( 'NONE', #103103, .T. ) ;
#81461 = ORIENTED_EDGE ( 'NONE', *, *, #90882, .F. ) ;
#81462 = CONICAL_SURFACE ( 'NONE', #45965, 0.1000000000000002554, 0.003490658503988666988 ) ;
#81463 = DIRECTION ( 'NONE',  ( 0.000000000000000000, -0.000000000000000000, 1.000000000000000000 ) ) ;
#81464 = DIRECTION ( 'NONE',  ( 0.000000000000000000, 0.000000000000000000, 1.000000000000000000 ) ) ;
#81465 = ORIENTED_EDGE ( 'NONE', *, *, #111683, .T. ) ;
#81467 = DIRECTION ( 'NONE',  ( 0.000000000000000000, 0.000000000000000000, 1.000000000000000000 ) ) ;
#81466 = CIRCLE ( 'NONE', #54271, 0.09999999999999982514 ) ;
#81468 = DIRECTION ( 'NONE',  ( 0.000000000000000000, 1.000000000000000000, 0.000000000000000000 ) ) ;
#81469 = FACE_OUTER_BOUND ( 'NONE', #91833, .T. ) ;
#81470 = CARTESIAN_POINT ( 'NONE',  ( 10.44999999999991047, 2.500000000000000000, -6.595190528383302109 ) ) ;
#81471 = DIRECTION ( 'NONE',  ( -0.000000000000000000, -1.000000000000000000, -0.000000000000000000 ) ) ;
#81472 = DIRECTION ( 'NONE',  ( 0.000000000000000000, 0.000000000000000000, 1.000000000000000000 ) ) ;
#81473 = DIRECTION ( 'NONE',  ( -0.000000000000000000, 1.000000000000000000, -0.000000000000000000 ) ) ;
#81474 = VECTOR ( 'NONE', #113952, 1000.000000000000000 ) ;
#81475 = ORIENTED_EDGE ( 'NONE', *, *, #47803, .T. ) ;
#81476 = ORIENTED_EDGE ( 'NONE', *, *, #114608, .F. ) ;
#81477 = EDGE_LOOP ( 'NONE', ( #115866, #52787 ) ) ;
#81478 = ORIENTED_EDGE ( 'NONE', *, *, #37766, .T. ) ;
#81479 = CARTESIAN_POINT ( 'NONE',  ( 11.44999999999991047, 12.50000000000000000, 6.148780366869520009 ) ) ;
#81480 = CARTESIAN_POINT ( 'NONE',  ( -4.150000000000024336, 2.500000000000000000, 1.572243186433545548 ) ) ;
#81481 = ORIENTED_EDGE ( 'NONE', *, *, #110057, .F. ) ;
#81482 = FACE_BOUND ( 'NONE', #1451, .T. ) ;
#81483 = DIRECTION ( 'NONE',  ( -0.000000000000000000, 1.000000000000000000, -0.000000000000000000 ) ) ;
#81484 = CARTESIAN_POINT ( 'NONE',  ( 1.649999999999951505, 12.50000000000000000, 1.407149913249508000 ) ) ;
#81486 = EDGE_CURVE ( 'NONE', #85725, #120306, #57372, .T. ) ;
#81485 = CARTESIAN_POINT ( 'NONE',  ( 2.899999999999943956, 2.500000000000000000, 4.230127018922196669 ) ) ;
#81487 = DIRECTION ( 'NONE',  ( -0.000000000000000000, 1.000000000000000000, -0.000000000000000000 ) ) ;
#81488 = DIRECTION ( 'NONE',  ( 0.000000000000000000, 0.000000000000000000, 1.000000000000000000 ) ) ;
#81489 = CARTESIAN_POINT ( 'NONE',  ( 15.59999999999988951, 2.500000000000000000, 0.4464101615137735513 ) ) ;
#81490 = FACE_OUTER_BOUND ( 'NONE', #93744, .T. ) ;
#81491 = DIRECTION ( 'NONE',  ( 0.000000000000000000, 1.000000000000000000, 0.000000000000000000 ) ) ;
#81492 = ADVANCED_FACE ( 'NONE', ( #94084 ), #126421, .T. ) ;
#81493 = CARTESIAN_POINT ( 'NONE',  ( -14.59999999999998366, 2.500000000000000000, 0.7928203230275517877 ) ) ;
#81494 = EDGE_LOOP ( 'NONE', ( #111431, #97047 ) ) ;
#81495 = ADVANCED_FACE ( 'NONE', ( #21477 ), #57470, .T. ) ;
#81496 = ORIENTED_EDGE ( 'NONE', *, *, #62858, .F. ) ;
#81497 = ORIENTED_EDGE ( 'NONE', *, *, #119637, .T. ) ;
#81498 = ORIENTED_EDGE ( 'NONE', *, *, #83299, .F. ) ;
#81499 = VERTEX_POINT ( 'NONE', #112448 ) ;
#81500 = EDGE_LOOP ( 'NONE', ( #36530, #17481 ) ) ;
#81501 = EDGE_CURVE ( 'NONE', #72150, #33066, #9441, .T. ) ;
#81503 = ADVANCED_FACE ( 'NONE', ( #96633 ), #1023, .T. ) ;
#81502 = DIRECTION ( 'NONE',  ( 0.000000000000000000, 0.000000000000000000, -1.000000000000000000 ) ) ;
#81504 = CIRCLE ( 'NONE', #27120, 0.06509327318403745899 ) ;
#81506 = EDGE_LOOP ( 'NONE', ( #80024, #74484 ) ) ;
#81505 = ADVANCED_FACE ( 'NONE', ( #46261 ), #47011, .T. ) ;
#81510 = ADVANCED_FACE ( 'NONE', ( #6958 ), #95119, .T. ) ;
#81509 = AXIS2_PLACEMENT_3D ( 'NONE', #58604, #49437, #68402 ) ;
#81508 = CARTESIAN_POINT ( 'NONE',  ( -1.450000000000035039, 12.50000000000000000, -6.841600689897077814 ) ) ;
#81507 = VECTOR ( 'NONE', #43597, 1000.000000000000000 ) ;
#81511 = CARTESIAN_POINT ( 'NONE',  ( 4.149999999999939959, 2.500000000000000000, 2.757883832488649656 ) ) ;
#81512 = CARTESIAN_POINT ( 'NONE',  ( 105.6184301395928031, 8.500000000000000000, -1.375000000000000888 ) ) ;
#81513 = CARTESIAN_POINT ( 'NONE',  ( 14.34999999999989306, 2.500000000000000000, -2.511473670974877948 ) ) ;
#81514 = ORIENTED_EDGE ( 'NONE', *, *, #60211, .F. ) ;
#81515 = CARTESIAN_POINT ( 'NONE',  ( -4.600000000000025402, 2.500000000000000000, 4.330127018922196314 ) ) ;
#81516 = ADVANCED_FACE ( 'NONE', ( #14844 ), #126511, .T. ) ;
#81517 = AXIS2_PLACEMENT_3D ( 'NONE', #74805, #12641, #12006 ) ;
#81518 = EDGE_LOOP ( 'NONE', ( #112568, #6634, #127377, #102837 ) ) ;
#81519 = ORIENTED_EDGE ( 'NONE', *, *, #63017, .F. ) ;
#81520 = FACE_OUTER_BOUND ( 'NONE', #119325, .T. ) ;
#81521 = DIRECTION ( 'NONE',  ( 0.000000000000000000, 1.000000000000000000, 0.000000000000000000 ) ) ;
#81522 = CARTESIAN_POINT ( 'NONE',  ( 11.69999999999990870, 12.50000000000000000, 4.330127018922196314 ) ) ;
#81523 = VERTEX_POINT ( 'NONE', #95375 ) ;
#81524 = EDGE_LOOP ( 'NONE', ( #45731, #31404, #113136, #903 ) ) ;
#81525 = LINE ( 'NONE', #110335, #61068 ) ;
#81526 = CARTESIAN_POINT ( 'NONE',  ( 9.349999999999919709, 12.50000000000000000, -6.841600689897078702 ) ) ;
#81527 = DIRECTION ( 'NONE',  ( 0.000000000000000000, 1.000000000000000000, 0.000000000000000000 ) ) ;
#81528 = CARTESIAN_POINT ( 'NONE',  ( 14.99999999999989164, 2.500000000000000000, 0.6928203230275494784 ) ) ;
#81529 = ORIENTED_EDGE ( 'NONE', *, *, #12933, .T. ) ;
#81530 = DIRECTION ( 'NONE',  ( 0.000000000000000000, 0.000000000000000000, 1.000000000000000000 ) ) ;
#81531 = VERTEX_POINT ( 'NONE', #96016 ) ;
#81532 = DIRECTION ( 'NONE',  ( 0.000000000000000000, 0.000000000000000000, 1.000000000000000000 ) ) ;
#81533 = AXIS2_PLACEMENT_3D ( 'NONE', #12443, #52381, #694 ) ;
#81534 = AXIS2_PLACEMENT_3D ( 'NONE', #54585, #36272, #128534 ) ;
#81535 = ORIENTED_EDGE ( 'NONE', *, *, #48756, .F. ) ;
#81536 = DIRECTION ( 'NONE',  ( 0.000000000000000000, 0.000000000000000000, -1.000000000000000000 ) ) ;
#81537 = DIRECTION ( 'NONE',  ( 0.000000000000000000, 0.000000000000000000, -1.000000000000000000 ) ) ;
#81538 = CARTESIAN_POINT ( 'NONE',  ( 9.349999999999919709, 12.50000000000000000, -6.148780366869526226 ) ) ;
#81539 = CARTESIAN_POINT ( 'NONE',  ( 13.94999999999989271, 2.500000000000000000, -1.818653347947326138 ) ) ;
#81540 = LINE ( 'NONE', #80257, #93970 ) ;
#81541 = ORIENTED_EDGE ( 'NONE', *, *, #115309, .F. ) ;
#81542 = VECTOR ( 'NONE', #81734, 1000.000000000000000 ) ;
#81543 = CARTESIAN_POINT ( 'NONE',  ( -11.64999999999999680, 12.50000000000000000, 5.867463478539781896 ) ) ;
#81544 = ADVANCED_FACE ( 'NONE', ( #125470 ), #13532, .T. ) ;
#81545 = DIRECTION ( 'NONE',  ( -0.000000000000000000, 1.000000000000000000, -0.000000000000000000 ) ) ;
#81546 = ORIENTED_EDGE ( 'NONE', *, *, #19214, .F. ) ;
#81547 = VERTEX_POINT ( 'NONE', #54787 ) ;
#81548 = ORIENTED_EDGE ( 'NONE', *, *, #111782, .T. ) ;
#81549 = CARTESIAN_POINT ( 'NONE',  ( 11.24999999999990585, 2.500000000000000000, 2.857883832488649301 ) ) ;
#81550 = CARTESIAN_POINT ( 'NONE',  ( -7.499999999999980460, 2.500000000000000000, -4.430127018922202176 ) ) ;
#81551 = CARTESIAN_POINT ( 'NONE',  ( 187.2760416670080588, 6.551208109652274736, 3.782341765625001351 ) ) ;
#81552 = AXIS2_PLACEMENT_3D ( 'NONE', #46511, #36721, #59436 ) ;
#81553 = CARTESIAN_POINT ( 'NONE',  ( 4.349999999999941025, 2.500000000000000000, -1.818653347947326138 ) ) ;
#81554 = DIRECTION ( 'NONE',  ( 0.000000000000000000, 0.000000000000000000, 1.000000000000000000 ) ) ;
#81555 = EDGE_CURVE ( 'NONE', #8118, #54678, #5215, .T. ) ;
#81556 = VECTOR ( 'NONE', #61785, 1000.000000000000000 ) ;
#81557 = AXIS2_PLACEMENT_3D ( 'NONE', #120558, #30906, #60986 ) ;
#81558 = CARTESIAN_POINT ( 'NONE',  ( -10.60000000000000142, 2.500000000000000000, 4.676537180435972552 ) ) ;
#81559 = CARTESIAN_POINT ( 'NONE',  ( -4.150000000000024336, 2.500000000000000000, -2.065063509461102065 ) ) ;
#81560 = DIRECTION ( 'NONE',  ( 0.000000000000000000, 0.000000000000000000, -1.000000000000000000 ) ) ;
#81561 = VERTEX_POINT ( 'NONE', #45641 ) ;
#81562 = CIRCLE ( 'NONE', #20927, 0.1000000000000000472 ) ;
#81563 = DIRECTION ( 'NONE',  ( 0.000000000000000000, 0.000000000000000000, -1.000000000000000000 ) ) ;
#81564 = DIRECTION ( 'NONE',  ( 0.000000000000000000, 1.000000000000000000, 0.000000000000000000 ) ) ;
#81565 = DIRECTION ( 'NONE',  ( 0.000000000000000000, -0.9999939076577903929, 0.003490651415223739937 ) ) ;
#81566 = CARTESIAN_POINT ( 'NONE',  ( -0.4000000000000392131, 2.500000000000000000, -4.330127018922201643 ) ) ;
#81567 = ORIENTED_EDGE ( 'NONE', *, *, #72956, .T. ) ;
#81568 = DIRECTION ( 'NONE',  ( -0.000000000000000000, 1.000000000000000000, -0.000000000000000000 ) ) ;
#81569 = DIRECTION ( 'NONE',  ( 0.000000000000000000, 0.000000000000000000, 1.000000000000000000 ) ) ;
#81571 = ORIENTED_EDGE ( 'NONE', *, *, #76130, .T. ) ;
#81570 = DIRECTION ( 'NONE',  ( -4.274815082592931898E-19, -0.9999939076577903929, -0.003490651415223739937 ) ) ;
#81572 = VERTEX_POINT ( 'NONE', #76384 ) ;
#81573 = DIRECTION ( 'NONE',  ( -4.274815082592931898E-19, -0.9999939076577903929, -0.003490651415223739937 ) ) ;
#81574 = ADVANCED_FACE ( 'NONE', ( #107107 ), #85547, .T. ) ;
#81575 = VERTEX_POINT ( 'NONE', #86166 ) ;
#81576 = ORIENTED_EDGE ( 'NONE', *, *, #56947, .F. ) ;
#81577 = DIRECTION ( 'NONE',  ( 0.000000000000000000, 0.000000000000000000, -1.000000000000000000 ) ) ;
#81578 = CIRCLE ( 'NONE', #58608, 0.1000000000000000472 ) ;
#81579 = CARTESIAN_POINT ( 'NONE',  ( 20.37025966759639672, 0.6621301594404709334, -4.188616773932404946 ) ) ;
#81580 = LINE ( 'NONE', #51496, #10781 ) ;
#81581 = DIRECTION ( 'NONE',  ( 0.000000000000000000, 0.000000000000000000, 1.000000000000000000 ) ) ;
#81582 = ADVANCED_FACE ( 'NONE', ( #67163 ), #36475, .T. ) ;
#81583 = EDGE_LOOP ( 'NONE', ( #22117, #24900, #39462 ) ) ;
#81585 = VECTOR ( 'NONE', #33021, 1000.000000000000000 ) ;
#81584 = AXIS2_PLACEMENT_3D ( 'NONE', #21867, #1554, #110857 ) ;
#81586 = DIRECTION ( 'NONE',  ( -0.000000000000000000, -1.000000000000000000, -0.000000000000000000 ) ) ;
#81587 = EDGE_LOOP ( 'NONE', ( #88294, #119625 ) ) ;
#81588 = ADVANCED_FACE ( 'NONE', ( #75719 ), #44947, .T. ) ;
#81589 = CARTESIAN_POINT ( 'NONE',  ( -13.54999999999998828, 2.500000000000000000, -2.611473670974875372 ) ) ;
#81590 = CARTESIAN_POINT ( 'NONE',  ( 186.4895833340161460, -4.445597072760135937, -7.699999999999966427 ) ) ;
#81591 = ADVANCED_FACE ( 'NONE', ( #65246 ), #3184, .T. ) ;
#81592 = ORIENTED_EDGE ( 'NONE', *, *, #63017, .T. ) ;
#81593 = ORIENTED_EDGE ( 'NONE', *, *, #58306, .F. ) ;
#81594 = EDGE_CURVE ( 'NONE', #29124, #84030, #7620, .T. ) ;
#81595 = ORIENTED_EDGE ( 'NONE', *, *, #10675, .T. ) ;
#81596 = ORIENTED_EDGE ( 'NONE', *, *, #43912, .T. ) ;
#81597 = CARTESIAN_POINT ( 'NONE',  ( -6.250000000000019540, 2.500000000000000000, -2.957883832488653830 ) ) ;
#81598 = DIRECTION ( 'NONE',  ( -0.000000000000000000, -1.000000000000000000, -0.000000000000000000 ) ) ;
#81599 = DIRECTION ( 'NONE',  ( 0.000000000000000000, 0.000000000000000000, -1.000000000000000000 ) ) ;
#81600 = ADVANCED_FACE ( 'NONE', ( #84903 ), #106479, .T. ) ;
#81601 = FACE_BOUND ( 'NONE', #115061, .T. ) ;
#81602 = ORIENTED_EDGE ( 'NONE', *, *, #56234, .T. ) ;
#81603 = CARTESIAN_POINT ( 'NONE',  ( 11.64999999999990798, 2.500000000000000000, 7.088010851410848190 ) ) ;
#81604 = CARTESIAN_POINT ( 'NONE',  ( 187.0677083336747444, -4.367472073101514418, -7.564683531250002702 ) ) ;
#81605 = LINE ( 'NONE', #31871, #67806 ) ;
#81606 = CARTESIAN_POINT ( 'NONE',  ( 3.549999999999941203, 12.50000000000000000, 6.148780366869520897 ) ) ;
#81607 = CARTESIAN_POINT ( 'NONE',  ( -4.350000000000023626, 12.50000000000000000, 1.818653347947321475 ) ) ;
#81608 = FACE_OUTER_BOUND ( 'NONE', #70507, .T. ) ;
#81609 = LINE ( 'NONE', #13507, #120293 ) ;
#81610 = AXIS2_PLACEMENT_3D ( 'NONE', #124351, #115133, #102757 ) ;
#81611 = CIRCLE ( 'NONE', #48175, 0.1000000000000002554 ) ;
#81612 = DIRECTION ( 'NONE',  ( -0.000000000000000000, 1.000000000000000000, -0.000000000000000000 ) ) ;
#81613 = ORIENTED_EDGE ( 'NONE', *, *, #88684, .T. ) ;
#81614 = VERTEX_POINT ( 'NONE', #27264 ) ;
#81615 = ORIENTED_EDGE ( 'NONE', *, *, #94855, .T. ) ;
#81616 = ORIENTED_EDGE ( 'NONE', *, *, #18127, .T. ) ;
#81617 = ORIENTED_EDGE ( 'NONE', *, *, #61057, .T. ) ;
#81618 = DIRECTION ( 'NONE',  ( 0.000000000000000000, 1.000000000000000000, 0.000000000000000000 ) ) ;
#81619 = CARTESIAN_POINT ( 'NONE',  ( -12.69999999999999041, 2.500000000000000000, 3.983716857408420964 ) ) ;
#81620 = ORIENTED_EDGE ( 'NONE', *, *, #125952, .T. ) ;
#81621 = FACE_BOUND ( 'NONE', #119952, .T. ) ;
#81622 = CARTESIAN_POINT ( 'NONE',  ( 5.649999999999934630, 2.500000000000000000, -1.918653347947325782 ) ) ;
#81623 = ADVANCED_FACE ( 'NONE', ( #35181 ), #86706, .T. ) ;
#81624 = ORIENTED_EDGE ( 'NONE', *, *, #75287, .T. ) ;
#81625 = CARTESIAN_POINT ( 'NONE',  ( -9.800000000000006040, 2.500000000000000000, -4.676537180435974328 ) ) ;
#81626 = DIRECTION ( 'NONE',  ( -0.000000000000000000, 1.000000000000000000, -0.000000000000000000 ) ) ;
#81627 = DIRECTION ( 'NONE',  ( 0.000000000000000000, 1.000000000000000000, 0.000000000000000000 ) ) ;
#81628 = FACE_OUTER_BOUND ( 'NONE', #81771, .T. ) ;
#81629 = ORIENTED_EDGE ( 'NONE', *, *, #92381, .F. ) ;
#81630 = FACE_OUTER_BOUND ( 'NONE', #99459, .T. ) ;
#81631 = EDGE_CURVE ( 'NONE', #50586, #10571, #105833, .T. ) ;
#81632 = VECTOR ( 'NONE', #22986, 1000.000000000000000 ) ;
#81633 = ORIENTED_EDGE ( 'NONE', *, *, #87845, .F. ) ;
#81634 = B_SPLINE_SURFACE_WITH_KNOTS ( 'NONE', 3, 1, ( 
 ( #100517, #10830 ),
 ( #90709, #1037 ),
 ( #23912, #103755 ),
 ( #64459, #82179 ),
 ( #114218, #121444 ),
 ( #33100, #33717 ),
 ( #122111, #24543 ),
 ( #54011, #72372 ),
 ( #93286, #104394 ),
 ( #103102, #42261 ),
 ( #112924, #63833 ),
 ( #74298, #62550 ),
 ( #31795, #73630 ),
 ( #42927, #12132 ),
 ( #14698, #124028 ),
 ( #111644, #52081 ),
 ( #14055, #84095 ),
 ( #102464, #54632 ) ),
 .UNSPECIFIED., .F., .F., .F.,
 ( 4, 2, 2, 2, 2, 2, 2, 2, 4 ),
 ( 2, 2 ),
 ( 0.000000000000000000, 0.1249999999999999445, 0.2499999999999998890, 0.3749999999999999445, 0.5000000000000000000, 0.6250000000000000000, 0.7500000000000001110, 0.8750000000000000000, 1.000000000000000000 ),
 ( 0.000000000000000000, 1.000000000000000000 ),
 .UNSPECIFIED. ) ;
#81635 = VERTEX_POINT ( 'NONE', #71545 ) ;
#81636 = ORIENTED_EDGE ( 'NONE', *, *, #39741, .F. ) ;
#81637 = ADVANCED_FACE ( 'NONE', ( #101667 ), #92476, .T. ) ;
#81638 = DIRECTION ( 'NONE',  ( 0.4999999999999471534, 0.000000000000000000, 0.8660254037844692387 ) ) ;
#81639 = DIRECTION ( 'NONE',  ( 0.000000000000000000, -0.000000000000000000, 1.000000000000000000 ) ) ;
#81641 = ORIENTED_EDGE ( 'NONE', *, *, #21665, .F. ) ;
#81640 = EDGE_CURVE ( 'NONE', #31627, #181, #11490, .T. ) ;
#81642 = CARTESIAN_POINT ( 'NONE',  ( -7.499999999999976907, 12.50000000000000000, 4.395220292106234439 ) ) ;
#81644 = EDGE_CURVE ( 'NONE', #111547, #102327, #2810, .T. ) ;
#81643 = CIRCLE ( 'NONE', #77441, 0.09999999999999982514 ) ;
#81645 = LINE ( 'NONE', #12883, #28126 ) ;
#81646 = CARTESIAN_POINT ( 'NONE',  ( 10.19999999999991580, 2.500000000000000000, -0.3464101615137783474 ) ) ;
#81648 = EDGE_CURVE ( 'NONE', #16181, #118050, #70076, .T. ) ;
#81647 = DIRECTION ( 'NONE',  ( -0.000000000000000000, 1.000000000000000000, -0.000000000000000000 ) ) ;
#81649 = DIRECTION ( 'NONE',  ( 0.000000000000000000, 1.000000000000000000, 0.000000000000000000 ) ) ;
#81650 = ORIENTED_EDGE ( 'NONE', *, *, #101590, .T. ) ;
#81651 = DIRECTION ( 'NONE',  ( 0.000000000000000000, 0.000000000000000000, 1.000000000000000000 ) ) ;
#81652 = EDGE_LOOP ( 'NONE', ( #124645, #54487 ) ) ;
#81653 = DIRECTION ( 'NONE',  ( -0.000000000000000000, -1.000000000000000000, -0.000000000000000000 ) ) ;
#81654 = EDGE_CURVE ( 'NONE', #40083, #126577, #30293, .T. ) ;
#81655 = EDGE_CURVE ( 'NONE', #6702, #52447, #15672, .T. ) ;
#81656 = ORIENTED_EDGE ( 'NONE', *, *, #85308, .T. ) ;
#81657 = DIRECTION ( 'NONE',  ( 0.000000000000000000, -0.9999939076577903929, 0.003490651415223739937 ) ) ;
#81658 = ORIENTED_EDGE ( 'NONE', *, *, #77370, .T. ) ;
#81659 = DIRECTION ( 'NONE',  ( -0.000000000000000000, 1.000000000000000000, -0.000000000000000000 ) ) ;
#81660 = DIRECTION ( 'NONE',  ( 0.000000000000000000, 0.000000000000000000, -1.000000000000000000 ) ) ;
#81661 = DIRECTION ( 'NONE',  ( 0.000000000000000000, -0.9999939076577903929, 0.003490651415223739937 ) ) ;
#81662 = DIRECTION ( 'NONE',  ( 0.000000000000000000, 0.000000000000000000, 1.000000000000000000 ) ) ;
#81663 = CARTESIAN_POINT ( 'NONE',  ( 108.0000000000000142, 9.000000000000001776, 0.000000000000000000 ) ) ;
#81664 = VERTEX_POINT ( 'NONE', #21155 ) ;
#81665 = ORIENTED_EDGE ( 'NONE', *, *, #104429, .F. ) ;
#81666 = EDGE_LOOP ( 'NONE', ( #72526, #127490 ) ) ;
#81667 = CARTESIAN_POINT ( 'NONE',  ( -5.200000000000020606, 2.500000000000000000, 3.983716857408420964 ) ) ;
#81668 = FACE_OUTER_BOUND ( 'NONE', #37667, .T. ) ;
#81670 = DIRECTION ( 'NONE',  ( 0.8660254037844391517, 0.000000000000000000, -0.4999999999999992228 ) ) ;
#81669 = VECTOR ( 'NONE', #119204, 1000.000000000000000 ) ;
#81672 = ORIENTED_EDGE ( 'NONE', *, *, #22407, .T. ) ;
#81671 = EDGE_LOOP ( 'NONE', ( #111790, #129523, #129042, #41794 ) ) ;
#81673 = ORIENTED_EDGE ( 'NONE', *, *, #127487, .T. ) ;
#81674 = CIRCLE ( 'NONE', #35708, 0.09999999999999982514 ) ;
#81675 = CONICAL_SURFACE ( 'NONE', #25221, 0.1000000000000000056, 0.003490658503988666988 ) ;
#81676 = DIRECTION ( 'NONE',  ( 0.000000000000000000, 0.000000000000000000, 1.000000000000000000 ) ) ;
#81677 = EDGE_LOOP ( 'NONE', ( #43846, #108823 ) ) ;
#81678 = DIRECTION ( 'NONE',  ( 0.000000000000000000, 0.000000000000000000, 1.000000000000000000 ) ) ;
#81679 = DIRECTION ( 'NONE',  ( 0.000000000000000000, 0.000000000000000000, -1.000000000000000000 ) ) ;
#81680 = AXIS2_PLACEMENT_3D ( 'NONE', #119897, #71418, #69492 ) ;
#81681 = DIRECTION ( 'NONE',  ( -0.000000000000000000, -1.000000000000000000, -0.000000000000000000 ) ) ;
#81682 = FACE_OUTER_BOUND ( 'NONE', #59847, .T. ) ;
#81683 = DIRECTION ( 'NONE',  ( 0.000000000000000000, 0.000000000000000000, 1.000000000000000000 ) ) ;
#81684 = CARTESIAN_POINT ( 'NONE',  ( 8.149999999999923972, 2.500000000000000000, 2.511473670974873507 ) ) ;
#81685 = LINE ( 'NONE', #112453, #92785 ) ;
#81686 = CIRCLE ( 'NONE', #50383, 0.09999999999999982514 ) ;
#81687 = DIRECTION ( 'NONE',  ( 0.000000000000000000, 0.000000000000000000, 1.000000000000000000 ) ) ;
#81688 = EDGE_LOOP ( 'NONE', ( #62627, #60919, #115952, #13963 ) ) ;
#81689 = FACE_OUTER_BOUND ( 'NONE', #4276, .T. ) ;
#81690 = CARTESIAN_POINT ( 'NONE',  ( 26.75237029038351366, -2.962322469583595907, 2.722363819585612355 ) ) ;
#81691 = ORIENTED_EDGE ( 'NONE', *, *, #60800, .F. ) ;
#81692 = VERTEX_POINT ( 'NONE', #42100 ) ;
#81693 = CARTESIAN_POINT ( 'NONE',  ( 184.1093750003413732, 9.264065473108010111E-16, -7.564683531250000925 ) ) ;
#81694 = LINE ( 'NONE', #41157, #53192 ) ;
#81695 = CARTESIAN_POINT ( 'NONE',  ( 9.799999999999913669, 2.500000000000000000, 4.676537180435972552 ) ) ;
#81696 = CARTESIAN_POINT ( 'NONE',  ( -1.050000000000037792, 2.500000000000000000, 1.918653347947321564 ) ) ;
#81697 = DIRECTION ( 'NONE',  ( 0.000000000000000000, 0.000000000000000000, 1.000000000000000000 ) ) ;
#81698 = ADVANCED_FACE ( 'NONE', ( #67839 ), #69990, .T. ) ;
#81699 = CARTESIAN_POINT ( 'NONE',  ( -1.250000000000037526, 2.500000000000000000, -1.472243186433550122 ) ) ;
#81700 = DIRECTION ( 'NONE',  ( 0.000000000000000000, 0.000000000000000000, 1.000000000000000000 ) ) ;
#81701 = DIRECTION ( 'NONE',  ( 0.000000000000000000, 0.000000000000000000, 1.000000000000000000 ) ) ;
#81702 = DIRECTION ( 'NONE',  ( 0.000000000000000000, -0.9999939076577903929, 0.003490651415223739937 ) ) ;
#81703 = AXIS2_PLACEMENT_3D ( 'NONE', #88457, #89117, #107470 ) ;
#81704 = ORIENTED_EDGE ( 'NONE', *, *, #66899, .F. ) ;
#81706 = ORIENTED_EDGE ( 'NONE', *, *, #11738, .F. ) ;
#81705 = VECTOR ( 'NONE', #12770, 1000.000000000000000 ) ;
#81707 = ORIENTED_EDGE ( 'NONE', *, *, #73771, .T. ) ;
#81708 = ORIENTED_EDGE ( 'NONE', *, *, #85591, .F. ) ;
#81709 = CARTESIAN_POINT ( 'NONE',  ( 184.5000000000000000, 9.429780353434619030E-16, 7.699999999999999289 ) ) ;
#81710 = FACE_OUTER_BOUND ( 'NONE', #121000, .T. ) ;
#81711 = VECTOR ( 'NONE', #14122, 1000.000000000000000 ) ;
#81712 = AXIS2_PLACEMENT_3D ( 'NONE', #11172, #18427, #51128 ) ;
#81713 = EDGE_LOOP ( 'NONE', ( #50961, #82193, #49547, #28485 ) ) ;
#81714 = FACE_OUTER_BOUND ( 'NONE', #122783, .T. ) ;
#81715 = DIRECTION ( 'NONE',  ( -0.000000000000000000, 1.000000000000000000, -0.000000000000000000 ) ) ;
#81716 = FACE_OUTER_BOUND ( 'NONE', #5230, .T. ) ;
#81718 = ORIENTED_EDGE ( 'NONE', *, *, #101180, .T. ) ;
#81717 = CARTESIAN_POINT ( 'NONE',  ( -0.8500000000000390576, 2.500000000000000000, -2.165063509461101710 ) ) ;
#81719 = DIRECTION ( 'NONE',  ( 0.000000000000000000, -0.000000000000000000, 1.000000000000000000 ) ) ;
#81720 = DIRECTION ( 'NONE',  ( -4.274815082592931898E-19, -0.9999939076577903929, -0.003490651415223739937 ) ) ;
#81721 = AXIS2_PLACEMENT_3D ( 'NONE', #2512, #60820, #42479 ) ;
#81722 = ORIENTED_EDGE ( 'NONE', *, *, #89301, .F. ) ;
#81723 = AXIS2_PLACEMENT_3D ( 'NONE', #32528, #82902, #70491 ) ;
#81724 = ORIENTED_EDGE ( 'NONE', *, *, #75338, .T. ) ;
#81725 = ORIENTED_EDGE ( 'NONE', *, *, #120745, .F. ) ;
#81726 = ORIENTED_EDGE ( 'NONE', *, *, #84843, .T. ) ;
#81727 = FACE_OUTER_BOUND ( 'NONE', #58037, .T. ) ;
#81728 = CONICAL_SURFACE ( 'NONE', #106771, 0.1000000000000002554, 0.003490658503988666988 ) ;
#81729 = DIRECTION ( 'NONE',  ( -0.000000000000000000, 1.000000000000000000, -0.000000000000000000 ) ) ;
#81730 = LINE ( 'NONE', #12975, #96295 ) ;
#81731 = ADVANCED_FACE ( 'NONE', ( #107767 ), #70915, .T. ) ;
#81732 = VERTEX_POINT ( 'NONE', #82012 ) ;
#81733 = AXIS2_PLACEMENT_3D ( 'NONE', #73559, #4171, #42862 ) ;
#81734 = DIRECTION ( 'NONE',  ( 0.000000000000000000, -0.9999939076577903929, 0.003490651415223739937 ) ) ;
#81735 = ORIENTED_EDGE ( 'NONE', *, *, #30790, .F. ) ;
#81736 = DIRECTION ( 'NONE',  ( 0.000000000000000000, -0.000000000000000000, 1.000000000000000000 ) ) ;
#81737 = DIRECTION ( 'NONE',  ( 0.000000000000000000, 0.000000000000000000, 1.000000000000000000 ) ) ;
#81738 = EDGE_CURVE ( 'NONE', #76276, #29239, #2158, .T. ) ;
#81739 = DIRECTION ( 'NONE',  ( 0.000000000000000000, -0.000000000000000000, 1.000000000000000000 ) ) ;
#81740 = FACE_OUTER_BOUND ( 'NONE', #70342, .T. ) ;
#81741 = EDGE_CURVE ( 'NONE', #37231, #70629, #112132, .T. ) ;
#81742 = VERTEX_POINT ( 'NONE', #22478 ) ;
#81743 = VERTEX_POINT ( 'NONE', #51294 ) ;
#81744 = ADVANCED_FACE ( 'NONE', ( #28568 ), #12617, .T. ) ;
#81746 = ORIENTED_EDGE ( 'NONE', *, *, #49869, .F. ) ;
#81745 = EDGE_CURVE ( 'NONE', #127958, #80681, #20529, .T. ) ;
#81747 = DIRECTION ( 'NONE',  ( 0.000000000000000000, 1.000000000000000000, 0.000000000000000000 ) ) ;
#81748 = DIRECTION ( 'NONE',  ( 0.000000000000000000, 1.000000000000000000, 0.000000000000000000 ) ) ;
#81749 = EDGE_CURVE ( 'NONE', #102801, #70298, #101383, .T. ) ;
#81750 = FACE_BOUND ( 'NONE', #97876, .T. ) ;
#81751 = DIRECTION ( 'NONE',  ( 0.000000000000000000, -0.000000000000000000, 1.000000000000000000 ) ) ;
#81752 = DIRECTION ( 'NONE',  ( 0.000000000000000000, 0.000000000000000000, 1.000000000000000000 ) ) ;
#81753 = DIRECTION ( 'NONE',  ( 0.000000000000000000, -0.000000000000000000, 1.000000000000000000 ) ) ;
#81754 = AXIS2_PLACEMENT_3D ( 'NONE', #45805, #5211, #87002 ) ;
#81755 = CIRCLE ( 'NONE', #83906, 0.06509327318403745899 ) ;
#81757 = AXIS2_PLACEMENT_3D ( 'NONE', #101666, #59833, #81390 ) ;
#81756 = DIRECTION ( 'NONE',  ( 0.000000000000000000, -0.000000000000000000, 1.000000000000000000 ) ) ;
#81758 = CARTESIAN_POINT ( 'NONE',  ( -11.44999999999999751, 2.500000000000000000, 6.148780366869520897 ) ) ;
#81759 = DIRECTION ( 'NONE',  ( 0.000000000000000000, 1.000000000000000000, 0.000000000000000000 ) ) ;
#81760 = ORIENTED_EDGE ( 'NONE', *, *, #16789, .T. ) ;
#81761 = CARTESIAN_POINT ( 'NONE',  ( 10.64999999999991331, 2.500000000000000000, -1.818653347947325916 ) ) ;
#81762 = AXIS2_PLACEMENT_3D ( 'NONE', #23624, #52437, #2042 ) ;
#81763 = DIRECTION ( 'NONE',  ( 0.000000000000000000, -0.9999939076577903929, 0.003490651415223739937 ) ) ;
#81764 = VERTEX_POINT ( 'NONE', #18091 ) ;
#81765 = VERTEX_POINT ( 'NONE', #97943 ) ;
#81766 = CONICAL_SURFACE ( 'NONE', #90161, 0.1000000000000002554, 0.003490658503988666988 ) ;
#81767 = CARTESIAN_POINT ( 'NONE',  ( -5.400000000000019895, 2.500000000000000000, 3.737306695894644371 ) ) ;
#81768 = DIRECTION ( 'NONE',  ( 0.000000000000000000, 0.000000000000000000, 1.000000000000000000 ) ) ;
#81769 = FACE_BOUND ( 'NONE', #75710, .T. ) ;
#81770 = CARTESIAN_POINT ( 'NONE',  ( 7.899999999999923084, 2.500000000000000000, 0.5928203230275495006 ) ) ;
#81771 = EDGE_LOOP ( 'NONE', ( #67598, #60259, #104867, #37900 ) ) ;
#81773 = EDGE_CURVE ( 'NONE', #103770, #11509, #36646, .T. ) ;
#81772 = DIRECTION ( 'NONE',  ( 0.000000000000000000, 0.000000000000000000, 1.000000000000000000 ) ) ;
#81774 = CARTESIAN_POINT ( 'NONE',  ( 184.0833333333333144, -6.668395609140180369, 3.849999999999994760 ) ) ;
#81775 = ORIENTED_EDGE ( 'NONE', *, *, #64490, .F. ) ;
#81776 = CARTESIAN_POINT ( 'NONE',  ( 11.44999999999991047, 2.500000000000000000, -2.611473670974877592 ) ) ;
#81777 = CARTESIAN_POINT ( 'NONE',  ( -4.200000000000029488, 12.50000000000000000, -4.330127018922201643 ) ) ;
#81778 = EDGE_CURVE ( 'NONE', #47295, #113860, #63727, .T. ) ;
#81779 = ORIENTED_EDGE ( 'NONE', *, *, #79092, .F. ) ;
#81780 = EDGE_CURVE ( 'NONE', #39986, #41483, #7268, .T. ) ;
#81781 = CARTESIAN_POINT ( 'NONE',  ( -0.4500000000000397571, 2.500000000000000000, -6.595190528383302109 ) ) ;
#81782 = DIRECTION ( 'NONE',  ( -0.000000000000000000, 1.000000000000000000, -0.000000000000000000 ) ) ;
#81783 = EDGE_CURVE ( 'NONE', #106452, #39808, #105676, .T. ) ;
#81784 = CIRCLE ( 'NONE', #90098, 0.06509327318403745899 ) ;
#81785 = AXIS2_PLACEMENT_3D ( 'NONE', #61096, #89904, #69621 ) ;
#81786 = EDGE_LOOP ( 'NONE', ( #64558, #91558, #124934, #22656 ) ) ;
#81787 = DIRECTION ( 'NONE',  ( -0.000000000000000000, 1.000000000000000000, -0.000000000000000000 ) ) ;
#81788 = LINE ( 'NONE', #71997, #53912 ) ;
#81789 = CARTESIAN_POINT ( 'NONE',  ( -7.500000000000001776, 2.500000000000000000, 1.734723475976807094E-15 ) ) ;
#81790 = EDGE_CURVE ( 'NONE', #124254, #43141, #105528, .T. ) ;
#81791 = EDGE_LOOP ( 'NONE', ( #62753, #60442, #20174, #46966 ) ) ;
#81792 = ORIENTED_EDGE ( 'NONE', *, *, #27956, .F. ) ;
#81793 = ADVANCED_FACE ( 'NONE', ( #35507 ), #109883, .T. ) ;
#81794 = DIRECTION ( 'NONE',  ( 0.000000000000000000, 1.000000000000000000, 0.000000000000000000 ) ) ;
#81795 = VECTOR ( 'NONE', #9142, 1000.000000000000000 ) ;
#81797 = ORIENTED_EDGE ( 'NONE', *, *, #110352, .T. ) ;
#81796 = ADVANCED_FACE ( 'NONE', ( #53849 ), #47104, .T. ) ;
#81798 = CARTESIAN_POINT ( 'NONE',  ( -13.34999999999999076, 12.50000000000000000, 1.407149913249511997 ) ) ;
#81799 = CONICAL_SURFACE ( 'NONE', #92264, 0.1000000000000002554, 0.003490658503988666988 ) ;
#81800 = CARTESIAN_POINT ( 'NONE',  ( 1.899999999999951283, 12.50000000000000000, -4.676537180435977881 ) ) ;
#81801 = ADVANCED_FACE ( 'NONE', ( #115305 ), #57562, .T. ) ;
#81802 = EDGE_CURVE ( 'NONE', #62761, #93687, #107725, .T. ) ;
#81803 = LINE ( 'NONE', #35782, #92751 ) ;
#81804 = EDGE_LOOP ( 'NONE', ( #5431, #15325 ) ) ;
#81805 = CARTESIAN_POINT ( 'NONE',  ( 11.24999999999990941, 2.500000000000000000, -1.572243186433550211 ) ) ;
#81806 = DIRECTION ( 'NONE',  ( 0.000000000000000000, 0.000000000000000000, 1.000000000000000000 ) ) ;
#81807 = DIRECTION ( 'NONE',  ( -0.000000000000000000, -1.000000000000000000, -0.000000000000000000 ) ) ;
#81808 = FACE_OUTER_BOUND ( 'NONE', #24656, .T. ) ;
#81809 = FACE_OUTER_BOUND ( 'NONE', #101515, .T. ) ;
#81811 = ADVANCED_FACE ( 'NONE', ( #122591 ), #72241, .T. ) ;
#81810 = DIRECTION ( 'NONE',  ( 0.000000000000000000, 0.000000000000000000, 1.000000000000000000 ) ) ;
#81812 = AXIS2_PLACEMENT_3D ( 'NONE', #39755, #107822, #79647 ) ;
#81813 = EDGE_LOOP ( 'NONE', ( #115777, #506, #1137, #65283 ) ) ;
#81814 = AXIS2_PLACEMENT_3D ( 'NONE', #8821, #108323, #107020 ) ;
#81815 = ORIENTED_EDGE ( 'NONE', *, *, #25019, .F. ) ;
#81816 = DIRECTION ( 'NONE',  ( 0.000000000000000000, 1.000000000000000000, 0.000000000000000000 ) ) ;
#81817 = ORIENTED_EDGE ( 'NONE', *, *, #105742, .F. ) ;
#81818 = CARTESIAN_POINT ( 'NONE',  ( 102.9915580679601135, 7.705489964099487388, 0.005789880036570591894 ) ) ;
#81819 = CONICAL_SURFACE ( 'NONE', #37914, 0.1000000000000002554, 0.003490658503988666988 ) ;
#81821 = VERTEX_POINT ( 'NONE', #45328 ) ;
#81820 = EDGE_LOOP ( 'NONE', ( #86532, #128397 ) ) ;
#81822 = ORIENTED_EDGE ( 'NONE', *, *, #102143, .F. ) ;
#81823 = DIRECTION ( 'NONE',  ( 0.000000000000000000, -0.000000000000000000, 1.000000000000000000 ) ) ;
#81824 = DIRECTION ( 'NONE',  ( 0.000000000000000000, -0.000000000000000000, 1.000000000000000000 ) ) ;
#81825 = CARTESIAN_POINT ( 'NONE',  ( 9.149999999999918643, 2.500000000000000000, 2.165063509461097713 ) ) ;
#81826 = FACE_OUTER_BOUND ( 'NONE', #63932, .T. ) ;
#81827 = CIRCLE ( 'NONE', #111053, 0.09999999999999982514 ) ;
#81828 = CIRCLE ( 'NONE', #25383, 0.06509327318403745899 ) ;
#81829 = CARTESIAN_POINT ( 'NONE',  ( 8.949999999999915801, 2.500000000000000000, -1.718653347947326049 ) ) ;
#81830 = LINE ( 'NONE', #43229, #100872 ) ;
#81831 = FACE_OUTER_BOUND ( 'NONE', #98957, .T. ) ;
#81832 = DIRECTION ( 'NONE',  ( -0.000000000000000000, 1.000000000000000000, -0.000000000000000000 ) ) ;
#81833 = DIRECTION ( 'NONE',  ( 0.000000000000000000, 0.000000000000000000, 1.000000000000000000 ) ) ;
#81834 = ORIENTED_EDGE ( 'NONE', *, *, #8308, .T. ) ;
#81835 = CARTESIAN_POINT ( 'NONE',  ( -5.400000000000019895, 12.50000000000000000, 3.637306695894644726 ) ) ;
#81836 = ORIENTED_EDGE ( 'NONE', *, *, #4156, .F. ) ;
#81837 = ORIENTED_EDGE ( 'NONE', *, *, #94342, .T. ) ;
#81838 = DIRECTION ( 'NONE',  ( -0.000000000000000000, 1.000000000000000000, -0.000000000000000000 ) ) ;
#81839 = DIRECTION ( 'NONE',  ( 0.000000000000000000, 0.000000000000000000, -1.000000000000000000 ) ) ;
#81840 = FACE_OUTER_BOUND ( 'NONE', #41676, .T. ) ;
#81841 = DIRECTION ( 'NONE',  ( 0.000000000000000000, 0.000000000000000000, 1.000000000000000000 ) ) ;
#81842 = EDGE_CURVE ( 'NONE', #102321, #65003, #13906, .T. ) ;
#81843 = DIRECTION ( 'NONE',  ( -0.000000000000000000, -1.000000000000000000, -0.000000000000000000 ) ) ;
#81844 = DIRECTION ( 'NONE',  ( -4.274815082592931898E-19, -0.9999939076577903929, -0.003490651415223739937 ) ) ;
#81845 = AXIS2_PLACEMENT_3D ( 'NONE', #98177, #78568, #118460 ) ;
#81846 = FACE_OUTER_BOUND ( 'NONE', #5737, .T. ) ;
#81847 = ORIENTED_EDGE ( 'NONE', *, *, #113606, .F. ) ;
#81848 = CONICAL_SURFACE ( 'NONE', #125751, 0.1000000000000000472, 0.003490658503988666988 ) ;
#81849 = CONICAL_SURFACE ( 'NONE', #10820, 0.09999999999999982514, 0.003490658503988666988 ) ;
#81850 = ORIENTED_EDGE ( 'NONE', *, *, #85649, .F. ) ;
#81851 = CIRCLE ( 'NONE', #125757, 0.09999999999999999167 ) ;
#81852 = VERTEX_POINT ( 'NONE', #125166 ) ;
#81853 = AXIS2_PLACEMENT_3D ( 'NONE', #18063, #37083, #29208 ) ;
#81854 = ORIENTED_EDGE ( 'NONE', *, *, #2436, .F. ) ;
#81855 = AXIS2_PLACEMENT_3D ( 'NONE', #8231, #57998, #29190 ) ;
#81856 = EDGE_CURVE ( 'NONE', #108534, #38221, #30387, .T. ) ;
#81857 = VERTEX_POINT ( 'NONE', #65593 ) ;
#81858 = CARTESIAN_POINT ( 'NONE',  ( 5.799999999999934985, 2.500000000000000000, -4.230127018922201998 ) ) ;
#81859 = CARTESIAN_POINT ( 'NONE',  ( 1.899999999999949507, 2.500000000000000000, 4.083716857408421497 ) ) ;
#81860 = CONICAL_SURFACE ( 'NONE', #98577, 0.09999999999999982514, 0.003490658503988666988 ) ;
#81861 = LINE ( 'NONE', #11835, #29930 ) ;
#81862 = DIRECTION ( 'NONE',  ( -0.000000000000000000, 1.000000000000000000, -0.000000000000000000 ) ) ;
#81863 = CARTESIAN_POINT ( 'NONE',  ( 87.50000000000001421, -3.413194297214857897, 6.711110875543779386 ) ) ;
#81864 = ORIENTED_EDGE ( 'NONE', *, *, #15109, .F. ) ;
#81865 = DIRECTION ( 'NONE',  ( 0.000000000000000000, 0.000000000000000000, 1.000000000000000000 ) ) ;
#81866 = DIRECTION ( 'NONE',  ( 0.000000000000000000, 1.000000000000000000, 0.000000000000000000 ) ) ;
#81867 = DIRECTION ( 'NONE',  ( -0.000000000000000000, 1.000000000000000000, -0.000000000000000000 ) ) ;
#81868 = DIRECTION ( 'NONE',  ( 0.000000000000000000, 0.000000000000000000, 1.000000000000000000 ) ) ;
#81869 = FACE_OUTER_BOUND ( 'NONE', #31149, .T. ) ;
#81870 = VERTEX_POINT ( 'NONE', #72845 ) ;
#81871 = ORIENTED_EDGE ( 'NONE', *, *, #49014, .T. ) ;
#81872 = VERTEX_POINT ( 'NONE', #104234 ) ;
#81873 = DIRECTION ( 'NONE',  ( 0.000000000000000000, 1.000000000000000000, 0.000000000000000000 ) ) ;
#81874 = ORIENTED_EDGE ( 'NONE', *, *, #93620, .F. ) ;
#81875 = LINE ( 'NONE', #14423, #76013 ) ;
#81876 = DIRECTION ( 'NONE',  ( -1.000000000000000000, 0.000000000000000000, 0.000000000000000000 ) ) ;
#81877 = VECTOR ( 'NONE', #106802, 1000.000000000000000 ) ;
#81878 = ADVANCED_FACE ( 'NONE', ( #44677 ), #114686, .T. ) ;
#81879 = ORIENTED_EDGE ( 'NONE', *, *, #25569, .F. ) ;
#81880 = DIRECTION ( 'NONE',  ( 0.000000000000000000, 0.000000000000000000, 1.000000000000000000 ) ) ;
#81881 = CARTESIAN_POINT ( 'NONE',  ( -1.850000000000033396, 2.500000000000000000, -1.818653347947325916 ) ) ;
#81882 = DIRECTION ( 'NONE',  ( 0.000000000000000000, 0.000000000000000000, 1.000000000000000000 ) ) ;
#81883 = DIRECTION ( 'NONE',  ( -0.000000000000000000, 1.000000000000000000, -0.000000000000000000 ) ) ;
#81884 = AXIS2_PLACEMENT_3D ( 'NONE', #23474, #90929, #42489 ) ;
#81885 = ADVANCED_FACE ( 'NONE', ( #93772 ), #34590, .T. ) ;
#81886 = AXIS2_PLACEMENT_3D ( 'NONE', #127497, #47647, #78408 ) ;
#81887 = CARTESIAN_POINT ( 'NONE',  ( 9.349999999999916156, 2.500000000000000000, -1.818653347947326138 ) ) ;
#81888 = CIRCLE ( 'NONE', #90207, 0.09999999999999982514 ) ;
#81889 = VERTEX_POINT ( 'NONE', #34223 ) ;
#81890 = EDGE_CURVE ( 'NONE', #32820, #36161, #124452, .T. ) ;
#81891 = EDGE_CURVE ( 'NONE', #101973, #102305, #53454, .T. ) ;
#81892 =( BOUNDED_CURVE ( )  B_SPLINE_CURVE ( 2, ( #107701, #18015, #85475, #8196, #117479, #47495, #116857 ),
 .UNSPECIFIED., .F., .F. ) 
 B_SPLINE_CURVE_WITH_KNOTS ( ( 3, 2, 2, 3 ),
 ( 0.7142857142857148567, 0.7380952380952386926, 0.7619047619047624176, 0.7857142857142862535 ),
 .UNSPECIFIED. ) 
 CURVE ( )  GEOMETRIC_REPRESENTATION_ITEM ( )  RATIONAL_B_SPLINE_CURVE ( ( 0.9999999999999968914, 0.8660254037844418162, 1.000000000000000000, 0.8660254037844387076, 1.000000000000000000, 0.8660254037844355990, 1.000000000000003109 ) ) 
 REPRESENTATION_ITEM ( '' )  );
#81893 = EDGE_LOOP ( 'NONE', ( #121347, #86922, #60377, #23270 ) ) ;
#81894 = ADVANCED_FACE ( 'NONE', ( #114061 ), #111935, .T. ) ;
#81896 = ADVANCED_FACE ( 'NONE', ( #83933 ), #24105, .T. ) ;
#81895 = CARTESIAN_POINT ( 'NONE',  ( 2.099999999999949463, 2.500000000000000000, 0.6928203230275494784 ) ) ;
#81897 = EDGE_CURVE ( 'NONE', #88124, #18723, #40858, .T. ) ;
#81898 = CARTESIAN_POINT ( 'NONE',  ( 5.649999999999932854, 12.50000000000000000, 1.753560074763284016 ) ) ;
#81899 = CARTESIAN_POINT ( 'NONE',  ( -13.94999999999998863, 2.500000000000000000, -1.918653347947324006 ) ) ;
#81900 = CIRCLE ( 'NONE', #37998, 0.09999999999999982514 ) ;
#81902 = CARTESIAN_POINT ( 'NONE',  ( 4.799999999999937650, 2.500000000000000000, -3.983716857408426293 ) ) ;
#81901 = CIRCLE ( 'NONE', #56753, 0.09999999999999982514 ) ;
#81903 = EDGE_LOOP ( 'NONE', ( #12688, #36063, #116971, #12265 ) ) ;
#81904 = AXIS2_PLACEMENT_3D ( 'NONE', #37523, #77430, #8034 ) ;
#81905 = VECTOR ( 'NONE', #52547, 1000.000000000000000 ) ;
#81906 = CIRCLE ( 'NONE', #111147, 0.06509327318403745899 ) ;
#81907 = ORIENTED_EDGE ( 'NONE', *, *, #40358, .T. ) ;
#81908 = DIRECTION ( 'NONE',  ( -4.274815082592931898E-19, -0.9999939076577903929, -0.003490651415223739937 ) ) ;
#81909 = DIRECTION ( 'NONE',  ( 0.000000000000000000, 0.000000000000000000, 1.000000000000000000 ) ) ;
#81910 = ADVANCED_FACE ( 'NONE', ( #108088 ), #74285, .T. ) ;
#81911 = CIRCLE ( 'NONE', #44257, 0.1000000000000002554 ) ;
#81912 = DIRECTION ( 'NONE',  ( 0.000000000000000000, 0.000000000000000000, 1.000000000000000000 ) ) ;
#81913 = CARTESIAN_POINT ( 'NONE',  ( -3.750000000000025757, 12.50000000000000000, -2.792790559304616504 ) ) ;
#81914 = EDGE_LOOP ( 'NONE', ( #79464, #23543, #117508, #61173 ) ) ;
#81915 = EDGE_CURVE ( 'NONE', #84545, #2147, #93167, .T. ) ;
#81917 = ADVANCED_FACE ( 'NONE', ( #18430 ), #125784, .T. ) ;
#81916 = CARTESIAN_POINT ( 'NONE',  ( 186.5000000000000000, 0.000000000000000000, -5.000000000000000000 ) ) ;
#81918 = DIRECTION ( 'NONE',  ( 0.000000000000000000, 1.000000000000000000, 0.000000000000000000 ) ) ;
#81919 = EDGE_LOOP ( 'NONE', ( #92208, #22941 ) ) ;
#81920 = CARTESIAN_POINT ( 'NONE',  ( 10.84999999999991260, 12.50000000000000000, -2.230156782645139391 ) ) ;
#81921 = ORIENTED_EDGE ( 'NONE', *, *, #107038, .F. ) ;
#81922 = DIRECTION ( 'NONE',  ( 0.000000000000000000, 0.000000000000000000, 1.000000000000000000 ) ) ;
#81923 = ORIENTED_EDGE ( 'NONE', *, *, #121835, .F. ) ;
#81924 = DIRECTION ( 'NONE',  ( 1.000000000000000000, 0.000000000000000000, 1.776356839400247112E-15 ) ) ;
#81925 = LINE ( 'NONE', #91116, #25027 ) ;
#81926 = VERTEX_POINT ( 'NONE', #86514 ) ;
#81927 = ORIENTED_EDGE ( 'NONE', *, *, #90955, .T. ) ;
#81928 = DIRECTION ( 'NONE',  ( -4.274815082592931898E-19, -0.9999939076577903929, -0.003490651415223739937 ) ) ;
#81929 = CARTESIAN_POINT ( 'NONE',  ( -4.150000000000025224, 2.500000000000000000, 6.595190528383296780 ) ) ;
#81930 = CARTESIAN_POINT ( 'NONE',  ( 6.849999999999927702, 2.500000000000000000, 1.818653347947321475 ) ) ;
#81931 = CARTESIAN_POINT ( 'NONE',  ( 184.0260416670080588, -6.551208109652273848, -3.782341765625003571 ) ) ;
#81932 = DIRECTION ( 'NONE',  ( 0.000000000000000000, 1.000000000000000000, 0.000000000000000000 ) ) ;
#81933 = AXIS2_PLACEMENT_3D ( 'NONE', #124761, #23323, #62633 ) ;
#81934 = CARTESIAN_POINT ( 'NONE',  ( 0.5999999999999612310, 12.50000000000000000, -0.4115034346978134749 ) ) ;
#81935 = CARTESIAN_POINT ( 'NONE',  ( 2.099999999999950351, 2.500000000000000000, -4.922947341949753586 ) ) ;
#81936 = CIRCLE ( 'NONE', #40197, 0.1000000000000002554 ) ;
#81938 = ADVANCED_FACE ( 'NONE', ( #97633 ), #98269, .T. ) ;
#81937 = AXIS2_PLACEMENT_3D ( 'NONE', #127732, #78656, #129053 ) ;
#81939 = CARTESIAN_POINT ( 'NONE',  ( 14.14999999999989733, 2.500000000000000000, 2.857883832488649301 ) ) ;
#81940 = DIRECTION ( 'NONE',  ( 0.000000000000000000, 0.000000000000000000, -1.000000000000000000 ) ) ;
#81941 = CONICAL_SURFACE ( 'NONE', #35996, 0.1000000000000002554, 0.003490658503988666988 ) ;
#81943 = ORIENTED_EDGE ( 'NONE', *, *, #9965, .T. ) ;
#81942 = AXIS2_PLACEMENT_3D ( 'NONE', #91701, #23597, #3317 ) ;
#81944 = ADVANCED_FACE ( 'NONE', ( #7956 ), #78506, .T. ) ;
#81946 = EDGE_LOOP ( 'NONE', ( #9761, #32358, #110385, #37521 ) ) ;
#81945 = VECTOR ( 'NONE', #73609, 1000.000000000000000 ) ;
#81947 = CARTESIAN_POINT ( 'NONE',  ( -10.84999999999999964, 2.500000000000000000, 5.802370205355744659 ) ) ;
#81948 = ORIENTED_EDGE ( 'NONE', *, *, #3443, .F. ) ;
#81949 = CARTESIAN_POINT ( 'NONE',  ( -6.650000000000014566, 2.500000000000000000, 5.802370205355744659 ) ) ;
#81950 = CARTESIAN_POINT ( 'NONE',  ( 6.649999999999929301, 2.500000000000000000, -2.265063509461101798 ) ) ;
#81951 = AXIS2_PLACEMENT_3D ( 'NONE', #107583, #38206, #78785 ) ;
#81952 = DIRECTION ( 'NONE',  ( 0.000000000000000000, 1.000000000000000000, 0.000000000000000000 ) ) ;
#81955 = ORIENTED_EDGE ( 'NONE', *, *, #25960, .T. ) ;
#81954 = ORIENTED_EDGE ( 'NONE', *, *, #69191, .T. ) ;
#81953 = CONICAL_SURFACE ( 'NONE', #58991, 0.09999999999999982514, 0.003490658503988666988 ) ;
#81956 = FACE_BOUND ( 'NONE', #38794, .T. ) ;
#81957 = ORIENTED_EDGE ( 'NONE', *, *, #120492, .T. ) ;
#81958 = ADVANCED_FACE ( 'NONE', ( #17774 ), #26258, .T. ) ;
#81959 = DIRECTION ( 'NONE',  ( -0.000000000000000000, 1.000000000000000000, -0.000000000000000000 ) ) ;
#81960 = DIRECTION ( 'NONE',  ( 0.000000000000000000, -0.000000000000000000, 1.000000000000000000 ) ) ;
#81961 = EDGE_CURVE ( 'NONE', #101480, #86613, #45973, .T. ) ;
#81962 = PLANE ( 'NONE',  #7467 ) ;
#81963 = DIRECTION ( 'NONE',  ( 0.000000000000000000, 0.000000000000000000, 1.000000000000000000 ) ) ;
#81964 = DIRECTION ( 'NONE',  ( 0.000000000000000000, 0.000000000000000000, 1.000000000000000000 ) ) ;
#81965 = EDGE_CURVE ( 'NONE', #103567, #84006, #51317, .T. ) ;
#81966 = CARTESIAN_POINT ( 'NONE',  ( 5.199999999999933564, 12.50000000000000000, 0.2813168883297361700 ) ) ;
#81967 = FACE_OUTER_BOUND ( 'NONE', #105118, .T. ) ;
#81968 = DIRECTION ( 'NONE',  ( 0.000000000000000000, 1.000000000000000000, 0.000000000000000000 ) ) ;
#81969 = CARTESIAN_POINT ( 'NONE',  ( 5.649999999999932854, 2.500000000000000000, 1.818653347947321475 ) ) ;
#81970 = DIRECTION ( 'NONE',  ( -0.000000000000000000, 1.000000000000000000, -0.000000000000000000 ) ) ;
#81972 = EDGE_CURVE ( 'NONE', #38064, #83506, #115983, .T. ) ;
#81971 = DIRECTION ( 'NONE',  ( 0.000000000000000000, -0.000000000000000000, 1.000000000000000000 ) ) ;
#81973 = VERTEX_POINT ( 'NONE', #56413 ) ;
#81974 = EDGE_LOOP ( 'NONE', ( #42485, #116549 ) ) ;
#81975 = ORIENTED_EDGE ( 'NONE', *, *, #88403, .T. ) ;
#81976 = CARTESIAN_POINT ( 'NONE',  ( 6.849999999999927702, 2.500000000000000000, 2.511473670974873507 ) ) ;
#81977 = ORIENTED_EDGE ( 'NONE', *, *, #85769, .F. ) ;
#81978 = DIRECTION ( 'NONE',  ( -4.274815082592931898E-19, -0.9999939076577903929, -0.003490651415223739937 ) ) ;
#81979 = CARTESIAN_POINT ( 'NONE',  ( -2.100000000000033840, 2.500000000000000000, 3.637306695894644726 ) ) ;
#81981 = ORIENTED_EDGE ( 'NONE', *, *, #105638, .F. ) ;
#81980 = ORIENTED_EDGE ( 'NONE', *, *, #50281, .T. ) ;
#81982 = ORIENTED_EDGE ( 'NONE', *, *, #72016, .F. ) ;
#81983 = DIRECTION ( 'NONE',  ( 0.000000000000000000, 0.000000000000000000, 1.000000000000000000 ) ) ;
#81984 = CIRCLE ( 'NONE', #54784, 0.06509327318403745899 ) ;
#81985 = PLANE ( 'NONE',  #117811 ) ;
#81986 =( NAMED_UNIT ( * ) PLANE_ANGLE_UNIT ( ) SI_UNIT ( $, .RADIAN. ) );
#81987 = DIRECTION ( 'NONE',  ( -0.000000000000000000, 1.000000000000000000, -0.000000000000000000 ) ) ;
#81988 = DIRECTION ( 'NONE',  ( -0.000000000000000000, -1.000000000000000000, -0.000000000000000000 ) ) ;
#81989 = FACE_OUTER_BOUND ( 'NONE', #59707, .T. ) ;
#81990 = CARTESIAN_POINT ( 'NONE',  ( 2.949999999999945111, 12.50000000000000000, 2.165063509461097713 ) ) ;
#81991 = EDGE_CURVE ( 'NONE', #54491, #37534, #68011, .T. ) ;
#81992 = ORIENTED_EDGE ( 'NONE', *, *, #89306, .T. ) ;
#81993 = AXIS2_PLACEMENT_3D ( 'NONE', #62613, #60682, #33154 ) ;
#81994 = CIRCLE ( 'NONE', #2553, 0.06509327318403745899 ) ;
#81995 = CARTESIAN_POINT ( 'NONE',  ( 13.34999999999990017, 2.500000000000000000, 1.372243186433545370 ) ) ;
#81996 = VERTEX_POINT ( 'NONE', #36798 ) ;
#81997 = CONICAL_SURFACE ( 'NONE', #79844, 0.09999999999999982514, 0.003490658503988666988 ) ;
#81998 = ORIENTED_EDGE ( 'NONE', *, *, #4228, .F. ) ;
#81999 = AXIS2_PLACEMENT_3D ( 'NONE', #124709, #32490, #82209 ) ;
#82000 = EDGE_LOOP ( 'NONE', ( #103009, #37412 ) ) ;
#82001 = DIRECTION ( 'NONE',  ( 0.000000000000000000, 0.000000000000000000, 1.000000000000000000 ) ) ;
#82002 = ORIENTED_EDGE ( 'NONE', *, *, #38205, .T. ) ;
#82003 = EDGE_LOOP ( 'NONE', ( #16963, #7159, #18860, #42979 ) ) ;
#82004 = ORIENTED_EDGE ( 'NONE', *, *, #53414, .T. ) ;
#82005 = AXIS2_PLACEMENT_3D ( 'NONE', #106067, #115206, #106697 ) ;
#82006 = CARTESIAN_POINT ( 'NONE',  ( -7.900000000000014566, 12.50000000000000000, -5.088040615133791356 ) ) ;
#82007 = CIRCLE ( 'NONE', #125907, 0.09999999999999982514 ) ;
#82008 = FACE_OUTER_BOUND ( 'NONE', #38321, .T. ) ;
#82009 = ADVANCED_FACE ( 'NONE', ( #7302 ), #11576, .T. ) ;
#82010 = DIRECTION ( 'NONE',  ( 0.000000000000000000, 0.000000000000000000, 1.000000000000000000 ) ) ;
#82011 = VECTOR ( 'NONE', #105351, 1000.000000000000000 ) ;
#82012 = CARTESIAN_POINT ( 'NONE',  ( -5.000000000000022204, 12.50000000000000000, -0.7579135962115916003 ) ) ;
#82013 = CARTESIAN_POINT ( 'NONE',  ( -1.250000000000037526, 2.500000000000000000, -5.902370205355750521 ) ) ;
#82014 = AXIS2_PLACEMENT_3D ( 'NONE', #83396, #117818, #47823 ) ;
#82015 = DIRECTION ( 'NONE',  ( 0.000000000000000000, 1.000000000000000000, 0.000000000000000000 ) ) ;
#82016 = EDGE_LOOP ( 'NONE', ( #129235, #84950 ) ) ;
#82017 = CARTESIAN_POINT ( 'NONE',  ( 4.799999999999939426, 12.50000000000000000, -4.676537180435977881 ) ) ;
#82018 = ORIENTED_EDGE ( 'NONE', *, *, #20352, .T. ) ;
#82019 = DIRECTION ( 'NONE',  ( 0.000000000000000000, 1.000000000000000000, 0.000000000000000000 ) ) ;
#82020 = ORIENTED_EDGE ( 'NONE', *, *, #113933, .T. ) ;
#82021 = DIRECTION ( 'NONE',  ( 0.000000000000000000, 1.000000000000000000, 0.000000000000000000 ) ) ;
#82022 = ADVANCED_FACE ( 'NONE', ( #88444 ), #45048, .T. ) ;
#82023 = ORIENTED_EDGE ( 'NONE', *, *, #25295, .F. ) ;
#82024 = CARTESIAN_POINT ( 'NONE',  ( 184.1510416670080588, 4.367472073101518859, -7.564683531249999149 ) ) ;
#82025 = CARTESIAN_POINT ( 'NONE',  ( 14.79999999999989413, 12.50000000000000000, -0.4115034346978156399 ) ) ;
#82026 = ORIENTED_EDGE ( 'NONE', *, *, #22464, .F. ) ;
#82027 = EDGE_LOOP ( 'NONE', ( #40085, #25727, #59999, #30479 ) ) ;
#82028 = FACE_OUTER_BOUND ( 'NONE', #90058, .T. ) ;
#82029 = PLANE ( 'NONE',  #59734 ) ;
#82030 = DIRECTION ( 'NONE',  ( 0.000000000000000000, -0.9999939076577903929, 0.003490651415223739937 ) ) ;
#82031 = FACE_OUTER_BOUND ( 'NONE', #127681, .T. ) ;
#82032 = DIRECTION ( 'NONE',  ( -4.274815082592931898E-19, -0.9999939076577903929, -0.003490651415223739937 ) ) ;
#82033 = ORIENTED_EDGE ( 'NONE', *, *, #23540, .F. ) ;
#82034 = CARTESIAN_POINT ( 'NONE',  ( 2.500000000000002220, -1.500000000000000000, 10.00000000000000178 ) ) ;
#82035 = VECTOR ( 'NONE', #1317, 1000.000000000000000 ) ;
#82036 = CONICAL_SURFACE ( 'NONE', #102968, 0.1000000000000002554, 0.003490658503988666988 ) ;
#82037 = ORIENTED_EDGE ( 'NONE', *, *, #70845, .F. ) ;
#82038 = DIRECTION ( 'NONE',  ( 0.000000000000000000, -0.000000000000000000, 1.000000000000000000 ) ) ;
#82039 = DIRECTION ( 'NONE',  ( 0.000000000000000000, 0.000000000000000000, 1.000000000000000000 ) ) ;
#82040 = AXIS2_PLACEMENT_3D ( 'NONE', #15671, #103435, #115822 ) ;
#82041 = AXIS2_PLACEMENT_3D ( 'NONE', #57426, #124233, #45038 ) ;
#82043 = ADVANCED_FACE ( 'NONE', ( #118555 ), #20000, .T. ) ;
#82042 = VECTOR ( 'NONE', #14036, 1000.000000000000000 ) ;
#82044 = CIRCLE ( 'NONE', #59075, 0.06509327318403745899 ) ;
#82045 = CIRCLE ( 'NONE', #466, 0.09999999999999982514 ) ;
#82046 = CARTESIAN_POINT ( 'NONE',  ( 186.4635416670080872, -4.367472073101519747, 7.564683531249999149 ) ) ;
#82047 = LINE ( 'NONE', #61790, #128410 ) ;
#82048 = DIRECTION ( 'NONE',  ( -4.274815082592931898E-19, -0.9999939076577903929, -0.003490651415223739937 ) ) ;
#82049 = CARTESIAN_POINT ( 'NONE',  ( -5.400000000000020783, 12.50000000000000000, 0.6277270498435120194 ) ) ;
#82050 = FACE_OUTER_BOUND ( 'NONE', #102649, .T. ) ;
#82051 = ORIENTED_EDGE ( 'NONE', *, *, #20204, .T. ) ;
#82052 = AXIS2_PLACEMENT_3D ( 'NONE', #90066, #393, #69139 ) ;
#82053 = ADVANCED_FACE ( 'NONE', ( #68816 ), #107532, .T. ) ;
#82054 = CARTESIAN_POINT ( 'NONE',  ( -11.25000000000000178, 12.50000000000000000, -5.802370205355746435 ) ) ;
#82055 = CARTESIAN_POINT ( 'NONE',  ( -4.999999999999986677, 12.50000000000000000, 4.330127018922196314 ) ) ;
#82056 = CARTESIAN_POINT ( 'NONE',  ( 3.099999999999945022, 12.50000000000000000, -4.676537180435978769 ) ) ;
#82057 = ORIENTED_EDGE ( 'NONE', *, *, #125513, .F. ) ;
#82058 = ADVANCED_FACE ( 'NONE', ( #66231 ), #74086, .T. ) ;
#82059 = EDGE_CURVE ( 'NONE', #31935, #53009, #128479, .T. ) ;
#82060 = EDGE_CURVE ( 'NONE', #104225, #39846, #96988, .T. ) ;
#82061 = EDGE_CURVE ( 'NONE', #83059, #127177, #39391, .T. ) ;
#82062 = ORIENTED_EDGE ( 'NONE', *, *, #76033, .T. ) ;
#82063 = DIRECTION ( 'NONE',  ( 0.000000000000000000, 0.000000000000000000, -1.000000000000000000 ) ) ;
#82064 = VECTOR ( 'NONE', #65799, 1000.000000000000000 ) ;
#82065 = EDGE_LOOP ( 'NONE', ( #14157, #20130 ) ) ;
#82066 = ORIENTED_EDGE ( 'NONE', *, *, #34924, .T. ) ;
#82067 = DIRECTION ( 'NONE',  ( -0.000000000000000000, -1.000000000000000000, -0.000000000000000000 ) ) ;
#82068 = EDGE_CURVE ( 'NONE', #87872, #64350, #121139, .T. ) ;
#82069 = EDGE_CURVE ( 'NONE', #93103, #50389, #99583, .T. ) ;
#82070 = ORIENTED_EDGE ( 'NONE', *, *, #80598, .T. ) ;
#82071 = CARTESIAN_POINT ( 'NONE',  ( 16.72050902516516757, -2.552201582241029332, -5.918448581785260565 ) ) ;
#82072 = PLANE ( 'NONE',  #2727 ) ;
#82073 = EDGE_CURVE ( 'NONE', #112141, #126712, #28118, .T. ) ;
#82074 = CARTESIAN_POINT ( 'NONE',  ( 16.09541403888798783, 2.463474929527698531, 3.723514363710399344 ) ) ;
#82075 = AXIS2_PLACEMENT_3D ( 'NONE', #87986, #25870, #17972 ) ;
#82076 = ORIENTED_EDGE ( 'NONE', *, *, #113564, .T. ) ;
#82078 = EDGE_CURVE ( 'NONE', #103138, #1435, #86588, .T. ) ;
#82077 = AXIS2_PLACEMENT_3D ( 'NONE', #103838, #4310, #66475 ) ;
#82079 = AXIS2_PLACEMENT_3D ( 'NONE', #73414, #121238, #4026 ) ;
#82081 = EDGE_CURVE ( 'NONE', #68676, #61297, #120058, .T. ) ;
#82080 = CARTESIAN_POINT ( 'NONE',  ( 195.5000000000000000, 6.123233995736766282E-16, 5.000000000000000000 ) ) ;
#82082 = CARTESIAN_POINT ( 'NONE',  ( -2.100000000000033396, 12.50000000000000000, 0.6928203230275494784 ) ) ;
#82084 = ADVANCED_FACE ( 'NONE', ( #110668 ), #7170, .T. ) ;
#82083 = AXIS2_PLACEMENT_3D ( 'NONE', #123761, #33485, #74038 ) ;
#82085 = ORIENTED_EDGE ( 'NONE', *, *, #84386, .T. ) ;
#82086 = CONICAL_SURFACE ( 'NONE', #61162, 0.09999999999999982514, 0.003490658503988666988 ) ;
#82087 = AXIS2_PLACEMENT_3D ( 'NONE', #44057, #84632, #102970 ) ;
#82088 = ORIENTED_EDGE ( 'NONE', *, *, #9385, .T. ) ;
#82089 = ORIENTED_EDGE ( 'NONE', *, *, #38031, .T. ) ;
#82090 = CARTESIAN_POINT ( 'NONE',  ( -3.350000000000031619, 12.50000000000000000, -7.122917578226816815 ) ) ;
#82091 = CARTESIAN_POINT ( 'NONE',  ( -4.400000000000025224, 2.500000000000000000, 0.3464101615137735735 ) ) ;
#82092 = DIRECTION ( 'NONE',  ( 1.000000000000000000, 0.000000000000000000, 0.000000000000000000 ) ) ;
#82093 = FACE_BOUND ( 'NONE', #56815, .T. ) ;
#82094 = VERTEX_POINT ( 'NONE', #20369 ) ;
#82095 = CARTESIAN_POINT ( 'NONE',  ( -0.6500000000000398792, 12.50000000000000000, -2.511473670974877948 ) ) ;
#82096 = DIRECTION ( 'NONE',  ( 0.000000000000000000, 0.000000000000000000, -1.000000000000000000 ) ) ;
#82097 = CIRCLE ( 'NONE', #67393, 0.09999999999999982514 ) ;
#82098 = EDGE_LOOP ( 'NONE', ( #103742, #43075, #15976, #14635 ) ) ;
#82099 = AXIS2_PLACEMENT_3D ( 'NONE', #121065, #9822, #60857 ) ;
#82100 = CARTESIAN_POINT ( 'NONE',  ( 8.549999999999918998, 12.50000000000000000, 6.776507416713035248 ) ) ;
#82101 = DIRECTION ( 'NONE',  ( 0.000000000000000000, 0.000000000000000000, 1.000000000000000000 ) ) ;
#82102 = VECTOR ( 'NONE', #90197, 1000.000000000000000 ) ;
#82103 = CONICAL_SURFACE ( 'NONE', #19397, 0.1000000000000002554, 0.003490658503988666988 ) ;
#82104 = AXIS2_PLACEMENT_3D ( 'NONE', #98233, #89707, #33 ) ;
#82105 = DIRECTION ( 'NONE',  ( 0.000000000000000000, -0.000000000000000000, 1.000000000000000000 ) ) ;
#82106 = CARTESIAN_POINT ( 'NONE',  ( 10.19999999999991225, 12.50000000000000000, 4.048810130592458201 ) ) ;
#82107 = DIRECTION ( 'NONE',  ( 0.000000000000000000, -1.000000000000000000, -0.000000000000000000 ) ) ;
#82108 = PLANE ( 'NONE',  #63949 ) ;
#82109 = AXIS2_PLACEMENT_3D ( 'NONE', #13671, #1920, #43169 ) ;
#82110 = DIRECTION ( 'NONE',  ( 0.000000000000000000, 0.000000000000000000, 1.000000000000000000 ) ) ;
#82111 = VERTEX_POINT ( 'NONE', #89746 ) ;
#82112 = AXIS2_PLACEMENT_3D ( 'NONE', #22748, #32571, #50261 ) ;
#82113 = ORIENTED_EDGE ( 'NONE', *, *, #89257, .F. ) ;
#82114 = ORIENTED_EDGE ( 'NONE', *, *, #94428, .F. ) ;
#82115 = EDGE_LOOP ( 'NONE', ( #12609, #43319 ) ) ;
#82116 = LINE ( 'NONE', #12080, #3549 ) ;
#82117 = CARTESIAN_POINT ( 'NONE',  ( 3.749999999999938716, 2.500000000000000000, 7.288010851410849256 ) ) ;
#82118 = LINE ( 'NONE', #111578, #29985 ) ;
#82119 = ORIENTED_EDGE ( 'NONE', *, *, #83446, .T. ) ;
#82120 = FACE_BOUND ( 'NONE', #41391, .T. ) ;
#82121 = FACE_OUTER_BOUND ( 'NONE', #110250, .T. ) ;
#82122 = DIRECTION ( 'NONE',  ( 0.000000000000000000, -0.9999939076577903929, 0.003490651415223739937 ) ) ;
#82123 = EDGE_CURVE ( 'NONE', #19888, #74443, #78307, .T. ) ;
#82124 = CARTESIAN_POINT ( 'NONE',  ( 107.5000000000000142, 0.000000000000000000, -2.000000000000000000 ) ) ;
#82125 = CARTESIAN_POINT ( 'NONE',  ( -0.2000000000000399791, 12.50000000000000000, -4.611443907251939756 ) ) ;
#82126 = EDGE_CURVE ( 'NONE', #51796, #47551, #60926, .T. ) ;
#82127 = CARTESIAN_POINT ( 'NONE',  ( -9.550000000000006040, 2.500000000000000000, 2.065063509461097624 ) ) ;
#82128 = CARTESIAN_POINT ( 'NONE',  ( 6.849999999999927702, 12.50000000000000000, 1.883746621131358934 ) ) ;
#82129 = CARTESIAN_POINT ( 'NONE',  ( 11.44999999999990514, 2.500000000000000000, 2.411473670974873862 ) ) ;
#82130 = LINE ( 'NONE', #72961, #9474 ) ;
#82131 = CONICAL_SURFACE ( 'NONE', #54926, 0.09999999999999982514, 0.003490658503988666988 ) ;
#82132 = CONICAL_SURFACE ( 'NONE', #65392, 0.09999999999999982514, 0.003490658503988666988 ) ;
#82133 = DIRECTION ( 'NONE',  ( -4.274815082592931898E-19, -0.9999939076577903929, -0.003490651415223739937 ) ) ;
#82134 = EDGE_CURVE ( 'NONE', #49056, #107837, #120352, .T. ) ;
#82135 = VERTEX_POINT ( 'NONE', #11175 ) ;
#82137 = EDGE_CURVE ( 'NONE', #64505, #39552, #36452, .T. ) ;
#82136 = AXIS2_PLACEMENT_3D ( 'NONE', #93497, #86226, #44385 ) ;
#82138 = ORIENTED_EDGE ( 'NONE', *, *, #81406, .F. ) ;
#82139 = ORIENTED_EDGE ( 'NONE', *, *, #97756, .F. ) ;
#82140 = VERTEX_POINT ( 'NONE', #9900 ) ;
#82141 = AXIS2_PLACEMENT_3D ( 'NONE', #83405, #8517, #7226 ) ;
#82142 = ORIENTED_EDGE ( 'NONE', *, *, #67280, .F. ) ;
#82143 = VERTEX_POINT ( 'NONE', #22320 ) ;
#82144 = AXIS2_PLACEMENT_3D ( 'NONE', #116789, #109567, #58545 ) ;
#82145 = CARTESIAN_POINT ( 'NONE',  ( 129.5000000000000000, 0.000000000000000000, 0.000000000000000000 ) ) ;
#82146 = ORIENTED_EDGE ( 'NONE', *, *, #35540, .F. ) ;
#82147 = ORIENTED_EDGE ( 'NONE', *, *, #38257, .T. ) ;
#82148 = CIRCLE ( 'NONE', #69618, 0.06509327318403745899 ) ;
#82149 = AXIS2_PLACEMENT_3D ( 'NONE', #41671, #81568, #3016 ) ;
#82150 = AXIS2_PLACEMENT_3D ( 'NONE', #4258, #92021, #2326 ) ;
#82151 = DIRECTION ( 'NONE',  ( 0.000000000000000000, 0.000000000000000000, 1.000000000000000000 ) ) ;
#82152 = LINE ( 'NONE', #81511, #33010 ) ;
#82153 = DIRECTION ( 'NONE',  ( 0.000000000000000000, 0.000000000000000000, -1.000000000000000000 ) ) ;
#82154 = CARTESIAN_POINT ( 'NONE',  ( 12.69999999999990159, 2.500000000000000000, 4.576537180435972019 ) ) ;
#82155 = CONICAL_SURFACE ( 'NONE', #8969, 0.1000000000000002554, 0.003490658503988666988 ) ;
#82156 = AXIS2_PLACEMENT_3D ( 'NONE', #22784, #103263, #81678 ) ;
#82157 = EDGE_LOOP ( 'NONE', ( #120567, #119256 ) ) ;
#82158 = LINE ( 'NONE', #61229, #119514 ) ;
#82159 = CIRCLE ( 'NONE', #128232, 0.06509327318403745899 ) ;
#82160 = ORIENTED_EDGE ( 'NONE', *, *, #79204, .F. ) ;
#82161 = ORIENTED_EDGE ( 'NONE', *, *, #55346, .T. ) ;
#82162 = DIRECTION ( 'NONE',  ( 0.000000000000000000, 1.000000000000000000, 0.000000000000000000 ) ) ;
#82163 = CARTESIAN_POINT ( 'NONE',  ( 6.249999999999932498, 2.500000000000000000, 5.702370205355745014 ) ) ;
#82164 = VERTEX_POINT ( 'NONE', #98921 ) ;
#82165 = EDGE_LOOP ( 'NONE', ( #96717, #46126, #34232, #13738 ) ) ;
#82166 = AXIS2_PLACEMENT_3D ( 'NONE', #72906, #64993, #44744 ) ;
#82167 = ADVANCED_FACE ( 'NONE', ( #11823 ), #68, .T. ) ;
#82168 = CARTESIAN_POINT ( 'NONE',  ( 10.64999999999991331, 2.500000000000000000, 6.148780366869520897 ) ) ;
#82169 = DIRECTION ( 'NONE',  ( 0.000000000000000000, -0.9999939076577903929, 0.003490651415223739937 ) ) ;
#82170 = FACE_OUTER_BOUND ( 'NONE', #6137, .T. ) ;
#82171 = CARTESIAN_POINT ( 'NONE',  ( 13.34999999999989662, 2.500000000000000000, -1.472243186433550122 ) ) ;
#82172 = LINE ( 'NONE', #21307, #108760 ) ;
#82174 = EDGE_LOOP ( 'NONE', ( #19241, #97779, #7616, #64856 ) ) ;
#82173 = CIRCLE ( 'NONE', #34060, 0.06509327318403745899 ) ;
#82175 = LINE ( 'NONE', #122109, #46919 ) ;
#82176 = VECTOR ( 'NONE', #44772, 1000.000000000000000 ) ;
#82177 = MECHANICAL_DESIGN_GEOMETRIC_PRESENTATION_REPRESENTATION (  '', ( #124026 ), #90576 ) ;
#82178 = ORIENTED_EDGE ( 'NONE', *, *, #63753, .F. ) ;
#82179 = CARTESIAN_POINT ( 'NONE',  ( 17.50000000000000000, 2.499999999999999556, 2.666666666666668739 ) ) ;
#82180 = DIRECTION ( 'NONE',  ( 0.000000000000000000, 0.000000000000000000, -1.000000000000000000 ) ) ;
#82181 = DIRECTION ( 'NONE',  ( -0.000000000000000000, 1.000000000000000000, -0.000000000000000000 ) ) ;
#82182 = EDGE_CURVE ( 'NONE', #13197, #6403, #49204, .T. ) ;
#82183 = CARTESIAN_POINT ( 'NONE',  ( -7.500000000000013323, 2.500000000000000000, 5.022947341949748790 ) ) ;
#82184 = EDGE_CURVE ( 'NONE', #65087, #43418, #90805, .T. ) ;
#82186 = CIRCLE ( 'NONE', #36127, 0.06509327318403745899 ) ;
#82185 = FACE_OUTER_BOUND ( 'NONE', #125771, .T. ) ;
#82187 = VERTEX_POINT ( 'NONE', #129054 ) ;
#82188 = CIRCLE ( 'NONE', #88519, 0.09999999999999982514 ) ;
#82189 = CONICAL_SURFACE ( 'NONE', #94797, 0.1000000000000002554, 0.003490658503988666988 ) ;
#82190 = CARTESIAN_POINT ( 'NONE',  ( 5.649999999999934630, 12.50000000000000000, 6.841600689897072485 ) ) ;
#82191 = CONICAL_SURFACE ( 'NONE', #98908, 0.1000000000000002554, 0.003490658503988666988 ) ;
#82192 = CARTESIAN_POINT ( 'NONE',  ( -11.84999999999999787, 2.500000000000000000, -2.611473670974873595 ) ) ;
#82193 = ORIENTED_EDGE ( 'NONE', *, *, #17803, .T. ) ;
#82194 = EDGE_LOOP ( 'NONE', ( #60484, #19439 ) ) ;
#82196 = EDGE_LOOP ( 'NONE', ( #129593, #121286, #71676, #4552 ) ) ;
#82195 = ADVANCED_FACE ( 'NONE', ( #119210 ), #69882, .T. ) ;
#82197 = CARTESIAN_POINT ( 'NONE',  ( 17.50000000000000000, -0.9166666666666678509, 10.00000000000000178 ) ) ;
#82198 = FACE_OUTER_BOUND ( 'NONE', #101659, .T. ) ;
#82199 = CARTESIAN_POINT ( 'NONE',  ( 187.3177083336747444, 4.367472073101515306, 7.564683531250000925 ) ) ;
#82200 = CARTESIAN_POINT ( 'NONE',  ( 9.399999999999915090, 12.50000000000000000, 3.983716857408420964 ) ) ;
#82201 = CARTESIAN_POINT ( 'NONE',  ( -6.850000000000017408, 2.500000000000000000, -1.718653347947325827 ) ) ;
#82202 = CARTESIAN_POINT ( 'NONE',  ( -12.09999999999999609, 12.50000000000000000, -4.395220292106237103 ) ) ;
#82203 = AXIS2_PLACEMENT_3D ( 'NONE', #119409, #78880, #38972 ) ;
#82204 = CARTESIAN_POINT ( 'NONE',  ( 2.049999999999948308, 2.500000000000000000, 6.595190528383296780 ) ) ;
#82205 = CIRCLE ( 'NONE', #90594, 0.06509327318403745899 ) ;
#82206 = AXIS2_PLACEMENT_3D ( 'NONE', #97433, #109844, #119646 ) ;
#82207 = CARTESIAN_POINT ( 'NONE',  ( -5.600000000000023626, 12.50000000000000000, -3.918623584224389056 ) ) ;
#82208 = CIRCLE ( 'NONE', #71745, 0.06509327318403745899 ) ;
#82209 = DIRECTION ( 'NONE',  ( 0.000000000000000000, 0.000000000000000000, 1.000000000000000000 ) ) ;
#82210 = AXIS2_PLACEMENT_3D ( 'NONE', #113690, #33211, #53485 ) ;
#82211 = ORIENTED_EDGE ( 'NONE', *, *, #101434, .F. ) ;
#82212 = FACE_OUTER_BOUND ( 'NONE', #23108, .T. ) ;
#82213 = CARTESIAN_POINT ( 'NONE',  ( -2.300000000000033573, 2.500000000000000000, 0.3464101615137735735 ) ) ;
#82214 = CARTESIAN_POINT ( 'NONE',  ( 11.24999999999990585, 12.50000000000000000, -5.802370205355749988 ) ) ;
#82215 = CARTESIAN_POINT ( 'NONE',  ( -8.550000000000014921, 2.500000000000000000, -6.148780366869520897 ) ) ;
#82216 = VERTEX_POINT ( 'NONE', #70116 ) ;
#82217 = DIRECTION ( 'NONE',  ( 0.000000000000000000, 0.000000000000000000, -1.000000000000000000 ) ) ;
#82218 = EDGE_CURVE ( 'NONE', #111323, #111265, #110040, .T. ) ;
#82219 = CARTESIAN_POINT ( 'NONE',  ( -1.450000000000035039, 2.500000000000000000, -2.511473670974877948 ) ) ;
#82221 = ORIENTED_EDGE ( 'NONE', *, *, #109075, .F. ) ;
#82220 = CARTESIAN_POINT ( 'NONE',  ( -13.54999999999998828, 12.50000000000000000, 1.883746621131362931 ) ) ;
#82222 = CIRCLE ( 'NONE', #17446, 0.06509327318403743123 ) ;
#82223 = VECTOR ( 'NONE', #111911, 1000.000000000000000 ) ;
#82224 = EDGE_CURVE ( 'NONE', #65883, #12959, #11382, .T. ) ;
#82225 = ADVANCED_FACE ( 'NONE', ( #53690 ), #19713, .T. ) ;
#82226 = EDGE_CURVE ( 'NONE', #82230, #106895, #13430, .T. ) ;
#82227 = EDGE_LOOP ( 'NONE', ( #61291, #38828 ) ) ;
#82228 = CARTESIAN_POINT ( 'NONE',  ( 11.04999999999991189, 2.500000000000000000, 6.148780366869520897 ) ) ;
#82229 = AXIS2_PLACEMENT_3D ( 'NONE', #124079, #93983, #124726 ) ;
#82230 = VERTEX_POINT ( 'NONE', #94903 ) ;
#82231 = VECTOR ( 'NONE', #95474, 1000.000000000000000 ) ;
#82232 = ORIENTED_EDGE ( 'NONE', *, *, #2939, .T. ) ;
#82233 = DIRECTION ( 'NONE',  ( 0.000000000000000000, 1.000000000000000000, 0.000000000000000000 ) ) ;
#82234 = CONICAL_SURFACE ( 'NONE', #86417, 0.1000000000000002554, 0.003490658503988666988 ) ;
#82235 = ADVANCED_FACE ( 'NONE', ( #14390 ), #55308, .T. ) ;
#82236 = AXIS2_PLACEMENT_3D ( 'NONE', #66249, #45345, #43426 ) ;
#82237 = EDGE_CURVE ( 'NONE', #64702, #66161, #112619, .T. ) ;
#82238 = DIRECTION ( 'NONE',  ( -0.000000000000000000, -1.000000000000000000, -0.000000000000000000 ) ) ;
#82239 = PLANE ( 'NONE',  #14981 ) ;
#82240 = DIRECTION ( 'NONE',  ( 0.000000000000000000, 0.000000000000000000, -1.000000000000000000 ) ) ;
#82242 = ORIENTED_EDGE ( 'NONE', *, *, #36160, .T. ) ;
#82241 = CIRCLE ( 'NONE', #21698, 0.06509327318403745899 ) ;
#82243 = VECTOR ( 'NONE', #69589, 1000.000000000000000 ) ;
#82244 = AXIS2_PLACEMENT_3D ( 'NONE', #53243, #102338, #2840 ) ;
#82245 = EDGE_CURVE ( 'NONE', #98256, #81821, #88754, .T. ) ;
#82246 = CARTESIAN_POINT ( 'NONE',  ( -2.900000000000029221, 2.500000000000000000, -5.022947341949754119 ) ) ;
#82248 = ORIENTED_EDGE ( 'NONE', *, *, #128652, .F. ) ;
#82247 = AXIS2_PLACEMENT_3D ( 'NONE', #75073, #126094, #34523 ) ;
#82249 = VECTOR ( 'NONE', #85862, 1000.000000000000000 ) ;
#82250 = DIRECTION ( 'NONE',  ( -0.000000000000000000, 1.000000000000000000, -0.000000000000000000 ) ) ;
#82251 = EDGE_CURVE ( 'NONE', #24335, #90263, #83165, .T. ) ;
#82252 = DIRECTION ( 'NONE',  ( -4.274815082592931898E-19, -0.9999939076577903929, -0.003490651415223739937 ) ) ;
#82253 = EDGE_CURVE ( 'NONE', #117879, #77488, #61583, .T. ) ;
#82254 = AXIS2_PLACEMENT_3D ( 'NONE', #49859, #31492, #79322 ) ;
#82255 = ORIENTED_EDGE ( 'NONE', *, *, #119744, .F. ) ;
#82256 = ORIENTED_EDGE ( 'NONE', *, *, #57574, .F. ) ;
#82257 = ORIENTED_EDGE ( 'NONE', *, *, #89579, .T. ) ;
#82258 = ORIENTED_EDGE ( 'NONE', *, *, #115339, .F. ) ;
#82259 = DIRECTION ( 'NONE',  ( 0.000000000000000000, 1.000000000000000000, 0.000000000000000000 ) ) ;
#82260 = CARTESIAN_POINT ( 'NONE',  ( 14.37945523737839082, 2.499999999999745981, 7.667852709070308137 ) ) ;
#82261 = CARTESIAN_POINT ( 'NONE',  ( -3.550000000000028244, 2.500000000000000000, -1.818653347947326138 ) ) ;
#82262 = FACE_BOUND ( 'NONE', #111379, .T. ) ;
#82263 = VERTEX_POINT ( 'NONE', #113242 ) ;
#82264 = CARTESIAN_POINT ( 'NONE',  ( 185.1562500006828031, 8.891194145520236347, 5.444286225454521982E-16 ) ) ;
#82265 = DIRECTION ( 'NONE',  ( -0.000000000000000000, -1.000000000000000000, -0.000000000000000000 ) ) ;
#82266 = DIRECTION ( 'NONE',  ( -0.000000000000000000, 1.000000000000000000, -0.000000000000000000 ) ) ;
#82267 = CIRCLE ( 'NONE', #78156, 0.1000000000000002554 ) ;
#82268 = FACE_OUTER_BOUND ( 'NONE', #5017, .T. ) ;
#82269 = CARTESIAN_POINT ( 'NONE',  ( -5.850000000000018296, 12.50000000000000000, 1.537336459617582918 ) ) ;
#82270 = UNCERTAINTY_MEASURE_WITH_UNIT (LENGTH_MEASURE( 1.000000000000000082E-05 ), #92961, 'distance_accuracy_value', 'NONE');
#82271 = CYLINDRICAL_SURFACE ( 'NONE', #65803, 7.700000000000000178 ) ;
#82272 = VECTOR ( 'NONE', #30736, 1000.000000000000000 ) ;
#82273 = AXIS2_PLACEMENT_3D ( 'NONE', #98353, #17865, #29623 ) ;
#82274 = AXIS2_PLACEMENT_3D ( 'NONE', #99160, #19279, #59246 ) ;
#82275 = CARTESIAN_POINT ( 'NONE',  ( -13.09999999999999254, 12.50000000000000000, -3.983716857408423628 ) ) ;
#82276 = EDGE_LOOP ( 'NONE', ( #72259, #77095, #113463, #125754 ) ) ;
#82277 = VERTEX_POINT ( 'NONE', #83789 ) ;
#82278 = VERTEX_POINT ( 'NONE', #4549 ) ;
#82279 = EDGE_LOOP ( 'NONE', ( #69164, #101477 ) ) ;
#82280 = ORIENTED_EDGE ( 'NONE', *, *, #36423, .T. ) ;
#82281 = DIRECTION ( 'NONE',  ( 0.000000000000000000, 1.000000000000000000, 0.000000000000000000 ) ) ;
#82282 = DIRECTION ( 'NONE',  ( 0.000000000000000000, 0.000000000000000000, -1.000000000000000000 ) ) ;
#82283 = EDGE_LOOP ( 'NONE', ( #116632, #80118 ) ) ;
#82284 = FACE_BOUND ( 'NONE', #47050, .T. ) ;
#82285 = AXIS2_PLACEMENT_3D ( 'NONE', #50163, #37753, #78979 ) ;
#82286 = FACE_OUTER_BOUND ( 'NONE', #55760, .T. ) ;
#82287 = AXIS2_PLACEMENT_3D ( 'NONE', #126080, #71334, #58652 ) ;
#82288 = ADVANCED_FACE ( 'NONE', ( #124372 ), #30478, .T. ) ;
#82289 = ADVANCED_FACE ( 'NONE', ( #5221 ), #97349, .T. ) ;
#82290 = EDGE_LOOP ( 'NONE', ( #49996, #20969 ) ) ;
#82291 = DIRECTION ( 'NONE',  ( -1.000000000000000000, 0.000000000000000000, 0.000000000000000000 ) ) ;
#82292 = DIRECTION ( 'NONE',  ( 0.000000000000000000, 0.000000000000000000, 1.000000000000000000 ) ) ;
#82293 = PLANE ( 'NONE',  #126925 ) ;
#82294 = CONICAL_SURFACE ( 'NONE', #36342, 0.09999999999999999167, 0.003490658503988666988 ) ;
#82295 = ORIENTED_EDGE ( 'NONE', *, *, #104336, .F. ) ;
#82296 = CARTESIAN_POINT ( 'NONE',  ( -10.84999999999999964, 2.500000000000000000, 5.702370205355745014 ) ) ;
#82297 = ORIENTED_EDGE ( 'NONE', *, *, #22526, .T. ) ;
#82298 = AXIS2_PLACEMENT_3D ( 'NONE', #106236, #95767, #16537 ) ;
#82299 = AXIS2_PLACEMENT_3D ( 'NONE', #21837, #82021, #110833 ) ;
#82300 = AXIS2_PLACEMENT_3D ( 'NONE', #85532, #14827, #34522 ) ;
#82301 = ORIENTED_EDGE ( 'NONE', *, *, #32334, .T. ) ;
#82302 = ORIENTED_EDGE ( 'NONE', *, *, #34812, .F. ) ;
#82303 = DIRECTION ( 'NONE',  ( -0.000000000000000000, -1.000000000000000000, -0.000000000000000000 ) ) ;
#82304 = PLANE ( 'NONE',  #33073 ) ;
#82306 = VECTOR ( 'NONE', #11440, 1000.000000000000000 ) ;
#82305 = DIRECTION ( 'NONE',  ( -0.000000000000000000, 1.000000000000000000, -0.000000000000000000 ) ) ;
#82307 = VERTEX_POINT ( 'NONE', #114528 ) ;
#82308 = DIRECTION ( 'NONE',  ( -0.000000000000000000, -1.000000000000000000, -0.000000000000000000 ) ) ;
#82309 = CIRCLE ( 'NONE', #15372, 0.06509327318403745899 ) ;
#82310 = DIRECTION ( 'NONE',  ( 0.000000000000000000, 0.000000000000000000, 1.000000000000000000 ) ) ;
#82311 = DIRECTION ( 'NONE',  ( 0.000000000000000000, 1.000000000000000000, 0.000000000000000000 ) ) ;
#82312 = DIRECTION ( 'NONE',  ( -0.000000000000000000, 1.000000000000000000, -0.000000000000000000 ) ) ;
#82313 = DIRECTION ( 'NONE',  ( -0.000000000000000000, -1.000000000000000000, -0.000000000000000000 ) ) ;
#82314 = ORIENTED_EDGE ( 'NONE', *, *, #85629, .F. ) ;
#82315 = FACE_OUTER_BOUND ( 'NONE', #27183, .T. ) ;
#82316 = ORIENTED_EDGE ( 'NONE', *, *, #18960, .T. ) ;
#82317 = DIRECTION ( 'NONE',  ( 0.000000000000000000, 0.000000000000000000, 1.000000000000000000 ) ) ;
#82318 = EDGE_LOOP ( 'NONE', ( #51698, #80584 ) ) ;
#82319 = ORIENTED_EDGE ( 'NONE', *, *, #104981, .F. ) ;
#82320 = CARTESIAN_POINT ( 'NONE',  ( 4.149999999999941735, 2.500000000000000000, -2.757883832488654097 ) ) ;
#82321 = DIRECTION ( 'NONE',  ( 0.000000000000000000, 0.000000000000000000, 1.000000000000000000 ) ) ;
#82322 = AXIS2_PLACEMENT_3D ( 'NONE', #41145, #9079, #1193 ) ;
#82323 = CARTESIAN_POINT ( 'NONE',  ( -12.29999999999999538, 2.500000000000000000, -0.2464101615137742063 ) ) ;
#82324 = VECTOR ( 'NONE', #115099, 1000.000000000000000 ) ;
#82325 = CARTESIAN_POINT ( 'NONE',  ( 12.09999999999990550, 2.500000000000000000, 4.230127018922196669 ) ) ;
#82326 = CARTESIAN_POINT ( 'NONE',  ( 9.349999999999919709, 12.50000000000000000, 1.883746621131358934 ) ) ;
#82327 = VERTEX_POINT ( 'NONE', #24876 ) ;
#82328 = ORIENTED_EDGE ( 'NONE', *, *, #47169, .F. ) ;
#82329 = ADVANCED_FACE ( 'NONE', ( #45170 ), #53053, .T. ) ;
#82330 = DIRECTION ( 'NONE',  ( 0.000000000000000000, 1.000000000000000000, 0.000000000000000000 ) ) ;
#82331 = VECTOR ( 'NONE', #74836, 1000.000000000000000 ) ;
#82332 = AXIS2_PLACEMENT_3D ( 'NONE', #105860, #6984, #67859 ) ;
#82333 = CIRCLE ( 'NONE', #101201, 0.06509327318403745899 ) ;
#82334 = CARTESIAN_POINT ( 'NONE',  ( 186.5000000000000000, 0.000000000000000000, -4.000000000000000000 ) ) ;
#82335 = AXIS2_PLACEMENT_3D ( 'NONE', #12749, #110329, #31146 ) ;
#82337 = CARTESIAN_POINT ( 'NONE',  ( 8.099999999999923261, 2.500000000000000000, 4.676537180435972552 ) ) ;
#82336 = CONICAL_SURFACE ( 'NONE', #96990, 0.09999999999999982514, 0.003490658503988666988 ) ;
#82338 = ORIENTED_EDGE ( 'NONE', *, *, #94451, .F. ) ;
#82339 = EDGE_LOOP ( 'NONE', ( #104675, #9041, #62094, #39171 ) ) ;
#82340 = ADVANCED_FACE ( 'NONE', ( #104706 ), #64146, .T. ) ;
#82341 = CARTESIAN_POINT ( 'NONE',  ( 14.34999999999989662, 12.50000000000000000, 1.818653347947321475 ) ) ;
#82342 = ORIENTED_EDGE ( 'NONE', *, *, #33121, .T. ) ;
#82344 = ADVANCED_FACE ( 'NONE', ( #92982 ), #35347, .T. ) ;
#82343 = DIRECTION ( 'NONE',  ( 0.000000000000000000, 0.000000000000000000, 1.000000000000000000 ) ) ;
#82345 = DIRECTION ( 'NONE',  ( 0.000000000000000000, 1.000000000000000000, 0.000000000000000000 ) ) ;
#82346 = AXIS2_PLACEMENT_3D ( 'NONE', #21532, #90248, #586 ) ;
#82347 = AXIS2_PLACEMENT_3D ( 'NONE', #76042, #4690, #45948 ) ;
#82348 = CONICAL_SURFACE ( 'NONE', #38437, 0.1000000000000000472, 0.003490658503988666988 ) ;
#82349 = CARTESIAN_POINT ( 'NONE',  ( -2.700000000000029932, 2.500000000000000000, -0.3464101615137782364 ) ) ;
#82350 = ORIENTED_EDGE ( 'NONE', *, *, #76312, .F. ) ;
#82351 = DIRECTION ( 'NONE',  ( 0.000000000000000000, -0.000000000000000000, 1.000000000000000000 ) ) ;
#82352 = LINE ( 'NONE', #81056, #44541 ) ;
#82353 = DIRECTION ( 'NONE',  ( 0.000000000000000000, 1.000000000000000000, 0.000000000000000000 ) ) ;
#82354 = CARTESIAN_POINT ( 'NONE',  ( -10.60000000000000320, 2.500000000000000000, -4.676537180435973440 ) ) ;
#82355 = VECTOR ( 'NONE', #43248, 1000.000000000000000 ) ;
#82356 = EDGE_CURVE ( 'NONE', #69398, #91341, #113799, .T. ) ;
#82357 = EDGE_CURVE ( 'NONE', #43167, #80186, #46753, .T. ) ;
#82358 = DIRECTION ( 'NONE',  ( 0.000000000000000000, 1.000000000000000000, 0.000000000000000000 ) ) ;
#82359 = ORIENTED_EDGE ( 'NONE', *, *, #87414, .F. ) ;
#82360 = DIRECTION ( 'NONE',  ( -0.000000000000000000, 1.000000000000000000, -0.000000000000000000 ) ) ;
#82361 = PLANE ( 'NONE',  #102075 ) ;
#82362 = ORIENTED_EDGE ( 'NONE', *, *, #73614, .T. ) ;
#82363 = ORIENTED_EDGE ( 'NONE', *, *, #121501, .T. ) ;
#82364 = EDGE_CURVE ( 'NONE', #53599, #11772, #16315, .T. ) ;
#82365 = CARTESIAN_POINT ( 'NONE',  ( 184.4843750003414016, -8.734944146203032389, -1.604583208406768146E-15 ) ) ;
#82366 = DIRECTION ( 'NONE',  ( 0.000000000000000000, 0.000000000000000000, -1.000000000000000000 ) ) ;
#82367 = CARTESIAN_POINT ( 'NONE',  ( -2.950000000000029932, 2.500000000000000000, 2.165063509461097713 ) ) ;
#82368 = CIRCLE ( 'NONE', #25919, 0.09999999999999982514 ) ;
#82369 = DIRECTION ( 'NONE',  ( 0.000000000000000000, 1.000000000000000000, 0.000000000000000000 ) ) ;
#82370 = DIRECTION ( 'NONE',  ( 0.000000000000000000, 1.000000000000000000, 0.000000000000000000 ) ) ;
#82371 = DIRECTION ( 'NONE',  ( 0.000000000000000000, 1.000000000000000000, 0.000000000000000000 ) ) ;
#82372 = DIRECTION ( 'NONE',  ( -0.000000000000000000, 1.000000000000000000, -0.000000000000000000 ) ) ;
#82373 = PLANE ( 'NONE',  #91666 ) ;
#82374 = B_SPLINE_CURVE_WITH_KNOTS ( 'NONE', 3,
 ( #129588, #11055, #39909, #58894, #121029, #30741, #31374, #40562, #101400, #80483, #121665, #32026 ),
 .UNSPECIFIED., .F., .F.,
 ( 4, 2, 2, 2, 2, 4 ),
 ( 3.476216610979977084E-18, 0.001300228439403502360, 0.002600456878807001250, 0.003900685318210500574, 0.004550799537912254139, 0.005200913757614008572 ),
 .UNSPECIFIED. ) ;
#82376 = AXIS2_PLACEMENT_3D ( 'NONE', #85167, #55705, #36075 ) ;
#82375 = DIRECTION ( 'NONE',  ( -4.274815082592931898E-19, -0.9999939076577903929, -0.003490651415223739937 ) ) ;
#82377 = ORIENTED_EDGE ( 'NONE', *, *, #11407, .T. ) ;
#82378 = VECTOR ( 'NONE', #66141, 1000.000000000000000 ) ;
#82379 = EDGE_LOOP ( 'NONE', ( #18139, #66842 ) ) ;
#82380 = EDGE_LOOP ( 'NONE', ( #122904, #77397, #63921, #66375 ) ) ;
#82381 = EDGE_LOOP ( 'NONE', ( #93438, #19287, #58394, #80735 ) ) ;
#82382 = AXIS2_PLACEMENT_3D ( 'NONE', #118315, #21400, #32541 ) ;
#82383 = LINE ( 'NONE', #70611, #85899 ) ;
#82384 = DIRECTION ( 'NONE',  ( -0.000000000000000000, 1.000000000000000000, -0.000000000000000000 ) ) ;
#82385 = CIRCLE ( 'NONE', #65636, 0.06509327318403741736 ) ;
#82386 = ORIENTED_EDGE ( 'NONE', *, *, #85625, .T. ) ;
#82387 = DIRECTION ( 'NONE',  ( -0.000000000000000000, 1.000000000000000000, -0.000000000000000000 ) ) ;
#82388 = CIRCLE ( 'NONE', #71924, 0.06509327318403745899 ) ;
#82389 = EDGE_CURVE ( 'NONE', #49015, #48086, #17618, .T. ) ;
#82390 = DIRECTION ( 'NONE',  ( 0.000000000000000000, 1.000000000000000000, 0.000000000000000000 ) ) ;
#82392 = ORIENTED_EDGE ( 'NONE', *, *, #129062, .T. ) ;
#82391 = DIRECTION ( 'NONE',  ( 0.000000000000000000, 0.000000000000000000, -1.000000000000000000 ) ) ;
#82393 = ADVANCED_FACE ( 'NONE', ( #87645 ), #126301, .T. ) ;
#82394 = CARTESIAN_POINT ( 'NONE',  ( 7.899999999999924860, 2.500000000000000000, -3.637306695894650055 ) ) ;
#82395 = EDGE_CURVE ( 'NONE', #1004, #53300, #84641, .T. ) ;
#82396 = CARTESIAN_POINT ( 'NONE',  ( 7.899999999999923084, 12.50000000000000000, -0.7579135962115917113 ) ) ;
#82397 = VERTEX_POINT ( 'NONE', #18270 ) ;
#82398 = AXIS2_PLACEMENT_3D ( 'NONE', #15904, #85295, #106856 ) ;
#82399 = AXIS2_PLACEMENT_3D ( 'NONE', #91333, #29841, #10199 ) ;
#82400 = EDGE_LOOP ( 'NONE', ( #70585, #97626 ) ) ;
#82401 = EDGE_LOOP ( 'NONE', ( #19951, #33921 ) ) ;
#82402 = EDGE_LOOP ( 'NONE', ( #128694, #34657, #43764, #60436 ) ) ;
#82403 = DIRECTION ( 'NONE',  ( 0.000000000000000000, 0.000000000000000000, -1.000000000000000000 ) ) ;
#82404 = EDGE_CURVE ( 'NONE', #79607, #120619, #101374, .T. ) ;
#82405 = ADVANCED_FACE ( 'NONE', ( #96823 ), #1013, .T. ) ;
#82406 = AXIS2_PLACEMENT_3D ( 'NONE', #118013, #59109, #116719 ) ;
#82407 = ADVANCED_FACE ( 'NONE', ( #126948 ), #90899, .T. ) ;
#82408 = ADVANCED_FACE ( 'NONE', ( #16944 ), #11479, .T. ) ;
#82409 = DIRECTION ( 'NONE',  ( 0.000000000000000000, 0.000000000000000000, 1.000000000000000000 ) ) ;
#82410 = DIRECTION ( 'NONE',  ( 0.000000000000000000, 0.000000000000000000, 1.000000000000000000 ) ) ;
#82411 = CONICAL_SURFACE ( 'NONE', #122108, 0.1000000000000002554, 0.003490658503988666988 ) ;
#82412 = DIRECTION ( 'NONE',  ( 0.000000000000000000, 1.000000000000000000, 0.000000000000000000 ) ) ;
#82413 = ORIENTED_EDGE ( 'NONE', *, *, #124652, .T. ) ;
#82414 = EDGE_CURVE ( 'NONE', #41903, #98295, #97162, .T. ) ;
#82415 = LINE ( 'NONE', #1254, #83691 ) ;
#82416 = VERTEX_POINT ( 'NONE', #75900 ) ;
#82417 = FACE_OUTER_BOUND ( 'NONE', #122331, .T. ) ;
#82418 = CARTESIAN_POINT ( 'NONE',  ( -8.350000000000013856, 2.500000000000000000, -2.165063509461101710 ) ) ;
#82419 = DIRECTION ( 'NONE',  ( 0.000000000000000000, -0.9999939076577903929, 0.003490651415223739937 ) ) ;
#82420 = DIRECTION ( 'NONE',  ( -0.000000000000000000, -1.000000000000000000, -0.000000000000000000 ) ) ;
#82421 = EDGE_CURVE ( 'NONE', #58918, #71342, #15677, .T. ) ;
#82422 = ORIENTED_EDGE ( 'NONE', *, *, #11145, .T. ) ;
#82423 = ORIENTED_EDGE ( 'NONE', *, *, #26059, .T. ) ;
#82424 = EDGE_LOOP ( 'NONE', ( #66244, #7537 ) ) ;
#82425 = CARTESIAN_POINT ( 'NONE',  ( 6.649999999999930189, 12.50000000000000000, -2.922977105672691422 ) ) ;
#82426 = DIRECTION ( 'NONE',  ( -0.000000000000000000, -1.000000000000000000, -0.000000000000000000 ) ) ;
#82427 = DIRECTION ( 'NONE',  ( -0.000000000000000000, -1.000000000000000000, -0.000000000000000000 ) ) ;
#82428 = FACE_BOUND ( 'NONE', #79526, .T. ) ;
#82429 = PLANE ( 'NONE',  #38949 ) ;
#82430 = CARTESIAN_POINT ( 'NONE',  ( 9.399999999999915090, 2.500000000000000000, -4.576537180435977348 ) ) ;
#82431 = CARTESIAN_POINT ( 'NONE',  ( 11.84999999999990727, 2.500000000000000000, 6.741600689897071952 ) ) ;
#82432 = CIRCLE ( 'NONE', #30200, 0.06509327318403745899 ) ;
#82433 = AXIS2_PLACEMENT_3D ( 'NONE', #81558, #59359, #11521 ) ;
#82434 = VECTOR ( 'NONE', #3496, 1000.000000000000000 ) ;
#82435 = CONICAL_SURFACE ( 'NONE', #21794, 0.1000000000000002554, 0.003490658503988666988 ) ;
#82436 = CARTESIAN_POINT ( 'NONE',  ( 187.2135416670080303, 4.367472073101518859, -7.564683531249999149 ) ) ;
#82437 = DIRECTION ( 'NONE',  ( 0.000000000000000000, 0.000000000000000000, 1.000000000000000000 ) ) ;
#82438 = CARTESIAN_POINT ( 'NONE',  ( -7.500000000000001776, 2.500000000000000000, -9.000000000000000000 ) ) ;
#82439 = ORIENTED_EDGE ( 'NONE', *, *, #97775, .F. ) ;
#82441 = CARTESIAN_POINT ( 'NONE',  ( 4.599999999999938360, 12.50000000000000000, -0.6928203230275541413 ) ) ;
#82440 = CIRCLE ( 'NONE', #82136, 0.06509327318403745899 ) ;
#82442 = AXIS2_PLACEMENT_3D ( 'NONE', #118398, #28748, #68657 ) ;
#82443 = AXIS2_PLACEMENT_3D ( 'NONE', #49933, #88533, #38834 ) ;
#82444 = DIRECTION ( 'NONE',  ( -0.000000000000000000, -1.000000000000000000, -0.000000000000000000 ) ) ;
#82445 = ORIENTED_EDGE ( 'NONE', *, *, #51808, .F. ) ;
#82446 = ORIENTED_EDGE ( 'NONE', *, *, #82073, .T. ) ;
#82447 = CIRCLE ( 'NONE', #3011, 0.1000000000000000472 ) ;
#82448 = CARTESIAN_POINT ( 'NONE',  ( 1.449999999999952216, 2.500000000000000000, 1.818653347947321475 ) ) ;
#82449 = DIRECTION ( 'NONE',  ( 0.000000000000000000, 0.000000000000000000, -1.000000000000000000 ) ) ;
#82450 = FACE_BOUND ( 'NONE', #76842, .T. ) ;
#82451 = CARTESIAN_POINT ( 'NONE',  ( -0.8500000000000386136, 2.500000000000000000, 5.702370205355745014 ) ) ;
#82452 = EDGE_CURVE ( 'NONE', #109690, #45787, #55396, .T. ) ;
#82453 = VERTEX_POINT ( 'NONE', #77827 ) ;
#82454 = CARTESIAN_POINT ( 'NONE',  ( -12.04999999999999716, 12.50000000000000000, -6.560283801567336148 ) ) ;
#82455 = CARTESIAN_POINT ( 'NONE',  ( -4.200000000000029488, 2.500000000000000000, -4.330127018922201643 ) ) ;
#82457 = ORIENTED_EDGE ( 'NONE', *, *, #126681, .T. ) ;
#82456 = VECTOR ( 'NONE', #97532, 1000.000000000000000 ) ;
#82458 = CARTESIAN_POINT ( 'NONE',  ( 0.8499999999999536815, 12.50000000000000000, 6.495190528383297135 ) ) ;
#82459 = CARTESIAN_POINT ( 'NONE',  ( 11.44999999999990692, 2.500000000000000000, 1.818653347947321475 ) ) ;
#82460 = EDGE_CURVE ( 'NONE', #75963, #92171, #66717, .T. ) ;
#82461 = ORIENTED_EDGE ( 'NONE', *, *, #84315, .F. ) ;
#82462 = FACE_OUTER_BOUND ( 'NONE', #70130, .T. ) ;
#82463 = DIRECTION ( 'NONE',  ( -0.000000000000000000, 1.000000000000000000, -0.000000000000000000 ) ) ;
#82464 = CIRCLE ( 'NONE', #71994, 0.1000000000000000056 ) ;
#82465 = ORIENTED_EDGE ( 'NONE', *, *, #16327, .F. ) ;
#82466 = CARTESIAN_POINT ( 'NONE',  ( -7.050000000000013145, 2.500000000000000000, 6.495190528383297135 ) ) ;
#82467 = DIRECTION ( 'NONE',  ( -0.000000000000000000, 1.000000000000000000, -0.000000000000000000 ) ) ;
#82468 = CARTESIAN_POINT ( 'NONE',  ( -7.100000000000017408, 12.50000000000000000, -0.6277270498435167934 ) ) ;
#82469 = VERTEX_POINT ( 'NONE', #47109 ) ;
#82470 = EDGE_LOOP ( 'NONE', ( #4113, #122579, #73096, #128873 ) ) ;
#82471 = DIRECTION ( 'NONE',  ( 0.000000000000000000, -0.9999939076577903929, 0.003490651415223739937 ) ) ;
#82472 = EDGE_LOOP ( 'NONE', ( #83224, #19523 ) ) ;
#82473 = DIRECTION ( 'NONE',  ( 0.000000000000000000, 1.000000000000000000, 0.000000000000000000 ) ) ;
#82474 = DIRECTION ( 'NONE',  ( -0.000000000000000000, 1.000000000000000000, -0.000000000000000000 ) ) ;
#82475 = AXIS2_PLACEMENT_3D ( 'NONE', #89948, #29122, #82063 ) ;
#82476 = CARTESIAN_POINT ( 'NONE',  ( 3.349999999999944578, 2.500000000000000000, -1.572243186433550211 ) ) ;
#82477 = ORIENTED_EDGE ( 'NONE', *, *, #113582, .F. ) ;
#82478 = CARTESIAN_POINT ( 'NONE',  ( -13.74999999999998757, 2.500000000000000000, 1.372243186433549367 ) ) ;
#82479 = FACE_OUTER_BOUND ( 'NONE', #42402, .T. ) ;
#82480 = CARTESIAN_POINT ( 'NONE',  ( 11.64999999999990798, 2.500000000000000000, -2.857883832488653741 ) ) ;
#82481 = CARTESIAN_POINT ( 'NONE',  ( -12.69999999999999041, 2.500000000000000000, 3.883716857408421319 ) ) ;
#82482 = CARTESIAN_POINT ( 'NONE',  ( 6.699999999999930012, 2.500000000000000000, -4.230127018922201998 ) ) ;
#82483 = CARTESIAN_POINT ( 'NONE',  ( 11.24999999999990763, 12.50000000000000000, -7.122917578226816815 ) ) ;
#82484 = VERTEX_POINT ( 'NONE', #67336 ) ;
#82486 = EDGE_LOOP ( 'NONE', ( #35717, #67899 ) ) ;
#82485 = EDGE_CURVE ( 'NONE', #112225, #69443, #103426, .T. ) ;
#82487 = DIRECTION ( 'NONE',  ( 0.000000000000000000, 0.000000000000000000, 1.000000000000000000 ) ) ;
#82488 = EDGE_LOOP ( 'NONE', ( #25140, #14666, #29667, #51078 ) ) ;
#82489 = AXIS2_PLACEMENT_3D ( 'NONE', #116873, #27217, #65188 ) ;
#82490 = DIRECTION ( 'NONE',  ( 0.000000000000000000, 0.000000000000000000, 1.000000000000000000 ) ) ;
#82492 = ORIENTED_EDGE ( 'NONE', *, *, #60539, .F. ) ;
#82491 = ORIENTED_EDGE ( 'NONE', *, *, #90344, .T. ) ;
#82493 = ORIENTED_EDGE ( 'NONE', *, *, #10106, .T. ) ;
#82494 = AXIS2_PLACEMENT_3D ( 'NONE', #51868, #31578, #102254 ) ;
#82495 = CARTESIAN_POINT ( 'NONE',  ( -11.25000000000000000, 12.50000000000000000, 7.253104124594885960 ) ) ;
#82496 = VECTOR ( 'NONE', #88697, 1000.000000000000000 ) ;
#82498 = ADVANCED_FACE ( 'NONE', ( #28098 ), #21967, .T. ) ;
#82497 = DIRECTION ( 'NONE',  ( 0.000000000000000000, 1.000000000000000000, 0.000000000000000000 ) ) ;
#82499 = CARTESIAN_POINT ( 'NONE',  ( 12.49999999999993960, 12.50000000000000000, 4.395220292106234439 ) ) ;
#82500 = FACE_OUTER_BOUND ( 'NONE', #31771, .T. ) ;
#82501 = CARTESIAN_POINT ( 'NONE',  ( 185.0312500006828031, 9.429780353434619030E-16, -7.700000000000000178 ) ) ;
#82502 = DIRECTION ( 'NONE',  ( 0.000000000000000000, 0.000000000000000000, -1.000000000000000000 ) ) ;
#82503 = CARTESIAN_POINT ( 'NONE',  ( -1.250000000000037970, 12.50000000000000000, 2.857883832488649301 ) ) ;
#82504 = DIRECTION ( 'NONE',  ( 0.000000000000000000, 0.000000000000000000, -1.000000000000000000 ) ) ;
#82505 = EDGE_CURVE ( 'NONE', #129541, #43692, #51201, .T. ) ;
#82506 = EDGE_CURVE ( 'NONE', #89650, #57903, #118082, .T. ) ;
#82507 = DIRECTION ( 'NONE',  ( 0.000000000000000000, -0.000000000000000000, 1.000000000000000000 ) ) ;
#82508 = ORIENTED_EDGE ( 'NONE', *, *, #115525, .F. ) ;
#82509 = EDGE_CURVE ( 'NONE', #16531, #121848, #24005, .T. ) ;
#82510 = CIRCLE ( 'NONE', #115941, 0.06509327318403745899 ) ;
#82511 = FACE_OUTER_BOUND ( 'NONE', #96834, .T. ) ;
#82512 = CIRCLE ( 'NONE', #59548, 0.09999999999999982514 ) ;
#82513 = AXIS2_PLACEMENT_3D ( 'NONE', #114329, #56044, #64581 ) ;
#82514 = ORIENTED_EDGE ( 'NONE', *, *, #124578, .F. ) ;
#82515 = EDGE_LOOP ( 'NONE', ( #107581, #8749 ) ) ;
#82516 = ADVANCED_FACE ( 'NONE', ( #36650 ), #76553, .T. ) ;
#82517 = DIRECTION ( 'NONE',  ( 0.000000000000000000, 0.000000000000000000, -1.000000000000000000 ) ) ;
#82518 = CARTESIAN_POINT ( 'NONE',  ( 5.399999999999932854, 2.500000000000000000, 5.122947341949749323 ) ) ;
#82519 = DIRECTION ( 'NONE',  ( -0.000000000000000000, 1.000000000000000000, -0.000000000000000000 ) ) ;
#82520 = AXIS2_PLACEMENT_3D ( 'NONE', #49024, #88932, #128884 ) ;
#82521 = CARTESIAN_POINT ( 'NONE',  ( 0.6499999999999566125, 2.500000000000000000, -6.841600689897077814 ) ) ;
#82522 = CIRCLE ( 'NONE', #11679, 0.09999999999999982514 ) ;
#82523 = DIRECTION ( 'NONE',  ( 0.000000000000000000, 0.000000000000000000, -1.000000000000000000 ) ) ;
#82524 = CARTESIAN_POINT ( 'NONE',  ( -12.69999999999999218, 12.50000000000000000, -0.3464101615137741286 ) ) ;
#82525 = CARTESIAN_POINT ( 'NONE',  ( -17.50000000000000000, -1.500000000000000000, 1.734723475976807094E-15 ) ) ;
#82526 = ORIENTED_EDGE ( 'NONE', *, *, #111009, .F. ) ;
#82527 = CIRCLE ( 'NONE', #26081, 0.06509327318403745899 ) ;
#82529 = ORIENTED_EDGE ( 'NONE', *, *, #75159, .T. ) ;
#82528 = CONICAL_SURFACE ( 'NONE', #88775, 0.1000000000000000472, 0.003490658503988666988 ) ;
#82530 = AXIS2_PLACEMENT_3D ( 'NONE', #6415, #44445, #43825 ) ;
#82531 = VERTEX_POINT ( 'NONE', #79148 ) ;
#82532 = VERTEX_POINT ( 'NONE', #60783 ) ;
#82533 = CIRCLE ( 'NONE', #26095, 0.06509327318403745899 ) ;
#82534 = VERTEX_POINT ( 'NONE', #553 ) ;
#82535 = LINE ( 'NONE', #40028, #85805 ) ;
#82536 = CARTESIAN_POINT ( 'NONE',  ( -10.60000000000000142, 12.50000000000000000, -0.3464101615137782364 ) ) ;
#82537 = DIRECTION ( 'NONE',  ( 0.000000000000000000, 0.000000000000000000, 1.000000000000000000 ) ) ;
#82538 = CARTESIAN_POINT ( 'NONE',  ( -5.800000000000018474, 12.50000000000000000, -0.06509327318403970719 ) ) ;
#82539 = DIRECTION ( 'NONE',  ( 0.000000000000000000, 0.000000000000000000, 1.000000000000000000 ) ) ;
#82540 = VERTEX_POINT ( 'NONE', #49047 ) ;
#82541 = CARTESIAN_POINT ( 'NONE',  ( -0.6500000000000398792, 2.500000000000000000, -2.511473670974877948 ) ) ;
#82542 = DIRECTION ( 'NONE',  ( -0.000000000000000000, 1.000000000000000000, -0.000000000000000000 ) ) ;
#82543 = DIRECTION ( 'NONE',  ( 0.000000000000000000, 1.000000000000000000, 0.000000000000000000 ) ) ;
#82544 = AXIS2_PLACEMENT_3D ( 'NONE', #15194, #66964, #35604 ) ;
#82545 = CARTESIAN_POINT ( 'NONE',  ( 187.1145833340161175, 6.668395609140177704, -3.849999999999998312 ) ) ;
#82546 = ORIENTED_EDGE ( 'NONE', *, *, #101552, .T. ) ;
#82547 = ORIENTED_EDGE ( 'NONE', *, *, #36538, .T. ) ;
#82548 = VERTEX_POINT ( 'NONE', #18904 ) ;
#82549 = EDGE_CURVE ( 'NONE', #71852, #115126, #61665, .T. ) ;
#82550 = DIRECTION ( 'NONE',  ( 0.000000000000000000, 1.000000000000000000, 0.000000000000000000 ) ) ;
#82551 = EDGE_CURVE ( 'NONE', #27445, #22099, #100065, .T. ) ;
#82552 = EDGE_CURVE ( 'NONE', #43625, #94349, #28208, .T. ) ;
#82553 = EDGE_LOOP ( 'NONE', ( #109423, #18258 ) ) ;
#82554 = AXIS2_PLACEMENT_3D ( 'NONE', #93889, #34341, #15297 ) ;
#82555 = EDGE_CURVE ( 'NONE', #8533, #79987, #9325, .T. ) ;
#82556 = DIRECTION ( 'NONE',  ( -0.000000000000000000, 1.000000000000000000, -0.000000000000000000 ) ) ;
#82557 = CARTESIAN_POINT ( 'NONE',  ( 3.349999999999945466, 2.500000000000000000, -2.065063509461102065 ) ) ;
#82558 = CIRCLE ( 'NONE', #44994, 0.06509327318403745899 ) ;
#82559 = EDGE_CURVE ( 'NONE', #94388, #129360, #105573, .T. ) ;
#82560 = EDGE_LOOP ( 'NONE', ( #71365, #73243 ) ) ;
#82561 = DIRECTION ( 'NONE',  ( 0.000000000000000000, 0.000000000000000000, 1.000000000000000000 ) ) ;
#82562 = DIRECTION ( 'NONE',  ( 0.000000000000000000, 0.000000000000000000, -1.000000000000000000 ) ) ;
#82563 = CARTESIAN_POINT ( 'NONE',  ( 184.5000000000000284, -7.608433918590866263, 0.5575073813830642155 ) ) ;
#82564 = DIRECTION ( 'NONE',  ( 0.000000000000000000, 0.000000000000000000, 1.000000000000000000 ) ) ;
#82565 = EDGE_CURVE ( 'NONE', #51534, #110814, #49063, .T. ) ;
#82566 = AXIS2_PLACEMENT_3D ( 'NONE', #86569, #27023, #58426 ) ;
#82567 = EDGE_CURVE ( 'NONE', #24704, #38510, #78395, .T. ) ;
#82568 = CARTESIAN_POINT ( 'NONE',  ( -11.69999999999999929, 12.50000000000000000, 0.06509327318403916596 ) ) ;
#82569 = CIRCLE ( 'NONE', #22026, 0.1000000000000002554 ) ;
#82570 = EDGE_LOOP ( 'NONE', ( #90977, #13003, #83943, #118338 ) ) ;
#82571 = ORIENTED_EDGE ( 'NONE', *, *, #28903, .T. ) ;
#82572 = LINE ( 'NONE', #62916, #91932 ) ;
#82573 = DIRECTION ( 'NONE',  ( 0.000000000000000000, 0.000000000000000000, 1.000000000000000000 ) ) ;
#82574 = ADVANCED_FACE ( 'NONE', ( #90218 ), #111838, .T. ) ;
#82575 = CARTESIAN_POINT ( 'NONE',  ( 1.849999999999950573, 12.50000000000000000, 2.446380397790835826 ) ) ;
#82576 = DIRECTION ( 'NONE',  ( 0.000000000000000000, 1.000000000000000000, 0.000000000000000000 ) ) ;
#82577 = VERTEX_POINT ( 'NONE', #111143 ) ;
#82578 = AXIS2_PLACEMENT_3D ( 'NONE', #12381, #71971, #41229 ) ;
#82579 = CIRCLE ( 'NONE', #11459, 0.1000000000000000472 ) ;
#82580 = ORIENTED_EDGE ( 'NONE', *, *, #49089, .T. ) ;
#82581 = CARTESIAN_POINT ( 'NONE',  ( -3.950000000000026379, 2.500000000000000000, -1.918653347947326004 ) ) ;
#82582 = DIRECTION ( 'NONE',  ( 0.000000000000000000, 0.000000000000000000, 1.000000000000000000 ) ) ;
#82583 = DIRECTION ( 'NONE',  ( 0.000000000000000000, 1.000000000000000000, 0.000000000000000000 ) ) ;
#82584 = LINE ( 'NONE', #13160, #92735 ) ;
#82585 = ORIENTED_EDGE ( 'NONE', *, *, #109271, .F. ) ;
#82586 = CARTESIAN_POINT ( 'NONE',  ( 9.549999999999918998, 12.50000000000000000, -6.560283801567339701 ) ) ;
#82587 = CARTESIAN_POINT ( 'NONE',  ( 11.44999999999990692, 12.50000000000000000, 1.818653347947321475 ) ) ;
#82588 = ORIENTED_EDGE ( 'NONE', *, *, #93067, .F. ) ;
#82589 = LINE ( 'NONE', #70817, #9308 ) ;
#82590 = CIRCLE ( 'NONE', #105665, 2.000000000000000000 ) ;
#82591 = ORIENTED_EDGE ( 'NONE', *, *, #22829, .T. ) ;
#82592 = CARTESIAN_POINT ( 'NONE',  ( 6.649999999999930189, 12.50000000000000000, -2.792790559304616504 ) ) ;
#82593 = CIRCLE ( 'NONE', #36636, 0.06509327318403745899 ) ;
#82594 = EDGE_LOOP ( 'NONE', ( #1147, #58501 ) ) ;
#82595 = DIRECTION ( 'NONE',  ( 0.000000000000000000, 0.000000000000000000, -1.000000000000000000 ) ) ;
#82596 = CARTESIAN_POINT ( 'NONE',  ( -6.450000000000019718, 2.500000000000000000, -1.718653347947326049 ) ) ;
#82597 = CIRCLE ( 'NONE', #55400, 0.1000000000000002554 ) ;
#82598 = ORIENTED_EDGE ( 'NONE', *, *, #342, .T. ) ;
#82599 = ORIENTED_EDGE ( 'NONE', *, *, #77747, .F. ) ;
#82600 = CARTESIAN_POINT ( 'NONE',  ( 187.2135416670080588, 4.367472073101518859, -7.564683531249999149 ) ) ;
#82601 = FACE_OUTER_BOUND ( 'NONE', #45373, .T. ) ;
#82602 = CARTESIAN_POINT ( 'NONE',  ( 186.5885416670080872, -6.551208109652273848, -3.782341765625003571 ) ) ;
#82603 = CARTESIAN_POINT ( 'NONE',  ( 185.0260416670080588, -6.551208109652273848, -3.782341765625003571 ) ) ;
#82604 = AXIS2_PLACEMENT_3D ( 'NONE', #25326, #5685, #16780 ) ;
#82605 = EDGE_CURVE ( 'NONE', #117649, #115225, #95110, .T. ) ;
#82606 = CIRCLE ( 'NONE', #92980, 0.1000000000000002554 ) ;
#82607 = DIRECTION ( 'NONE',  ( -4.274815082592931898E-19, -0.9999939076577903929, -0.003490651415223739937 ) ) ;
#82608 = LINE ( 'NONE', #41401, #17964 ) ;
#82609 = DIRECTION ( 'NONE',  ( 0.000000000000000000, 1.000000000000000000, 0.000000000000000000 ) ) ;
#82610 = AXIS2_PLACEMENT_3D ( 'NONE', #33293, #73198, #113113 ) ;
#82611 = LINE ( 'NONE', #30299, #68230 ) ;
#82612 = PLANE ( 'NONE',  #14899 ) ;
#82613 = CIRCLE ( 'NONE', #74295, 0.06509327318403745899 ) ;
#82614 = AXIS2_PLACEMENT_3D ( 'NONE', #86942, #110922, #77755 ) ;
#82615 = EDGE_LOOP ( 'NONE', ( #13055, #95972 ) ) ;
#82616 = ORIENTED_EDGE ( 'NONE', *, *, #2690, .T. ) ;
#82617 = CARTESIAN_POINT ( 'NONE',  ( -2.050000000000033129, 2.500000000000000000, 6.495190528383297135 ) ) ;
#82618 = VERTEX_POINT ( 'NONE', #21497 ) ;
#82619 = DIRECTION ( 'NONE',  ( -0.000000000000000000, -1.000000000000000000, -0.000000000000000000 ) ) ;
#82620 = PLANE ( 'NONE',  #7387 ) ;
#82621 = CONICAL_SURFACE ( 'NONE', #101396, 0.1000000000000000472, 0.003490658503988666988 ) ;
#82622 = DIRECTION ( 'NONE',  ( -0.000000000000000000, 1.000000000000000000, -0.000000000000000000 ) ) ;
#82624 = ORIENTED_EDGE ( 'NONE', *, *, #16590, .F. ) ;
#82623 = ORIENTED_EDGE ( 'NONE', *, *, #27842, .F. ) ;
#82625 = FACE_BOUND ( 'NONE', #49175, .T. ) ;
#82626 = EDGE_LOOP ( 'NONE', ( #65733, #40318, #59220, #56847 ) ) ;
#82627 = DIRECTION ( 'NONE',  ( 0.000000000000000000, 1.000000000000000000, 0.000000000000000000 ) ) ;
#82628 = CARTESIAN_POINT ( 'NONE',  ( 7.499999999999961808, 2.500000000000000000, 4.230127018922196669 ) ) ;
#82629 = DIRECTION ( 'NONE',  ( 0.000000000000000000, 0.000000000000000000, 1.000000000000000000 ) ) ;
#82630 = CARTESIAN_POINT ( 'NONE',  ( 12.49999999999993960, 2.500000000000000000, 4.330127018922196314 ) ) ;
#82631 = DIRECTION ( 'NONE',  ( 0.000000000000000000, 1.000000000000000000, 0.000000000000000000 ) ) ;
#82632 = PLANE ( 'NONE',  #6845 ) ;
#82633 = DIRECTION ( 'NONE',  ( -0.000000000000000000, 1.000000000000000000, -0.000000000000000000 ) ) ;
#82634 = DIRECTION ( 'NONE',  ( -1.000000000000000000, 0.000000000000000000, 0.000000000000000000 ) ) ;
#82635 = DIRECTION ( 'NONE',  ( 0.000000000000000000, 0.000000000000000000, 1.000000000000000000 ) ) ;
#82636 = FACE_OUTER_BOUND ( 'NONE', #101002, .T. ) ;
#82637 = CIRCLE ( 'NONE', #36581, 0.06509327318403745899 ) ;
#82638 = DIRECTION ( 'NONE',  ( 0.000000000000000000, 0.000000000000000000, 1.000000000000000000 ) ) ;
#82639 = ORIENTED_EDGE ( 'NONE', *, *, #7684, .T. ) ;
#82640 = ORIENTED_EDGE ( 'NONE', *, *, #8362, .T. ) ;
#82641 = EDGE_LOOP ( 'NONE', ( #1879, #120035 ) ) ;
#82642 = CARTESIAN_POINT ( 'NONE',  ( -1.250000000000037970, 2.500000000000000000, 7.088010851410848190 ) ) ;
#82643 = ORIENTED_EDGE ( 'NONE', *, *, #110678, .F. ) ;
#82644 = DIRECTION ( 'NONE',  ( -0.000000000000000000, 1.000000000000000000, -0.000000000000000000 ) ) ;
#82646 = EDGE_LOOP ( 'NONE', ( #106150, #70818, #74282, #13228 ) ) ;
#82645 = EDGE_LOOP ( 'NONE', ( #15064, #51426 ) ) ;
#82647 = CONICAL_SURFACE ( 'NONE', #111880, 0.1000000000000000472, 0.003490658503988666988 ) ;
#82648 = ORIENTED_EDGE ( 'NONE', *, *, #108769, .T. ) ;
#82649 = FACE_OUTER_BOUND ( 'NONE', #96330, .T. ) ;
#82650 = CONICAL_SURFACE ( 'NONE', #124506, 0.1000000000000002554, 0.003490658503988666988 ) ;
#82651 = VECTOR ( 'NONE', #69711, 1000.000000000000000 ) ;
#82652 = ADVANCED_FACE ( 'NONE', ( #100687 ), #101358, .T. ) ;
#82653 = DIRECTION ( 'NONE',  ( 0.000000000000000000, 1.000000000000000000, 0.000000000000000000 ) ) ;
#82654 = DIRECTION ( 'NONE',  ( -0.000000000000000000, 1.000000000000000000, -0.000000000000000000 ) ) ;
#82655 = DIRECTION ( 'NONE',  ( 0.000000000000000000, 1.000000000000000000, 0.000000000000000000 ) ) ;
#82656 = DIRECTION ( 'NONE',  ( 0.000000000000000000, 0.000000000000000000, -1.000000000000000000 ) ) ;
#82657 = ADVANCED_FACE ( 'NONE', ( #50977 ), #57454, .T. ) ;
#82658 = ORIENTED_EDGE ( 'NONE', *, *, #49435, .F. ) ;
#82659 = EDGE_CURVE ( 'NONE', #103176, #69132, #90880, .T. ) ;
#82660 = CARTESIAN_POINT ( 'NONE',  ( -10.60000000000000142, 12.50000000000000000, 4.048810130592458201 ) ) ;
#82661 = ORIENTED_EDGE ( 'NONE', *, *, #98924, .F. ) ;
#82662 = CIRCLE ( 'NONE', #93125, 0.1000000000000002554 ) ;
#82663 = VERTEX_POINT ( 'NONE', #109216 ) ;
#82664 = ORIENTED_EDGE ( 'NONE', *, *, #119469, .T. ) ;
#82665 = VECTOR ( 'NONE', #25949, 1000.000000000000000 ) ;
#82666 = ADVANCED_FACE ( 'NONE', ( #30695 ), #13522, .T. ) ;
#82668 = ADVANCED_FACE ( 'NONE', ( #120990 ), #126409, .T. ) ;
#82667 = CARTESIAN_POINT ( 'NONE',  ( 185.1145833340161175, 6.668395609140177704, -3.849999999999998312 ) ) ;
#82670 = VERTEX_POINT ( 'NONE', #79774 ) ;
#82669 = EDGE_CURVE ( 'NONE', #110342, #37153, #49691, .T. ) ;
#82671 = ORIENTED_EDGE ( 'NONE', *, *, #75973, .T. ) ;
#82672 = ADVANCED_FACE ( 'NONE', ( #30043 ), #61766, .T. ) ;
#82674 = ORIENTED_EDGE ( 'NONE', *, *, #57810, .T. ) ;
#82673 = EDGE_CURVE ( 'NONE', #98422, #29970, #30278, .T. ) ;
#82675 =( LENGTH_UNIT ( ) NAMED_UNIT ( * ) SI_UNIT ( .MILLI., .METRE. ) );
#82677 = AXIS2_PLACEMENT_3D ( 'NONE', #40253, #80171, #58607 ) ;
#82676 = DIRECTION ( 'NONE',  ( 0.000000000000000000, 0.000000000000000000, -1.000000000000000000 ) ) ;
#82678 = DIRECTION ( 'NONE',  ( 0.000000000000000000, -0.000000000000000000, 1.000000000000000000 ) ) ;
#82679 = VECTOR ( 'NONE', #53166, 1000.000000000000000 ) ;
#82680 = CARTESIAN_POINT ( 'NONE',  ( -6.250000000000021316, 2.500000000000000000, -1.572243186433550211 ) ) ;
#82681 = CARTESIAN_POINT ( 'NONE',  ( -14.59999999999998366, 2.500000000000000000, -0.6928203230275520319 ) ) ;
#82682 = CARTESIAN_POINT ( 'NONE',  ( -13.14999999999999147, 2.500000000000000000, -1.718653347947323828 ) ) ;
#82683 = ADVANCED_FACE ( 'NONE', ( #3157 ), #9520, .T. ) ;
#82684 = DIRECTION ( 'NONE',  ( 0.000000000000000000, 0.000000000000000000, -1.000000000000000000 ) ) ;
#82685 = ORIENTED_EDGE ( 'NONE', *, *, #94049, .F. ) ;
#82686 = DIRECTION ( 'NONE',  ( -0.000000000000000000, -1.000000000000000000, -0.000000000000000000 ) ) ;
#82687 = ORIENTED_EDGE ( 'NONE', *, *, #33029, .T. ) ;
#82688 = DIRECTION ( 'NONE',  ( 0.000000000000000000, 0.000000000000000000, 1.000000000000000000 ) ) ;
#82689 = AXIS2_PLACEMENT_3D ( 'NONE', #31297, #70548, #60114 ) ;
#82690 = VERTEX_POINT ( 'NONE', #4399 ) ;
#82691 = FACE_OUTER_BOUND ( 'NONE', #8679, .T. ) ;
#82692 = CIRCLE ( 'NONE', #120333, 0.09999999999999999167 ) ;
#82693 = EDGE_LOOP ( 'NONE', ( #77427, #124832, #32426, #23047 ) ) ;
#82694 = CARTESIAN_POINT ( 'NONE',  ( -1.900000000000034994, 2.500000000000000000, -0.2464101615137783419 ) ) ;
#82695 = AXIS2_PLACEMENT_3D ( 'NONE', #84047, #24497, #113513 ) ;
#82697 = CARTESIAN_POINT ( 'NONE',  ( -12.69999999999999218, 2.500000000000000000, -4.676537180435975216 ) ) ;
#82696 = AXIS2_PLACEMENT_3D ( 'NONE', #38930, #69642, #78844 ) ;
#82698 = ORIENTED_EDGE ( 'NONE', *, *, #5193, .F. ) ;
#82699 = EDGE_LOOP ( 'NONE', ( #48563, #2151 ) ) ;
#82700 =( BOUNDED_CURVE ( )  B_SPLINE_CURVE ( 2, ( #102418, #91950, #12722, #82792, #112882, #42214, #123972 ),
 .UNSPECIFIED., .F., .F. ) 
 B_SPLINE_CURVE_WITH_KNOTS ( ( 3, 2, 2, 3 ),
 ( 0.5714285714285719520, 0.5952380952380957879, 0.6190476190476195129, 0.6428571428571433488 ),
 .UNSPECIFIED. ) 
 CURVE ( )  GEOMETRIC_REPRESENTATION_ITEM ( )  RATIONAL_B_SPLINE_CURVE ( ( 0.9999999999999968914, 0.8660254037844418162, 1.000000000000000000, 0.8660254037844387076, 1.000000000000000000, 0.8660254037844361541, 1.000000000000002442 ) ) 
 REPRESENTATION_ITEM ( '' )  );
#82701 = DIRECTION ( 'NONE',  ( -0.000000000000000000, 1.000000000000000000, -0.000000000000000000 ) ) ;
#82702 = CARTESIAN_POINT ( 'NONE',  ( 0.8499999999999545697, 2.500000000000000000, -1.472243186433550122 ) ) ;
#82703 = DIRECTION ( 'NONE',  ( 0.000000000000000000, 0.000000000000000000, 1.000000000000000000 ) ) ;
#82704 = CARTESIAN_POINT ( 'NONE',  ( -11.64999999999999858, 12.50000000000000000, -1.472243186433546125 ) ) ;
#82705 = AXIS2_PLACEMENT_3D ( 'NONE', #37441, #46595, #36144 ) ;
#82706 = CARTESIAN_POINT ( 'NONE',  ( 7.699999999999923794, 2.500000000000000000, -4.083716857408426826 ) ) ;
#82707 = ORIENTED_EDGE ( 'NONE', *, *, #84750, .T. ) ;
#82708 = CARTESIAN_POINT ( 'NONE',  ( 2.500000000000002220, -2.500000000000000000, 9.261799387799150907 ) ) ;
#82709 = VECTOR ( 'NONE', #54666, 1000.000000000000000 ) ;
#82710 = EDGE_CURVE ( 'NONE', #3855, #3469, #43102, .T. ) ;
#82711 = EDGE_CURVE ( 'NONE', #4247, #40133, #15757, .T. ) ;
#82712 = ORIENTED_EDGE ( 'NONE', *, *, #39200, .F. ) ;
#82713 = AXIS2_PLACEMENT_3D ( 'NONE', #120037, #91217, #70293 ) ;
#82714 = DIRECTION ( 'NONE',  ( 0.000000000000000000, 0.000000000000000000, 1.000000000000000000 ) ) ;
#82716 = AXIS2_PLACEMENT_3D ( 'NONE', #95806, #76176, #125897 ) ;
#82715 = CARTESIAN_POINT ( 'NONE',  ( 6.449999999999931788, 2.500000000000000000, -2.511473670974877948 ) ) ;
#82717 = ADVANCED_FACE ( 'NONE', ( #43743 ), #65850, .T. ) ;
#82718 = AXIS2_PLACEMENT_3D ( 'NONE', #98397, #57858, #17909 ) ;
#82719 = CARTESIAN_POINT ( 'NONE',  ( 187.1666666666666856, -6.668395609140176816, -3.850000000000003642 ) ) ;
#82720 = CARTESIAN_POINT ( 'NONE',  ( 0.3999999999999628852, 12.50000000000000000, -0.6928203230275520319 ) ) ;
#82721 = DIRECTION ( 'NONE',  ( 0.000000000000000000, 0.000000000000000000, 1.000000000000000000 ) ) ;
#82722 = ADVANCED_FACE ( 'NONE', ( #112469 ), #40846, .T. ) ;
#82723 = CARTESIAN_POINT ( 'NONE',  ( 1.849999999999950129, 2.500000000000000000, -6.941600689897078347 ) ) ;
#82724 = FACE_OUTER_BOUND ( 'NONE', #23809, .T. ) ;
#82725 = VERTEX_POINT ( 'NONE', #102624 ) ;
#82726 = EDGE_CURVE ( 'NONE', #20272, #72203, #28301, .T. ) ;
#82727 = EDGE_CURVE ( 'NONE', #84568, #37944, #5293, .T. ) ;
#82728 = DIRECTION ( 'NONE',  ( 0.000000000000000000, 0.000000000000000000, 1.000000000000000000 ) ) ;
#82729 = EDGE_CURVE ( 'NONE', #74213, #48575, #95202, .T. ) ;
#82730 = DIRECTION ( 'NONE',  ( 0.000000000000000000, 0.000000000000000000, 1.000000000000000000 ) ) ;
#82731 = PLANE ( 'NONE',  #28720 ) ;
#82732 = ORIENTED_EDGE ( 'NONE', *, *, #99502, .T. ) ;
#82733 = AXIS2_PLACEMENT_3D ( 'NONE', #25598, #16407, #56990 ) ;
#82734 = EDGE_CURVE ( 'NONE', #6628, #103260, #51307, .T. ) ;
#82735 = CARTESIAN_POINT ( 'NONE',  ( -11.89999999999999680, 2.500000000000000000, 0.3464101615137776813 ) ) ;
#82736 = VERTEX_POINT ( 'NONE', #33275 ) ;
#82737 = ORIENTED_EDGE ( 'NONE', *, *, #116901, .F. ) ;
#82738 = LINE ( 'NONE', #113462, #28034 ) ;
#82739 = AXIS2_PLACEMENT_3D ( 'NONE', #10480, #39961, #32734 ) ;
#82740 = ORIENTED_EDGE ( 'NONE', *, *, #23212, .T. ) ;
#82741 = CARTESIAN_POINT ( 'NONE',  ( -3.550000000000028688, 2.500000000000000000, 6.741600689897071952 ) ) ;
#82742 = DIRECTION ( 'NONE',  ( 0.000000000000000000, 1.000000000000000000, 0.000000000000000000 ) ) ;
#82743 = LINE ( 'NONE', #124586, #119598 ) ;
#82744 = AXIS2_PLACEMENT_3D ( 'NONE', #36266, #26440, #106280 ) ;
#82745 = CIRCLE ( 'NONE', #122448, 0.1000000000000000472 ) ;
#82746 = ORIENTED_EDGE ( 'NONE', *, *, #61118, .F. ) ;
#82747 = DIRECTION ( 'NONE',  ( 0.000000000000000000, 0.000000000000000000, 1.000000000000000000 ) ) ;
#82748 = CIRCLE ( 'NONE', #55545, 1.000000000000000888 ) ;
#82749 = DIRECTION ( 'NONE',  ( -4.274815082592931898E-19, -0.9999939076577903929, -0.003490651415223739937 ) ) ;
#82750 = EDGE_CURVE ( 'NONE', #66161, #92620, #7350, .T. ) ;
#82751 = ORIENTED_EDGE ( 'NONE', *, *, #52568, .T. ) ;
#82752 = AXIS2_PLACEMENT_3D ( 'NONE', #111874, #83065, #52957 ) ;
#82753 = ORIENTED_EDGE ( 'NONE', *, *, #69128, .F. ) ;
#82755 = AXIS2_PLACEMENT_3D ( 'NONE', #18041, #107724, #87427 ) ;
#82754 = AXIS2_PLACEMENT_3D ( 'NONE', #8556, #48504, #11139 ) ;
#82756 = VERTEX_POINT ( 'NONE', #13595 ) ;
#82757 = FACE_OUTER_BOUND ( 'NONE', #119002, .T. ) ;
#82758 = CARTESIAN_POINT ( 'NONE',  ( -7.900000000000014566, 2.500000000000000000, -4.230127018922201998 ) ) ;
#82759 = DIRECTION ( 'NONE',  ( -4.274815082592931898E-19, -0.9999939076577903929, -0.003490651415223739937 ) ) ;
#82760 = FACE_BOUND ( 'NONE', #15928, .T. ) ;
#82761 = VERTEX_POINT ( 'NONE', #52896 ) ;
#82762 = CARTESIAN_POINT ( 'NONE',  ( 5.799999999999931433, 12.50000000000000000, 4.330127018922196314 ) ) ;
#82763 = DIRECTION ( 'NONE',  ( 0.000000000000000000, 0.000000000000000000, -1.000000000000000000 ) ) ;
#82764 = ORIENTED_EDGE ( 'NONE', *, *, #14223, .F. ) ;
#82765 = CARTESIAN_POINT ( 'NONE',  ( -11.89999999999999503, 12.50000000000000000, 4.741630453620009789 ) ) ;
#82767 = FACE_OUTER_BOUND ( 'NONE', #105497, .T. ) ;
#82766 = CIRCLE ( 'NONE', #97327, 0.09999999999999982514 ) ;
#82768 = CONICAL_SURFACE ( 'NONE', #78564, 0.1000000000000000472, 0.003490658503988666988 ) ;
#82769 = EDGE_CURVE ( 'NONE', #11681, #55449, #123547, .T. ) ;
#82770 = FACE_OUTER_BOUND ( 'NONE', #76271, .T. ) ;
#82771 = DIRECTION ( 'NONE',  ( 0.000000000000000000, 1.000000000000000000, 0.000000000000000000 ) ) ;
#82772 = CARTESIAN_POINT ( 'NONE',  ( -4.800000000000026468, 2.500000000000000000, -4.676537180435978769 ) ) ;
#82773 = DIRECTION ( 'NONE',  ( 0.000000000000000000, 0.000000000000000000, -1.000000000000000000 ) ) ;
#82774 = DIRECTION ( 'NONE',  ( 0.000000000000000000, 1.000000000000000000, 0.000000000000000000 ) ) ;
#82775 = ORIENTED_EDGE ( 'NONE', *, *, #117868, .T. ) ;
#82776 = VERTEX_POINT ( 'NONE', #71902 ) ;
#82777 = ORIENTED_EDGE ( 'NONE', *, *, #21755, .F. ) ;
#82778 = ORIENTED_EDGE ( 'NONE', *, *, #84262, .F. ) ;
#82779 = DIRECTION ( 'NONE',  ( 0.000000000000000000, -0.000000000000000000, 1.000000000000000000 ) ) ;
#82780 = DIRECTION ( 'NONE',  ( -0.000000000000000000, -1.000000000000000000, -0.000000000000000000 ) ) ;
#82781 = DIRECTION ( 'NONE',  ( 0.000000000000000000, 0.000000000000000000, 1.000000000000000000 ) ) ;
#82782 = ORIENTED_EDGE ( 'NONE', *, *, #16692, .F. ) ;
#82783 = EDGE_CURVE ( 'NONE', #123701, #39867, #103290, .T. ) ;
#82784 = FACE_BOUND ( 'NONE', #12683, .T. ) ;
#82785 = DIRECTION ( 'NONE',  ( -0.000000000000000000, -1.000000000000000000, -0.000000000000000000 ) ) ;
#82786 = LINE ( 'NONE', #114792, #50045 ) ;
#82787 = DIRECTION ( 'NONE',  ( 0.000000000000000000, 1.000000000000000000, 0.000000000000000000 ) ) ;
#82788 = CIRCLE ( 'NONE', #68086, 0.1000000000000002554 ) ;
#82789 = CARTESIAN_POINT ( 'NONE',  ( 11.44999999999991047, 2.500000000000000000, -2.611473670974877592 ) ) ;
#82790 = CIRCLE ( 'NONE', #70258, 0.06509327318403745899 ) ;
#82791 = CARTESIAN_POINT ( 'NONE',  ( 6.249999999999934275, 12.50000000000000000, -7.188010851410854052 ) ) ;
#82792 = CARTESIAN_POINT ( 'NONE',  ( 185.3750000000000000, 8.891194145520236347, 5.444286225454521982E-16 ) ) ;
#82793 = LINE ( 'NONE', #2935, #35066 ) ;
#82794 = PLANE ( 'NONE',  #128632 ) ;
#82795 = DIRECTION ( 'NONE',  ( 0.000000000000000000, -0.000000000000000000, 1.000000000000000000 ) ) ;
#82796 = ORIENTED_EDGE ( 'NONE', *, *, #22255, .T. ) ;
#82797 = VERTEX_POINT ( 'NONE', #111822 ) ;
#82798 = VERTEX_POINT ( 'NONE', #62082 ) ;
#82799 = EDGE_LOOP ( 'NONE', ( #39739, #31756, #35167, #42911 ) ) ;
#82800 = ORIENTED_EDGE ( 'NONE', *, *, #67736, .F. ) ;
#82801 = ORIENTED_EDGE ( 'NONE', *, *, #71579, .T. ) ;
#82802 = CIRCLE ( 'NONE', #86884, 0.1000000000000002554 ) ;
#82803 = CARTESIAN_POINT ( 'NONE',  ( 5.849999999999934808, 2.500000000000000000, -5.802370205355749988 ) ) ;
#82804 = VERTEX_POINT ( 'NONE', #12315 ) ;
#82805 = ORIENTED_EDGE ( 'NONE', *, *, #79711, .T. ) ;
#82806 = VECTOR ( 'NONE', #106816, 1000.000000000000000 ) ;
#82808 = ADVANCED_FACE ( 'NONE', ( #59288 ), #47095, .T. ) ;
#82807 = AXIS2_PLACEMENT_3D ( 'NONE', #49, #10506, #11155 ) ;
#82809 = PLANE ( 'NONE',  #20387 ) ;
#82810 = PLANE ( 'NONE',  #95980 ) ;
#82811 = CARTESIAN_POINT ( 'NONE',  ( -0.2000000000000412836, 2.500000000000000000, 4.776537180435972196 ) ) ;
#82812 = ORIENTED_EDGE ( 'NONE', *, *, #18699, .T. ) ;
#82813 = DIRECTION ( 'NONE',  ( -4.274815082592931898E-19, -0.9999939076577903929, -0.003490651415223739937 ) ) ;
#82814 = ORIENTED_EDGE ( 'NONE', *, *, #22842, .T. ) ;
#82815 = ORIENTED_EDGE ( 'NONE', *, *, #53430, .T. ) ;
#82816 = CARTESIAN_POINT ( 'NONE',  ( 10.84999999999990905, 2.500000000000000000, -7.188010851410854052 ) ) ;
#82817 = ADVANCED_FACE ( 'NONE', ( #41584 ), #105668, .T. ) ;
#82819 = EDGE_CURVE ( 'NONE', #100751, #62359, #38791, .T. ) ;
#82818 = CARTESIAN_POINT ( 'NONE',  ( 6.449999999999930012, 12.50000000000000000, 1.818653347947321475 ) ) ;
#82820 = EDGE_CURVE ( 'NONE', #47664, #56350, #19902, .T. ) ;
#82821 = EDGE_CURVE ( 'NONE', #97088, #31864, #22051, .T. ) ;
#82822 = VECTOR ( 'NONE', #102095, 1000.000000000000000 ) ;
#82823 = EDGE_LOOP ( 'NONE', ( #72155, #4952 ) ) ;
#82824 = ORIENTED_EDGE ( 'NONE', *, *, #65474, .F. ) ;
#82825 = DIRECTION ( 'NONE',  ( -0.000000000000000000, -1.000000000000000000, -0.000000000000000000 ) ) ;
#82826 = CARTESIAN_POINT ( 'NONE',  ( -6.050000000000018474, 2.500000000000000000, 2.511473670974873507 ) ) ;
#82827 = CARTESIAN_POINT ( 'NONE',  ( -1.250000000000001554, 2.500000000000000000, 2.065063509461097624 ) ) ;
#82828 = CIRCLE ( 'NONE', #26385, 0.1000000000000002554 ) ;
#82829 = FACE_OUTER_BOUND ( 'NONE', #7120, .T. ) ;
#82830 = DIRECTION ( 'NONE',  ( 0.000000000000000000, 1.000000000000000000, 0.000000000000000000 ) ) ;
#82831 = AXIS2_PLACEMENT_3D ( 'NONE', #68604, #128854, #8390 ) ;
#82832 = EDGE_CURVE ( 'NONE', #93338, #34594, #82593, .T. ) ;
#82833 = CIRCLE ( 'NONE', #26393, 0.06509327318403745899 ) ;
#82834 = EDGE_LOOP ( 'NONE', ( #46633, #68761 ) ) ;
#82836 = VECTOR ( 'NONE', #80017, 1000.000000000000000 ) ;
#82835 = DIRECTION ( 'NONE',  ( 0.000000000000000000, 1.000000000000000000, 0.000000000000000000 ) ) ;
#82837 = EDGE_CURVE ( 'NONE', #59007, #56480, #68000, .T. ) ;
#82838 = EDGE_CURVE ( 'NONE', #75963, #47693, #113975, .T. ) ;
#82839 = ORIENTED_EDGE ( 'NONE', *, *, #91738, .T. ) ;
#82840 = VECTOR ( 'NONE', #48453, 1000.000000000000000 ) ;
#82841 = FACE_OUTER_BOUND ( 'NONE', #93545, .T. ) ;
#82842 = EDGE_LOOP ( 'NONE', ( #7942, #91495 ) ) ;
#82843 = CARTESIAN_POINT ( 'NONE',  ( 9.549999999999915445, 12.50000000000000000, 6.430097255199259010 ) ) ;
#82844 = CARTESIAN_POINT ( 'NONE',  ( 9.999999999999912959, 2.500000000000000000, 3.637306695894644726 ) ) ;
#82845 = FACE_OUTER_BOUND ( 'NONE', #101878, .T. ) ;
#82846 = DIRECTION ( 'NONE',  ( -0.000000000000000000, 1.000000000000000000, -0.000000000000000000 ) ) ;
#82847 = ORIENTED_EDGE ( 'NONE', *, *, #8511, .F. ) ;
#82848 = CIRCLE ( 'NONE', #3406, 0.06509327318403745899 ) ;
#82849 = CARTESIAN_POINT ( 'NONE',  ( -8.950000000000009948, 2.500000000000000000, -6.841600689897072485 ) ) ;
#82851 = VECTOR ( 'NONE', #2106, 1000.000000000000000 ) ;
#82850 = AXIS2_PLACEMENT_3D ( 'NONE', #1180, #19527, #9716 ) ;
#82852 = DIRECTION ( 'NONE',  ( 0.000000000000000000, 0.000000000000000000, 1.000000000000000000 ) ) ;
#82853 = ORIENTED_EDGE ( 'NONE', *, *, #42794, .F. ) ;
#82854 = ORIENTED_EDGE ( 'NONE', *, *, #105446, .F. ) ;
#82855 = ORIENTED_EDGE ( 'NONE', *, *, #56174, .T. ) ;
#82856 = CARTESIAN_POINT ( 'NONE',  ( 17.50000000000000000, 0.9166666666666674068, 10.00000000000000178 ) ) ;
#82857 = LINE ( 'NONE', #63199, #13633 ) ;
#82858 = CARTESIAN_POINT ( 'NONE',  ( 185.7760416670080588, 6.551208109652274736, 3.782341765625001351 ) ) ;
#82859 = DIRECTION ( 'NONE',  ( -0.000000000000000000, 1.000000000000000000, -0.000000000000000000 ) ) ;
#82860 = CARTESIAN_POINT ( 'NONE',  ( 8.349999999999923261, 2.500000000000000000, 2.165063509461097713 ) ) ;
#82861 = DIRECTION ( 'NONE',  ( -4.274815082592931898E-19, -0.9999939076577903929, -0.003490651415223739937 ) ) ;
#82862 = DIRECTION ( 'NONE',  ( 0.000000000000000000, 0.000000000000000000, 1.000000000000000000 ) ) ;
#82863 = DIRECTION ( 'NONE',  ( 1.000000000000000000, 0.000000000000000000, 0.000000000000000000 ) ) ;
#82864 = ORIENTED_EDGE ( 'NONE', *, *, #129538, .F. ) ;
#82865 = DIRECTION ( 'NONE',  ( 0.000000000000000000, 0.000000000000000000, 1.000000000000000000 ) ) ;
#82866 = CARTESIAN_POINT ( 'NONE',  ( -3.550000000000030909, 2.500000000000000000, -6.741600689897078169 ) ) ;
#82867 = LINE ( 'NONE', #44208, #17195 ) ;
#82868 = EDGE_CURVE ( 'NONE', #105143, #87462, #26156, .T. ) ;
#82869 = CARTESIAN_POINT ( 'NONE',  ( -14.14999999999998614, 12.50000000000000000, 2.165063509461101265 ) ) ;
#82870 = EDGE_LOOP ( 'NONE', ( #120936, #113122, #44733, #122339 ) ) ;
#82871 = CARTESIAN_POINT ( 'NONE',  ( -3.550000000000027356, 2.500000000000000000, -2.611473670974877592 ) ) ;
#82872 = EDGE_CURVE ( 'NONE', #92109, #66987, #55491, .T. ) ;
#82873 = AXIS2_PLACEMENT_3D ( 'NONE', #68125, #89074, #87125 ) ;
#82874 = CIRCLE ( 'NONE', #45317, 0.1000000000000002554 ) ;
#82875 = EDGE_CURVE ( 'NONE', #103454, #26032, #59626, .T. ) ;
#82876 = CARTESIAN_POINT ( 'NONE',  ( -7.100000000000018296, 12.50000000000000000, -4.330127018922201643 ) ) ;
#82878 = VERTEX_POINT ( 'NONE', #82127 ) ;
#82877 = CARTESIAN_POINT ( 'NONE',  ( -3.350000000000028955, 12.50000000000000000, 2.165063509461097713 ) ) ;
#82879 = EDGE_LOOP ( 'NONE', ( #20237, #108631, #8097, #66616 ) ) ;
#82880 = EDGE_CURVE ( 'NONE', #126609, #75979, #11558, .T. ) ;
#82882 = AXIS2_PLACEMENT_3D ( 'NONE', #102539, #63264, #53460 ) ;
#82881 = VECTOR ( 'NONE', #79342, 1000.000000000000000 ) ;
#82883 = DIRECTION ( 'NONE',  ( -0.000000000000000000, 1.000000000000000000, -0.000000000000000000 ) ) ;
#82884 = ORIENTED_EDGE ( 'NONE', *, *, #90775, .T. ) ;
#82885 = ORIENTED_EDGE ( 'NONE', *, *, #49541, .F. ) ;
#82886 = LINE ( 'NONE', #73056, #61303 ) ;
#82887 = CARTESIAN_POINT ( 'NONE',  ( 14.34999999999989662, 12.50000000000000000, 2.511473670974873507 ) ) ;
#82888 = CARTESIAN_POINT ( 'NONE',  ( 10.19999999999991402, 12.50000000000000000, 0.4115034346978109769 ) ) ;
#82890 = AXIS2_PLACEMENT_3D ( 'NONE', #30272, #90437, #60992 ) ;
#82889 = AXIS2_PLACEMENT_3D ( 'NONE', #48565, #90394, #49866 ) ;
#82891 = CARTESIAN_POINT ( 'NONE',  ( -9.400000000000007461, 2.500000000000000000, 3.983716857408420076 ) ) ;
#82892 = ORIENTED_EDGE ( 'NONE', *, *, #70358, .T. ) ;
#82893 = CARTESIAN_POINT ( 'NONE',  ( -12.29999999999999716, 12.50000000000000000, 0.4115034346978150848 ) ) ;
#82895 = ORIENTED_EDGE ( 'NONE', *, *, #40232, .T. ) ;
#82894 = DIRECTION ( 'NONE',  ( 0.000000000000000000, 0.000000000000000000, 1.000000000000000000 ) ) ;
#82896 = CARTESIAN_POINT ( 'NONE',  ( 16.89179977596970517, 0.9177129796201533019, 5.694535519815870472 ) ) ;
#82897 = DIRECTION ( 'NONE',  ( 0.000000000000000000, -0.000000000000000000, 1.000000000000000000 ) ) ;
#82898 = VERTEX_POINT ( 'NONE', #69074 ) ;
#82899 = ORIENTED_EDGE ( 'NONE', *, *, #128329, .F. ) ;
#82900 = EDGE_LOOP ( 'NONE', ( #24556, #101912 ) ) ;
#82901 = EDGE_LOOP ( 'NONE', ( #31249, #8484, #92483, #24190 ) ) ;
#82902 = DIRECTION ( 'NONE',  ( 0.000000000000000000, 1.000000000000000000, 0.000000000000000000 ) ) ;
#82903 = CARTESIAN_POINT ( 'NONE',  ( 13.39053294345161227, 2.500000000000000444, 7.037281288959872150 ) ) ;
#82904 = FACE_OUTER_BOUND ( 'NONE', #110238, .T. ) ;
#82905 = FACE_BOUND ( 'NONE', #68220, .T. ) ;
#82906 = ORIENTED_EDGE ( 'NONE', *, *, #91682, .T. ) ;
#82907 = CIRCLE ( 'NONE', #76639, 0.06509327318403745899 ) ;
#82908 = CARTESIAN_POINT ( 'NONE',  ( 184.9479166673494603, -6.668395609140176816, -3.850000000000003642 ) ) ;
#82909 = DIRECTION ( 'NONE',  ( 0.000000000000000000, 0.000000000000000000, -1.000000000000000000 ) ) ;
#82910 = FACE_OUTER_BOUND ( 'NONE', #13575, .T. ) ;
#82911 = CIRCLE ( 'NONE', #80854, 0.06509327318403745899 ) ;
#82912 = CIRCLE ( 'NONE', #11793, 0.06509327318403745899 ) ;
#82913 = ADVANCED_FACE ( 'NONE', ( #40942 ), #128682, .T. ) ;
#82914 = FACE_OUTER_BOUND ( 'NONE', #8630, .T. ) ;
#82915 = AXIS2_PLACEMENT_3D ( 'NONE', #31919, #40463, #101945 ) ;
#82916 = DIRECTION ( 'NONE',  ( -0.000000000000000000, -1.000000000000000000, -0.000000000000000000 ) ) ;
#82917 = DIRECTION ( 'NONE',  ( 0.000000000000000000, 1.000000000000000000, 0.000000000000000000 ) ) ;
#82918 = CIRCLE ( 'NONE', #3390, 0.09999999999999982514 ) ;
#82919 = AXIS2_PLACEMENT_3D ( 'NONE', #3387, #93704, #4021 ) ;
#82920 = LINE ( 'NONE', #124767, #82974 ) ;
#82921 = ORIENTED_EDGE ( 'NONE', *, *, #121635, .F. ) ;
#82922 = EDGE_LOOP ( 'NONE', ( #18684, #113767 ) ) ;
#82923 = VERTEX_POINT ( 'NONE', #71660 ) ;
#82924 = ORIENTED_EDGE ( 'NONE', *, *, #72621, .T. ) ;
#82926 = VERTEX_POINT ( 'NONE', #110297 ) ;
#82925 = EDGE_CURVE ( 'NONE', #44661, #24778, #13614, .T. ) ;
#82927 = CARTESIAN_POINT ( 'NONE',  ( -4.800000000000024691, 2.500000000000000000, 0.3464101615137735735 ) ) ;
#82928 = PLANE ( 'NONE',  #84246 ) ;
#82929 = EDGE_LOOP ( 'NONE', ( #92122, #84971, #129386, #40865 ) ) ;
#82930 = EDGE_CURVE ( 'NONE', #70218, #85514, #108988, .T. ) ;
#82931 = FACE_BOUND ( 'NONE', #98358, .T. ) ;
#82932 = DIRECTION ( 'NONE',  ( -0.000000000000000000, -1.000000000000000000, -0.000000000000000000 ) ) ;
#82934 = CIRCLE ( 'NONE', #7689, 0.06509327318403745899 ) ;
#82933 = AXIS2_PLACEMENT_3D ( 'NONE', #25988, #105825, #16129 ) ;
#82935 = VERTEX_POINT ( 'NONE', #11449 ) ;
#82936 = DIRECTION ( 'NONE',  ( 0.000000000000000000, 1.000000000000000000, 0.000000000000000000 ) ) ;
#82937 = ADVANCED_FACE ( 'NONE', ( #2258 ), #110925, .T. ) ;
#82938 = CARTESIAN_POINT ( 'NONE',  ( 2.099999999999948574, 12.50000000000000000, 3.637306695894644726 ) ) ;
#82939 = LINE ( 'NONE', #42366, #124863 ) ;
#82940 = VERTEX_POINT ( 'NONE', #99200 ) ;
#82941 = CARTESIAN_POINT ( 'NONE',  ( -4.550000000000022915, 2.500000000000000000, -2.165063509461101710 ) ) ;
#82942 = EDGE_LOOP ( 'NONE', ( #8729, #91063 ) ) ;
#82943 = EDGE_LOOP ( 'NONE', ( #36015, #79890 ) ) ;
#82944 = VERTEX_POINT ( 'NONE', #80847 ) ;
#82945 = FACE_OUTER_BOUND ( 'NONE', #34864, .T. ) ;
#82946 = DIRECTION ( 'NONE',  ( -0.000000000000000000, 1.000000000000000000, -0.000000000000000000 ) ) ;
#82947 = DIRECTION ( 'NONE',  ( 0.000000000000000000, 0.000000000000000000, -1.000000000000000000 ) ) ;
#82948 = EDGE_LOOP ( 'NONE', ( #117011, #74332, #101741, #43785 ) ) ;
#82949 = CIRCLE ( 'NONE', #26511, 0.06509327318403745899 ) ;
#82950 = DIRECTION ( 'NONE',  ( -0.000000000000000000, 1.000000000000000000, -0.000000000000000000 ) ) ;
#82951 = CARTESIAN_POINT ( 'NONE',  ( -8.749999999999975131, 12.50000000000000000, 2.230156782645134950 ) ) ;
#82952 = ADVANCED_FACE ( 'NONE', ( #9523 ), #74275, .T. ) ;
#82953 = LINE ( 'NONE', #101304, #118399 ) ;
#82954 = LINE ( 'NONE', #1787, #3655 ) ;
#82955 = VERTEX_POINT ( 'NONE', #14011 ) ;
#82956 = CARTESIAN_POINT ( 'NONE',  ( 9.799999999999917222, 2.500000000000000000, 0.4464101615137735513 ) ) ;
#82957 = VERTEX_POINT ( 'NONE', #42880 ) ;
#82958 = PLANE ( 'NONE',  #120260 ) ;
#82959 = ADVANCED_FACE ( 'NONE', ( #84701 ), #65038, .T. ) ;
#82960 = CONICAL_SURFACE ( 'NONE', #128946, 0.09999999999999999167, 0.003490658503988666988 ) ;
#82961 = EDGE_LOOP ( 'NONE', ( #28875, #70033 ) ) ;
#82962 = EDGE_LOOP ( 'NONE', ( #111248, #106304 ) ) ;
#82963 = CARTESIAN_POINT ( 'NONE',  ( -11.64999999999999858, 2.500000000000000000, -5.802370205355746435 ) ) ;
#82964 = CARTESIAN_POINT ( 'NONE',  ( 2.499999999999948930, 2.500000000000000000, -0.6928203230275541413 ) ) ;
#82965 = EDGE_CURVE ( 'NONE', #24381, #125995, #86871, .T. ) ;
#82966 = DIRECTION ( 'NONE',  ( 0.000000000000000000, 0.000000000000000000, 1.000000000000000000 ) ) ;
#82968 = EDGE_CURVE ( 'NONE', #15244, #58440, #93153, .T. ) ;
#82967 = CARTESIAN_POINT ( 'NONE',  ( 4.999999999999969802, 12.50000000000000000, 4.265033745738159077 ) ) ;
#82969 = EDGE_CURVE ( 'NONE', #38921, #99960, #72318, .T. ) ;
#82970 = CARTESIAN_POINT ( 'NONE',  ( -6.249999999999984901, 12.50000000000000000, -6.495190528383302464 ) ) ;
#82971 = EDGE_CURVE ( 'NONE', #118702, #29739, #126603, .T. ) ;
#82972 = ORIENTED_EDGE ( 'NONE', *, *, #39529, .T. ) ;
#82975 = ORIENTED_EDGE ( 'NONE', *, *, #46810, .F. ) ;
#82974 = VECTOR ( 'NONE', #54721, 1000.000000000000000 ) ;
#82973 = CIRCLE ( 'NONE', #72509, 0.09999999999999982514 ) ;
#82976 = CARTESIAN_POINT ( 'NONE',  ( 2.049999999999950084, 12.50000000000000000, -2.165063509461101710 ) ) ;
#82977 = DIRECTION ( 'NONE',  ( 0.000000000000000000, -1.000000000000000000, 0.000000000000000000 ) ) ;
#82978 = EDGE_CURVE ( 'NONE', #70528, #121075, #76423, .T. ) ;
#82979 = CARTESIAN_POINT ( 'NONE',  ( 105.6184301395928031, 8.500000000000000000, 1.375000000000001110 ) ) ;
#82980 = ORIENTED_EDGE ( 'NONE', *, *, #116488, .F. ) ;
#82981 = VERTEX_POINT ( 'NONE', #124632 ) ;
#82982 = EDGE_CURVE ( 'NONE', #89637, #117873, #17917, .T. ) ;
#82983 = CONICAL_SURFACE ( 'NONE', #62054, 0.1000000000000000056, 0.003490658503988666988 ) ;
#82984 = PLANE ( 'NONE',  #68727 ) ;
#82986 = AXIS2_PLACEMENT_3D ( 'NONE', #32053, #92226, #11744 ) ;
#82985 = CIRCLE ( 'NONE', #41228, 0.06509327318403745899 ) ;
#82987 = ORIENTED_EDGE ( 'NONE', *, *, #60362, .F. ) ;
#82988 = DIRECTION ( 'NONE',  ( 0.000000000000000000, 0.000000000000000000, -1.000000000000000000 ) ) ;
#82989 = DIRECTION ( 'NONE',  ( -4.274815082592931898E-19, -0.9999939076577903929, -0.003490651415223739937 ) ) ;
#82990 = ADVANCED_FACE ( 'NONE', ( #64415 ), #33675, .T. ) ;
#82991 = EDGE_CURVE ( 'NONE', #31157, #40264, #112017, .T. ) ;
#82992 = DIRECTION ( 'NONE',  ( 0.000000000000000000, 1.000000000000000000, 0.000000000000000000 ) ) ;
#82993 = EDGE_LOOP ( 'NONE', ( #10917, #91753, #107466, #42455 ) ) ;
#82994 = DIRECTION ( 'NONE',  ( 0.000000000000000000, 0.000000000000000000, 1.000000000000000000 ) ) ;
#82995 = DIRECTION ( 'NONE',  ( -0.000000000000000000, -1.000000000000000000, -0.000000000000000000 ) ) ;
#82996 = CARTESIAN_POINT ( 'NONE',  ( -5.200000000000020606, 12.50000000000000000, -0.2813168883297408329 ) ) ;
#82997 = CARTESIAN_POINT ( 'NONE',  ( -2.900000000000029665, 12.50000000000000000, 4.265033745738159077 ) ) ;
#82999 = EDGE_CURVE ( 'NONE', #37147, #37160, #34337, .T. ) ;
#82998 = FACE_OUTER_BOUND ( 'NONE', #90602, .T. ) ;
#83000 = VERTEX_POINT ( 'NONE', #63787 ) ;
#83001 = DIRECTION ( 'NONE',  ( 0.000000000000000000, -0.9999939076577903929, 0.003490651415223739937 ) ) ;
#83002 = CARTESIAN_POINT ( 'NONE',  ( 23.85240649353151454, -2.660544618004264006, 4.258220037302151262 ) ) ;
#83003 = ORIENTED_EDGE ( 'NONE', *, *, #72640, .F. ) ;
#83004 = VERTEX_POINT ( 'NONE', #34984 ) ;
#83005 = CARTESIAN_POINT ( 'NONE',  ( 184.6927083336747160, 6.551208109652275624, -3.782341765624998686 ) ) ;
#83006 = DIRECTION ( 'NONE',  ( 0.000000000000000000, 0.000000000000000000, 1.000000000000000000 ) ) ;
#83007 = AXIS2_PLACEMENT_3D ( 'NONE', #95987, #86804, #114330 ) ;
#83008 = CARTESIAN_POINT ( 'NONE',  ( -12.09999999999999609, 2.500000000000000000, -0.6928203230275501445 ) ) ;
#83009 = AXIS2_PLACEMENT_3D ( 'NONE', #43203, #90993, #101464 ) ;
#83011 = CONICAL_SURFACE ( 'NONE', #34990, 0.1000000000000000056, 0.003490658503988666988 ) ;
#83010 = CARTESIAN_POINT ( 'NONE',  ( 8.549999999999918998, 12.50000000000000000, 6.841600689897072485 ) ) ;
#83012 = DIRECTION ( 'NONE',  ( 0.000000000000000000, 0.000000000000000000, 1.000000000000000000 ) ) ;
#83013 = DIRECTION ( 'NONE',  ( 0.000000000000000000, 0.000000000000000000, 1.000000000000000000 ) ) ;
#83014 = AXIS2_PLACEMENT_3D ( 'NONE', #4790, #4143, #114120 ) ;
#83015 = DIRECTION ( 'NONE',  ( -0.000000000000000000, 1.000000000000000000, -0.000000000000000000 ) ) ;
#83016 = DIRECTION ( 'NONE',  ( 0.000000000000000000, 0.000000000000000000, -1.000000000000000000 ) ) ;
#83017 = DIRECTION ( 'NONE',  ( -0.000000000000000000, -1.000000000000000000, -0.000000000000000000 ) ) ;
#83018 = VECTOR ( 'NONE', #13527, 1000.000000000000000 ) ;
#83019 = VECTOR ( 'NONE', #6911, 1000.000000000000000 ) ;
#83020 = CARTESIAN_POINT ( 'NONE',  ( 0.8499999999999550138, 2.500000000000000000, -5.902370205355750521 ) ) ;
#83021 = ORIENTED_EDGE ( 'NONE', *, *, #40064, .F. ) ;
#83022 = ORIENTED_EDGE ( 'NONE', *, *, #24267, .T. ) ;
#83023 = AXIS2_PLACEMENT_3D ( 'NONE', #94287, #104739, #102810 ) ;
#83024 = ORIENTED_EDGE ( 'NONE', *, *, #46870, .T. ) ;
#83025 = ORIENTED_EDGE ( 'NONE', *, *, #42020, .T. ) ;
#83026 = DIRECTION ( 'NONE',  ( 0.000000000000000000, 0.000000000000000000, 1.000000000000000000 ) ) ;
#83027 = CARTESIAN_POINT ( 'NONE',  ( -8.950000000000008171, 2.500000000000000000, 1.818653347947321475 ) ) ;
#83028 = VECTOR ( 'NONE', #110106, 1000.000000000000000 ) ;
#83029 = ORIENTED_EDGE ( 'NONE', *, *, #88429, .T. ) ;
#83030 = CARTESIAN_POINT ( 'NONE',  ( 4.599999999999936584, 2.500000000000000000, 3.637306695894644726 ) ) ;
#83031 = EDGE_CURVE ( 'NONE', #92919, #37333, #45122, .T. ) ;
#83033 = AXIS2_PLACEMENT_3D ( 'NONE', #120925, #36747, #78609 ) ;
#83032 = AXIS2_PLACEMENT_3D ( 'NONE', #46761, #114206, #46107 ) ;
#83034 = ADVANCED_FACE ( 'NONE', ( #74891 ), #36718, .T. ) ;
#83035 = CARTESIAN_POINT ( 'NONE',  ( -0.8000000000000376810, 2.500000000000000000, -4.430127018922202176 ) ) ;
#83037 = EDGE_LOOP ( 'NONE', ( #125260, #61522, #128512, #95160 ) ) ;
#83036 = CARTESIAN_POINT ( 'NONE',  ( -3.300000000000027800, 12.50000000000000000, -0.06509327318403970719 ) ) ;
#83038 = CARTESIAN_POINT ( 'NONE',  ( -4.150000000000024336, 12.50000000000000000, -2.165063509461101710 ) ) ;
#83039 = CARTESIAN_POINT ( 'NONE',  ( 2.899999999999943956, 12.50000000000000000, 4.330127018922196314 ) ) ;
#83040 = ORIENTED_EDGE ( 'NONE', *, *, #79411, .T. ) ;
#83041 = ORIENTED_EDGE ( 'NONE', *, *, #92525, .F. ) ;
#83042 = VERTEX_POINT ( 'NONE', #103711 ) ;
#83043 = ORIENTED_EDGE ( 'NONE', *, *, #51888, .F. ) ;
#83044 = CARTESIAN_POINT ( 'NONE',  ( -14.79999999999998472, 12.50000000000000000, 0.2813168883297384459 ) ) ;
#83045 = AXIS2_PLACEMENT_3D ( 'NONE', #113044, #124156, #23365 ) ;
#83046 = FACE_OUTER_BOUND ( 'NONE', #69165, .T. ) ;
#83047 = CARTESIAN_POINT ( 'NONE',  ( 5.399999999999936406, 12.50000000000000000, -3.637306695894650055 ) ) ;
#83048 = DIRECTION ( 'NONE',  ( 0.000000000000000000, 0.000000000000000000, 1.000000000000000000 ) ) ;
#83049 = ORIENTED_EDGE ( 'NONE', *, *, #66839, .F. ) ;
#83050 = CARTESIAN_POINT ( 'NONE',  ( -11.89999999999999680, 12.50000000000000000, -3.918623584224386391 ) ) ;
#83051 = VERTEX_POINT ( 'NONE', #15294 ) ;
#83052 = DIRECTION ( 'NONE',  ( 0.000000000000000000, 1.000000000000000000, 0.000000000000000000 ) ) ;
#83053 = CARTESIAN_POINT ( 'NONE',  ( 8.497934422427476875, -1.500000000000508038, -9.526046680185665139 ) ) ;
#83054 = DIRECTION ( 'NONE',  ( 0.000000000000000000, -0.9999939076577903929, 0.003490651415223739937 ) ) ;
#83055 = FACE_OUTER_BOUND ( 'NONE', #49480, .T. ) ;
#83056 = VERTEX_POINT ( 'NONE', #12721 ) ;
#83057 = CONICAL_SURFACE ( 'NONE', #95568, 0.1000000000000002554, 0.003490658503988666988 ) ;
#83058 = CIRCLE ( 'NONE', #76787, 0.09999999999999982514 ) ;
#83059 = VERTEX_POINT ( 'NONE', #104964 ) ;
#83060 = VERTEX_POINT ( 'NONE', #13378 ) ;
#83061 = DIRECTION ( 'NONE',  ( 0.000000000000000000, 0.000000000000000000, 1.000000000000000000 ) ) ;
#83062 = PLANE ( 'NONE',  #64450 ) ;
#83063 = CARTESIAN_POINT ( 'NONE',  ( 9.349999999999916156, 2.500000000000000000, -1.918653347947326004 ) ) ;
#83064 = FACE_BOUND ( 'NONE', #59683, .T. ) ;
#83065 = DIRECTION ( 'NONE',  ( -0.000000000000000000, -1.000000000000000000, -0.000000000000000000 ) ) ;
#83066 = DIRECTION ( 'NONE',  ( 0.000000000000000000, 1.000000000000000000, 0.000000000000000000 ) ) ;
#83068 = CIRCLE ( 'NONE', #93521, 0.06509327318403743123 ) ;
#83067 = CIRCLE ( 'NONE', #37092, 4.500000000000003553 ) ;
#83069 = LINE ( 'NONE', #122987, #127298 ) ;
#83070 = EDGE_CURVE ( 'NONE', #76977, #80050, #53960, .T. ) ;
#83071 = CIRCLE ( 'NONE', #76800, 0.06509327318403745899 ) ;
#83072 = FACE_OUTER_BOUND ( 'NONE', #51094, .T. ) ;
#83073 = CARTESIAN_POINT ( 'NONE',  ( 1.649999999999950617, 2.500000000000000000, -2.165063509461101710 ) ) ;
#83074 = FACE_OUTER_BOUND ( 'NONE', #19599, .T. ) ;
#83075 = ORIENTED_EDGE ( 'NONE', *, *, #60865, .F. ) ;
#83077 = AXIS2_PLACEMENT_3D ( 'NONE', #83719, #14305, #75807 ) ;
#83076 = AXIS2_PLACEMENT_3D ( 'NONE', #52114, #1064, #80287 ) ;
#83078 = AXIS2_PLACEMENT_3D ( 'NONE', #76812, #116717, #27064 ) ;
#83079 = DIRECTION ( 'NONE',  ( -0.000000000000000000, 1.000000000000000000, -0.000000000000000000 ) ) ;
#83080 = ORIENTED_EDGE ( 'NONE', *, *, #125839, .F. ) ;
#83081 = VERTEX_POINT ( 'NONE', #95172 ) ;
#83082 = EDGE_CURVE ( 'NONE', #78931, #10631, #72958, .T. ) ;
#83083 = CARTESIAN_POINT ( 'NONE',  ( 7.699999999999925571, 12.50000000000000000, 3.983716857408420076 ) ) ;
#83085 = EDGE_CURVE ( 'NONE', #97899, #73263, #2933, .T. ) ;
#83084 = CARTESIAN_POINT ( 'NONE',  ( 3.749999999999978684, 12.50000000000000000, -2.165063509461101710 ) ) ;
#83086 = FACE_BOUND ( 'NONE', #98690, .T. ) ;
#83087 = DIRECTION ( 'NONE',  ( 0.000000000000000000, 1.000000000000000000, 0.000000000000000000 ) ) ;
#83088 = AXIS2_PLACEMENT_3D ( 'NONE', #1624, #41586, #121403 ) ;
#83089 = VERTEX_POINT ( 'NONE', #103045 ) ;
#83090 = CARTESIAN_POINT ( 'NONE',  ( 65.40459994261938448, 3.824478557803584700, 5.306485876514984490 ) ) ;
#83091 = EDGE_CURVE ( 'NONE', #38337, #69557, #103616, .T. ) ;
#83092 = CARTESIAN_POINT ( 'NONE',  ( -11.69999999999999574, 2.500000000000000000, 4.430127018922196847 ) ) ;
#83093 = CIRCLE ( 'NONE', #43394, 0.06509327318403745899 ) ;
#83094 = ORIENTED_EDGE ( 'NONE', *, *, #28112, .T. ) ;
#83095 = DIRECTION ( 'NONE',  ( 0.000000000000000000, -0.000000000000000000, 1.000000000000000000 ) ) ;
#83096 = AXIS2_PLACEMENT_3D ( 'NONE', #87775, #50439, #19032 ) ;
#83097 = DIRECTION ( 'NONE',  ( 0.000000000000000000, -0.000000000000000000, 1.000000000000000000 ) ) ;
#83098 = AXIS2_PLACEMENT_3D ( 'NONE', #67719, #38954, #128620 ) ;
#83099 = EDGE_LOOP ( 'NONE', ( #4059, #49697 ) ) ;
#83100 = PLANE ( 'NONE',  #115446 ) ;
#83101 = CARTESIAN_POINT ( 'NONE',  ( -11.64999999999999680, 12.50000000000000000, -6.495190528383298911 ) ) ;
#83102 = AXIS2_PLACEMENT_3D ( 'NONE', #34339, #3565, #33676 ) ;
#83103 = AXIS2_PLACEMENT_3D ( 'NONE', #78927, #30476, #70378 ) ;
#83104 = ORIENTED_EDGE ( 'NONE', *, *, #5892, .T. ) ;
#83105 = CIRCLE ( 'NONE', #127116, 0.1000000000000000472 ) ;
#83106 = DIRECTION ( 'NONE',  ( 0.000000000000000000, 0.000000000000000000, 1.000000000000000000 ) ) ;
#83107 = DIRECTION ( 'NONE',  ( 0.000000000000000000, 0.000000000000000000, -1.000000000000000000 ) ) ;
#83108 = CARTESIAN_POINT ( 'NONE',  ( -8.950000000000009948, 12.50000000000000000, -6.841600689897072485 ) ) ;
#83109 = VERTEX_POINT ( 'NONE', #115419 ) ;
#83110 = EDGE_LOOP ( 'NONE', ( #38712, #90417, #9067, #48801 ) ) ;
#83111 = CIRCLE ( 'NONE', #32955, 0.1000000000000002554 ) ;
#83112 = DIRECTION ( 'NONE',  ( 1.000000000000000000, 0.000000000000000000, 0.000000000000000000 ) ) ;
#83113 = EDGE_LOOP ( 'NONE', ( #82114, #89558 ) ) ;
#83114 = DIRECTION ( 'NONE',  ( 0.000000000000000000, 1.000000000000000000, 0.000000000000000000 ) ) ;
#83115 = CARTESIAN_POINT ( 'NONE',  ( 13.94999999999989804, 12.50000000000000000, 1.818653347947321475 ) ) ;
#83116 = ADVANCED_FACE ( 'NONE', ( #125900 ), #75513, .T. ) ;
#83118 = VECTOR ( 'NONE', #32576, 1000.000000000000000 ) ;
#83117 = CIRCLE ( 'NONE', #112459, 0.06509327318403745899 ) ;
#83119 = ORIENTED_EDGE ( 'NONE', *, *, #85053, .F. ) ;
#83120 = DIRECTION ( 'NONE',  ( 0.000000000000000000, 0.000000000000000000, 1.000000000000000000 ) ) ;
#83121 = PLANE ( 'NONE',  #20537 ) ;
#83122 = DIRECTION ( 'NONE',  ( -4.274815082592931898E-19, -0.9999939076577903929, -0.003490651415223739937 ) ) ;
#83123 = DIRECTION ( 'NONE',  ( -4.274815082592931898E-19, -0.9999939076577903929, -0.003490651415223739937 ) ) ;
#83124 = APPLICATION_CONTEXT ( 'automotive_design' ) ;
#83125 = EDGE_CURVE ( 'NONE', #16607, #46996, #87532, .T. ) ;
#83126 = FACE_OUTER_BOUND ( 'NONE', #100485, .T. ) ;
#83127 = EDGE_CURVE ( 'NONE', #102950, #111853, #106907, .T. ) ;
#83128 = EDGE_LOOP ( 'NONE', ( #50994, #69739, #81957, #60105 ) ) ;
#83129 = EDGE_LOOP ( 'NONE', ( #55806, #94367 ) ) ;
#83130 = CARTESIAN_POINT ( 'NONE',  ( -1.700000000000034817, 12.50000000000000000, -4.395220292106239768 ) ) ;
#83131 = ORIENTED_EDGE ( 'NONE', *, *, #58004, .F. ) ;
#83132 = PLANE ( 'NONE',  #89001 ) ;
#83133 = EDGE_CURVE ( 'NONE', #19378, #123253, #53441, .T. ) ;
#83135 = ORIENTED_EDGE ( 'NONE', *, *, #913, .F. ) ;
#83134 = ORIENTED_EDGE ( 'NONE', *, *, #110163, .T. ) ;
#83136 = EDGE_CURVE ( 'NONE', #18239, #122843, #6128, .T. ) ;
#83137 = ORIENTED_EDGE ( 'NONE', *, *, #46600, .T. ) ;
#83138 = ADVANCED_FACE ( 'NONE', ( #106277 ), #78585, .T. ) ;
#83139 = CIRCLE ( 'NONE', #30824, 0.1000000000000002554 ) ;
#83140 = CARTESIAN_POINT ( 'NONE',  ( -7.900000000000014566, 2.500000000000000000, -4.230127018922201998 ) ) ;
#83141 = DIRECTION ( 'NONE',  ( 0.000000000000000000, 0.000000000000000000, -1.000000000000000000 ) ) ;
#83142 = PLANE ( 'NONE',  #45629 ) ;
#83143 =( NAMED_UNIT ( * ) SI_UNIT ( $, .STERADIAN. ) SOLID_ANGLE_UNIT ( ) );
#83144 = EDGE_CURVE ( 'NONE', #18181, #103538, #79652, .T. ) ;
#83145 = DIRECTION ( 'NONE',  ( 0.000000000000000000, 1.000000000000000000, 0.000000000000000000 ) ) ;
#83146 = DIRECTION ( 'NONE',  ( 0.000000000000000000, 1.000000000000000000, 0.000000000000000000 ) ) ;
#83147 = DIRECTION ( 'NONE',  ( 0.000000000000000000, 1.000000000000000000, 0.000000000000000000 ) ) ;
#83148 = CARTESIAN_POINT ( 'NONE',  ( 127.5000000000000000, 1.500000000000000000, -2.598076211353316900 ) ) ;
#83149 = CARTESIAN_POINT ( 'NONE',  ( 6.449999999999930012, 2.500000000000000000, -1.818653347947326138 ) ) ;
#83151 = ADVANCED_FACE ( 'NONE', ( #17888 ), #96439, .T. ) ;
#83150 = CARTESIAN_POINT ( 'NONE',  ( -11.89999999999999680, 12.50000000000000000, 0.3464101615137776813 ) ) ;
#83153 = ORIENTED_EDGE ( 'NONE', *, *, #111325, .T. ) ;
#83152 = CIRCLE ( 'NONE', #70515, 0.06509327318403745899 ) ;
#83154 = CIRCLE ( 'NONE', #45585, 0.1000000000000002554 ) ;
#83155 = DIRECTION ( 'NONE',  ( 0.000000000000000000, -0.000000000000000000, 1.000000000000000000 ) ) ;
#83156 = ORIENTED_EDGE ( 'NONE', *, *, #79971, .F. ) ;
#83157 = ORIENTED_EDGE ( 'NONE', *, *, #3712, .T. ) ;
#83158 = DIRECTION ( 'NONE',  ( -0.000000000000000000, 1.000000000000000000, -0.000000000000000000 ) ) ;
#83159 = DIRECTION ( 'NONE',  ( 0.000000000000000000, 0.000000000000000000, 1.000000000000000000 ) ) ;
#83160 = DIRECTION ( 'NONE',  ( -0.000000000000000000, 1.000000000000000000, -0.000000000000000000 ) ) ;
#83161 = CIRCLE ( 'NONE', #26715, 0.06509327318403745899 ) ;
#83162 = FACE_OUTER_BOUND ( 'NONE', #79133, .T. ) ;
#83163 = VECTOR ( 'NONE', #62362, 1000.000000000000000 ) ;
#83164 = DIRECTION ( 'NONE',  ( -4.274815082592931898E-19, -0.9999939076577903929, -0.003490651415223739937 ) ) ;
#83165 = LINE ( 'NONE', #22949, #105483 ) ;
#83166 = CARTESIAN_POINT ( 'NONE',  ( 15.39999999999989200, 12.50000000000000000, 0.6928203230275494784 ) ) ;
#83167 = VERTEX_POINT ( 'NONE', #6751 ) ;
#83168 = CARTESIAN_POINT ( 'NONE',  ( -3.350000000000028955, 2.500000000000000000, 7.088010851410848190 ) ) ;
#83169 = ORIENTED_EDGE ( 'NONE', *, *, #93447, .T. ) ;
#83170 = AXIS2_PLACEMENT_3D ( 'NONE', #1305, #19666, #658 ) ;
#83171 = EDGE_LOOP ( 'NONE', ( #55434, #48042, #8793, #21068 ) ) ;
#83172 = VERTEX_POINT ( 'NONE', #46713 ) ;
#83173 = AXIS2_PLACEMENT_3D ( 'NONE', #107635, #47433, #89283 ) ;
#83174 = ORIENTED_EDGE ( 'NONE', *, *, #117951, .T. ) ;
#83175 = DIRECTION ( 'NONE',  ( 0.000000000000000000, 0.000000000000000000, 1.000000000000000000 ) ) ;
#83176 = CARTESIAN_POINT ( 'NONE',  ( -10.80000000000000071, 12.50000000000000000, 4.265033745738159077 ) ) ;
#83177 = VECTOR ( 'NONE', #123, 1000.000000000000000 ) ;
#83178 = DIRECTION ( 'NONE',  ( -0.000000000000000000, 1.000000000000000000, -0.000000000000000000 ) ) ;
#83179 = EDGE_CURVE ( 'NONE', #42996, #14604, #8694, .T. ) ;
#83180 = CARTESIAN_POINT ( 'NONE',  ( 2.499999999999983569, 2.500000000000000000, -4.330127018922201643 ) ) ;
#83181 = MECHANICAL_DESIGN_GEOMETRIC_PRESENTATION_REPRESENTATION (  '', ( #66523 ), #43573 ) ;
#83182 = PLANE ( 'NONE',  #99442 ) ;
#83183 = EDGE_LOOP ( 'NONE', ( #50492, #93917 ) ) ;
#83184 = PLANE ( 'NONE',  #1393 ) ;
#83185 = DIRECTION ( 'NONE',  ( -0.000000000000000000, -1.000000000000000000, -0.000000000000000000 ) ) ;
#83186 = CARTESIAN_POINT ( 'NONE',  ( 4.349999999999941025, 2.500000000000000000, -6.248780366869526759 ) ) ;
#83187 = CIRCLE ( 'NONE', #16339, 0.1000000000000002554 ) ;
#83188 = VECTOR ( 'NONE', #54947, 1000.000000000000000 ) ;
#83190 = EDGE_CURVE ( 'NONE', #98077, #104184, #57640, .T. ) ;
#83189 = CARTESIAN_POINT ( 'NONE',  ( 0.7999999999999612976, 12.50000000000000000, -0.06509327318403752838 ) ) ;
#83191 = ORIENTED_EDGE ( 'NONE', *, *, #44977, .F. ) ;
#83192 = CIRCLE ( 'NONE', #28811, 0.06509327318403741736 ) ;
#83193 = EDGE_LOOP ( 'NONE', ( #102692, #104226 ) ) ;
#83194 = ORIENTED_EDGE ( 'NONE', *, *, #4358, .T. ) ;
#83195 = DIRECTION ( 'NONE',  ( -0.000000000000000000, 1.000000000000000000, -0.000000000000000000 ) ) ;
#83196 = AXIS2_PLACEMENT_3D ( 'NONE', #66344, #36906, #66974 ) ;
#83197 = AXIS2_PLACEMENT_3D ( 'NONE', #6755, #35617, #76183 ) ;
#83198 = CARTESIAN_POINT ( 'NONE',  ( 3.349999999999945466, 12.50000000000000000, -2.922977105672691422 ) ) ;
#83199 = DIRECTION ( 'NONE',  ( 0.000000000000000000, 0.000000000000000000, -1.000000000000000000 ) ) ;
#83200 = ORIENTED_EDGE ( 'NONE', *, *, #16369, .T. ) ;
#83201 = DIRECTION ( 'NONE',  ( 0.000000000000000000, -0.9999939076577903929, 0.003490651415223739937 ) ) ;
#83203 = AXIS2_PLACEMENT_3D ( 'NONE', #64606, #26620, #46250 ) ;
#83202 = CARTESIAN_POINT ( 'NONE',  ( 1.249999999999954259, 2.500000000000000000, -7.188010851410854052 ) ) ;
#83204 = CARTESIAN_POINT ( 'NONE',  ( -6.700000000000016165, 12.50000000000000000, 4.265033745738159077 ) ) ;
#83205 = DIRECTION ( 'NONE',  ( 0.000000000000000000, 1.000000000000000000, 0.000000000000000000 ) ) ;
#83207 = CIRCLE ( 'NONE', #45555, 0.06509327318403741736 ) ;
#83206 = CIRCLE ( 'NONE', #22586, 0.1000000000000002554 ) ;
#83208 = CARTESIAN_POINT ( 'NONE',  ( 1.649999999999950617, 2.500000000000000000, -2.065063509461102065 ) ) ;
#83209 = VERTEX_POINT ( 'NONE', #65703 ) ;
#83210 = EDGE_LOOP ( 'NONE', ( #85530, #24074, #38417, #38199 ) ) ;
#83211 = CARTESIAN_POINT ( 'NONE',  ( 10.19999999999991047, 2.500000000000000000, -3.983716857408426293 ) ) ;
#83212 = DIRECTION ( 'NONE',  ( -0.000000000000000000, -1.000000000000000000, -0.000000000000000000 ) ) ;
#83213 = DIRECTION ( 'NONE',  ( -0.000000000000000000, 1.000000000000000000, -0.000000000000000000 ) ) ;
#83214 = CARTESIAN_POINT ( 'NONE',  ( 7.049999999999930544, 2.500000000000000000, -6.495190528383302464 ) ) ;
#83215 = FACE_OUTER_BOUND ( 'NONE', #100339, .T. ) ;
#83216 = EDGE_CURVE ( 'NONE', #33924, #103702, #15855, .T. ) ;
#83217 = ORIENTED_EDGE ( 'NONE', *, *, #116818, .T. ) ;
#83218 = ORIENTED_EDGE ( 'NONE', *, *, #79715, .T. ) ;
#83219 = CARTESIAN_POINT ( 'NONE',  ( 5.199999999999937117, 2.500000000000000000, -4.676537180435978769 ) ) ;
#83220 = DIRECTION ( 'NONE',  ( 0.000000000000000000, 1.000000000000000000, 0.000000000000000000 ) ) ;
#83221 = DIRECTION ( 'NONE',  ( 0.000000000000000000, 0.000000000000000000, 1.000000000000000000 ) ) ;
#83222 = DIRECTION ( 'NONE',  ( 0.000000000000000000, 0.000000000000000000, 1.000000000000000000 ) ) ;
#83223 = DIRECTION ( 'NONE',  ( 0.000000000000000000, 1.000000000000000000, 0.000000000000000000 ) ) ;
#83224 = ORIENTED_EDGE ( 'NONE', *, *, #15513, .F. ) ;
#83225 = EDGE_CURVE ( 'NONE', #56742, #114427, #47176, .T. ) ;
#83226 = FACE_OUTER_BOUND ( 'NONE', #52622, .T. ) ;
#83227 = DIRECTION ( 'NONE',  ( -0.000000000000000000, 1.000000000000000000, -0.000000000000000000 ) ) ;
#83228 = AXIS2_PLACEMENT_3D ( 'NONE', #50421, #100794, #90326 ) ;
#83229 = ORIENTED_EDGE ( 'NONE', *, *, #25325, .T. ) ;
#83231 = EDGE_CURVE ( 'NONE', #55407, #23165, #7448, .T. ) ;
#83230 = CIRCLE ( 'NONE', #104150, 0.06509327318403745899 ) ;
#83232 = CARTESIAN_POINT ( 'NONE',  ( 5.399999999999931966, 2.500000000000000000, 4.230127018922196669 ) ) ;
#83233 = ADVANCED_FACE ( 'NONE', ( #78113 ), #35613, .T. ) ;
#83234 = EDGE_LOOP ( 'NONE', ( #63465, #111012, #83829, #35937 ) ) ;
#83235 = DIRECTION ( 'NONE',  ( 0.000000000000000000, 1.000000000000000000, 0.000000000000000000 ) ) ;
#83236 = VECTOR ( 'NONE', #80726, 1000.000000000000000 ) ;
#83237 = AXIS2_PLACEMENT_3D ( 'NONE', #65475, #105415, #5895 ) ;
#83238 = ORIENTED_EDGE ( 'NONE', *, *, #46770, .F. ) ;
#83239 = PLANE ( 'NONE',  #102934 ) ;
#83240 = FACE_OUTER_BOUND ( 'NONE', #19453, .T. ) ;
#83241 = EDGE_CURVE ( 'NONE', #127171, #13735, #105641, .T. ) ;
#83242 = ORIENTED_EDGE ( 'NONE', *, *, #116844, .T. ) ;
#83243 = ORIENTED_EDGE ( 'NONE', *, *, #118872, .F. ) ;
#83244 = EDGE_CURVE ( 'NONE', #74924, #48671, #105754, .T. ) ;
#83245 = CARTESIAN_POINT ( 'NONE',  ( 184.6718750003414016, 9.264065473108010111E-16, -7.564683531250000925 ) ) ;
#83246 = DIRECTION ( 'NONE',  ( -0.000000000000000000, -1.000000000000000000, -0.000000000000000000 ) ) ;
#83247 = AXIS2_PLACEMENT_3D ( 'NONE', #113804, #116363, #45712 ) ;
#83248 = CARTESIAN_POINT ( 'NONE',  ( 11.84999999999990372, 2.500000000000000000, 1.918653347947321564 ) ) ;
#83249 = CARTESIAN_POINT ( 'NONE',  ( 184.1927083336747160, 6.551208109652275624, -3.782341765624998686 ) ) ;
#83250 = AXIS2_PLACEMENT_3D ( 'NONE', #119106, #77876, #20261 ) ;
#83251 = FACE_OUTER_BOUND ( 'NONE', #101208, .T. ) ;
#83252 = FACE_OUTER_BOUND ( 'NONE', #85642, .T. ) ;
#83253 = DIRECTION ( 'NONE',  ( 0.000000000000000000, 1.000000000000000000, 0.000000000000000000 ) ) ;
#83254 = DIRECTION ( 'NONE',  ( -0.000000000000000000, 1.000000000000000000, -0.000000000000000000 ) ) ;
#83255 = VECTOR ( 'NONE', #38533, 1000.000000000000000 ) ;
#83256 = ORIENTED_EDGE ( 'NONE', *, *, #30653, .F. ) ;
#83257 = ORIENTED_EDGE ( 'NONE', *, *, #68880, .T. ) ;
#83258 = DIRECTION ( 'NONE',  ( -0.000000000000000000, 1.000000000000000000, -0.000000000000000000 ) ) ;
#83259 = VERTEX_POINT ( 'NONE', #37550 ) ;
#83260 = CARTESIAN_POINT ( 'NONE',  ( 187.4166666666666856, 6.668395609140176816, 3.850000000000000977 ) ) ;
#83261 = DIRECTION ( 'NONE',  ( -0.000000000000000000, -1.000000000000000000, -0.000000000000000000 ) ) ;
#83262 = AXIS2_PLACEMENT_3D ( 'NONE', #92493, #102957, #111490 ) ;
#83263 = CARTESIAN_POINT ( 'NONE',  ( -2.900000000000029665, 2.500000000000000000, 4.230127018922196669 ) ) ;
#83265 = VERTEX_POINT ( 'NONE', #72175 ) ;
#83264 = VERTEX_POINT ( 'NONE', #77458 ) ;
#83266 = LINE ( 'NONE', #103549, #108048 ) ;
#83267 = VERTEX_POINT ( 'NONE', #49966 ) ;
#83268 = DIRECTION ( 'NONE',  ( 0.000000000000000000, 0.000000000000000000, 1.000000000000000000 ) ) ;
#83269 = LINE ( 'NONE', #32249, #54033 ) ;
#83270 = FACE_OUTER_BOUND ( 'NONE', #1459, .T. ) ;
#83271 = VECTOR ( 'NONE', #100690, 1000.000000000000000 ) ;
#83272 = CARTESIAN_POINT ( 'NONE',  ( 1.699999999999950218, 12.50000000000000000, 4.395220292106234439 ) ) ;
#83273 = LINE ( 'NONE', #115262, #38873 ) ;
#83274 = DIRECTION ( 'NONE',  ( 0.000000000000000000, 0.000000000000000000, 1.000000000000000000 ) ) ;
#83275 = DIRECTION ( 'NONE',  ( 0.000000000000000000, -0.000000000000000000, 1.000000000000000000 ) ) ;
#83276 = DIRECTION ( 'NONE',  ( 0.000000000000000000, 0.000000000000000000, 1.000000000000000000 ) ) ;
#83277 = DIRECTION ( 'NONE',  ( 0.000000000000000000, 0.000000000000000000, 1.000000000000000000 ) ) ;
#83278 = CARTESIAN_POINT ( 'NONE',  ( 6.249999999999965361, 12.50000000000000000, 2.099970236277060032 ) ) ;
#83279 = AXIS2_PLACEMENT_3D ( 'NONE', #104057, #14366, #116439 ) ;
#83280 = DIRECTION ( 'NONE',  ( 0.000000000000000000, 0.000000000000000000, 1.000000000000000000 ) ) ;
#83281 = ADVANCED_FACE ( 'NONE', ( #177 ), #97342, .T. ) ;
#83282 = VERTEX_POINT ( 'NONE', #52513 ) ;
#83284 = ORIENTED_EDGE ( 'NONE', *, *, #16460, .F. ) ;
#83283 = CIRCLE ( 'NONE', #87457, 0.09999999999999982514 ) ;
#83285 = ORIENTED_EDGE ( 'NONE', *, *, #33156, .F. ) ;
#83286 = PLANE ( 'NONE',  #128589 ) ;
#83287 = ORIENTED_EDGE ( 'NONE', *, *, #95097, .T. ) ;
#83288 = DIRECTION ( 'NONE',  ( 0.000000000000000000, -0.000000000000000000, 1.000000000000000000 ) ) ;
#83289 = EDGE_CURVE ( 'NONE', #120080, #71030, #19989, .T. ) ;
#83291 = ORIENTED_EDGE ( 'NONE', *, *, #18812, .F. ) ;
#83290 = ORIENTED_EDGE ( 'NONE', *, *, #101860, .T. ) ;
#83292 = ORIENTED_EDGE ( 'NONE', *, *, #62702, .F. ) ;
#83293 = CIRCLE ( 'NONE', #81228, 0.06509327318403745899 ) ;
#83294 = ADVANCED_FACE ( 'NONE', ( #51887 ), #32261, .T. ) ;
#83295 = DIRECTION ( 'NONE',  ( 0.000000000000000000, 0.000000000000000000, -1.000000000000000000 ) ) ;
#83296 = EDGE_CURVE ( 'NONE', #20888, #85559, #21785, .T. ) ;
#83297 = DIRECTION ( 'NONE',  ( -0.000000000000000000, 1.000000000000000000, -0.000000000000000000 ) ) ;
#83298 =( NAMED_UNIT ( * ) PLANE_ANGLE_UNIT ( ) SI_UNIT ( $, .RADIAN. ) );
#83299 = EDGE_CURVE ( 'NONE', #38578, #65715, #9606, .T. ) ;
#83300 = DIRECTION ( 'NONE',  ( 0.000000000000000000, 1.000000000000000000, 0.000000000000000000 ) ) ;
#83301 = DIRECTION ( 'NONE',  ( 0.000000000000000000, 0.000000000000000000, -1.000000000000000000 ) ) ;
#83302 = DIRECTION ( 'NONE',  ( 0.000000000000000000, 0.000000000000000000, 1.000000000000000000 ) ) ;
#83303 = VERTEX_POINT ( 'NONE', #81348 ) ;
#83305 = EDGE_CURVE ( 'NONE', #73593, #66462, #82788, .T. ) ;
#83304 = DIRECTION ( 'NONE',  ( 0.000000000000000000, 0.000000000000000000, 1.000000000000000000 ) ) ;
#83306 = EDGE_LOOP ( 'NONE', ( #3615, #109746 ) ) ;
#83308 = EDGE_CURVE ( 'NONE', #89740, #47635, #90493, .T. ) ;
#83307 = VECTOR ( 'NONE', #100269, 1000.000000000000000 ) ;
#83309 = ORIENTED_EDGE ( 'NONE', *, *, #90792, .F. ) ;
#83310 = EDGE_LOOP ( 'NONE', ( #120534, #4916, #7150, #107714 ) ) ;
#83311 = DIRECTION ( 'NONE',  ( 0.000000000000000000, -0.9999939076577903929, 0.003490651415223739937 ) ) ;
#83312 = VERTEX_POINT ( 'NONE', #31596 ) ;
#83313 = ORIENTED_EDGE ( 'NONE', *, *, #72630, .F. ) ;
#83314 = ORIENTED_EDGE ( 'NONE', *, *, #31111, .F. ) ;
#83315 = CARTESIAN_POINT ( 'NONE',  ( 127.5000000000000000, 5.000000000000000000, -1.999999999999998224 ) ) ;
#83316 = DIRECTION ( 'NONE',  ( 0.000000000000000000, -0.000000000000000000, 1.000000000000000000 ) ) ;
#83317 = CARTESIAN_POINT ( 'NONE',  ( -13.34999999999999076, 2.500000000000000000, -2.265063509461099578 ) ) ;
#83318 = CARTESIAN_POINT ( 'NONE',  ( 6.649999999999931966, 2.500000000000000000, -5.802370205355749988 ) ) ;
#83319 = CARTESIAN_POINT ( 'NONE',  ( -12.49999999999999289, 12.50000000000000000, -0.6928203230275500335 ) ) ;
#83321 = CIRCLE ( 'NONE', #51927, 0.1000000000000002554 ) ;
#83320 = PLANE ( 'NONE',  #4862 ) ;
#83322 = EDGE_CURVE ( 'NONE', #115754, #21052, #26344, .T. ) ;
#83323 = CARTESIAN_POINT ( 'NONE',  ( 0.8499999999999557909, 12.50000000000000000, -7.188010851410854052 ) ) ;
#83324 = ORIENTED_EDGE ( 'NONE', *, *, #38205, .F. ) ;
#83326 = LINE ( 'NONE', #33580, #50589 ) ;
#83325 = CONICAL_SURFACE ( 'NONE', #72850, 0.1000000000000002554, 0.003490658503988666988 ) ;
#83328 = ORIENTED_EDGE ( 'NONE', *, *, #109890, .F. ) ;
#83327 = VECTOR ( 'NONE', #24239, 1000.000000000000000 ) ;
#83329 = DIRECTION ( 'NONE',  ( 0.000000000000000000, 0.000000000000000000, -1.000000000000000000 ) ) ;
#83330 = AXIS2_PLACEMENT_3D ( 'NONE', #88929, #57538, #99400 ) ;
#83331 = ORIENTED_EDGE ( 'NONE', *, *, #56230, .T. ) ;
#83332 = ORIENTED_EDGE ( 'NONE', *, *, #68211, .F. ) ;
#83334 = CARTESIAN_POINT ( 'NONE',  ( -6.250000000000019540, 12.50000000000000000, -2.857883832488653741 ) ) ;
#83333 = AXIS2_PLACEMENT_3D ( 'NONE', #110941, #71680, #24996 ) ;
#83335 = CARTESIAN_POINT ( 'NONE',  ( 12.29999999999990656, 2.500000000000000000, -4.676537180435977881 ) ) ;
#83336 = CIRCLE ( 'NONE', #60355, 0.1000000000000000056 ) ;
#83337 = AXIS2_PLACEMENT_3D ( 'NONE', #64832, #115872, #113946 ) ;
#83338 = VECTOR ( 'NONE', #102268, 1000.000000000000000 ) ;
#83339 = CARTESIAN_POINT ( 'NONE',  ( -10.84999999999999964, 2.500000000000000000, 2.857883832488649301 ) ) ;
#83340 = ORIENTED_EDGE ( 'NONE', *, *, #111341, .T. ) ;
#83341 = EDGE_LOOP ( 'NONE', ( #73562, #5299, #45823, #93064 ) ) ;
#83342 = DIRECTION ( 'NONE',  ( 0.000000000000000000, 0.000000000000000000, 1.000000000000000000 ) ) ;
#83343 = DIRECTION ( 'NONE',  ( 0.000000000000000000, 1.000000000000000000, 0.000000000000000000 ) ) ;
#83344 = CARTESIAN_POINT ( 'NONE',  ( -1.850000000000033396, 2.500000000000000000, -6.148780366869526226 ) ) ;
#83345 = CARTESIAN_POINT ( 'NONE',  ( 1.899999999999951283, 2.500000000000000000, -4.083716857408426826 ) ) ;
#83346 = AXIS2_PLACEMENT_3D ( 'NONE', #127342, #118148, #37670 ) ;
#83348 = EDGE_CURVE ( 'NONE', #117173, #59532, #2769, .T. ) ;
#83347 = CARTESIAN_POINT ( 'NONE',  ( -11.24999999999996447, 12.50000000000000000, -6.495190528383298911 ) ) ;
#83349 = VECTOR ( 'NONE', #102786, 1000.000000000000000 ) ;
#83350 = ORIENTED_EDGE ( 'NONE', *, *, #10561, .F. ) ;
#83351 = ORIENTED_EDGE ( 'NONE', *, *, #15092, .F. ) ;
#83352 = CARTESIAN_POINT ( 'NONE',  ( -8.750000000000010658, 2.500000000000000000, -7.288010851410849256 ) ) ;
#83354 = CIRCLE ( 'NONE', #87529, 0.06509327318403745899 ) ;
#83353 = DIRECTION ( 'NONE',  ( 0.000000000000000000, 0.000000000000000000, -1.000000000000000000 ) ) ;
#83355 = VECTOR ( 'NONE', #732, 1000.000000000000000 ) ;
#83356 = CARTESIAN_POINT ( 'NONE',  ( 185.8385416670080872, 6.551208109652274736, 3.782341765625001351 ) ) ;
#83357 = DIRECTION ( 'NONE',  ( -1.000000000000000000, -0.000000000000000000, -0.000000000000000000 ) ) ;
#83358 = CARTESIAN_POINT ( 'NONE',  ( 9.599999999999917932, 2.500000000000000000, -0.1000000000000022815 ) ) ;
#83359 = CARTESIAN_POINT ( 'NONE',  ( 9.549999999999915445, 2.500000000000000000, -2.265063509461101798 ) ) ;
#83360 = PLANE ( 'NONE',  #45502 ) ;
#83361 = VERTEX_POINT ( 'NONE', #91158 ) ;
#83362 = CARTESIAN_POINT ( 'NONE',  ( 1.699999999999951994, 2.500000000000000000, -2.276824562219559311E-15 ) ) ;
#83363 = DIRECTION ( 'NONE',  ( -0.000000000000000000, -1.000000000000000000, -0.000000000000000000 ) ) ;
#83364 = CARTESIAN_POINT ( 'NONE',  ( 0.6499999999999543920, 12.50000000000000000, 6.148780366869520897 ) ) ;
#83365 = AXIS2_PLACEMENT_3D ( 'NONE', #56235, #5835, #105992 ) ;
#83366 = ORIENTED_EDGE ( 'NONE', *, *, #101397, .F. ) ;
#83368 = AXIS2_PLACEMENT_3D ( 'NONE', #85972, #63789, #125902 ) ;
#83367 = VECTOR ( 'NONE', #106946, 1000.000000000000000 ) ;
#83369 = CARTESIAN_POINT ( 'NONE',  ( 5.399999999999936406, 2.500000000000000000, -4.922947341949753586 ) ) ;
#83370 = AXIS2_PLACEMENT_3D ( 'NONE', #75303, #115198, #65477 ) ;
#83371 = ORIENTED_EDGE ( 'NONE', *, *, #126116, .F. ) ;
#83372 = CARTESIAN_POINT ( 'NONE',  ( 3.349999999999944578, 12.50000000000000000, -1.407149913249512663 ) ) ;
#83373 = EDGE_LOOP ( 'NONE', ( #53311, #62377 ) ) ;
#83375 = CIRCLE ( 'NONE', #116803, 0.06509327318403745899 ) ;
#83374 = CARTESIAN_POINT ( 'NONE',  ( 9.999999999999914735, 12.50000000000000000, 0.6928203230275494784 ) ) ;
#83376 = CARTESIAN_POINT ( 'NONE',  ( -5.400000000000020783, 2.500000000000000000, 0.6928203230275494784 ) ) ;
#83377 = CARTESIAN_POINT ( 'NONE',  ( -4.800000000000024691, 2.500000000000000000, 4.676537180435972552 ) ) ;
#83378 = ORIENTED_EDGE ( 'NONE', *, *, #86906, .T. ) ;
#83379 = EDGE_CURVE ( 'NONE', #1899, #66996, #59717, .T. ) ;
#83380 = CARTESIAN_POINT ( 'NONE',  ( -2.100000000000033396, 2.500000000000000000, 0.6928203230275494784 ) ) ;
#83382 = CONICAL_SURFACE ( 'NONE', #85519, 0.1000000000000002554, 0.003490658503988666988 ) ;
#83381 = AXIS2_PLACEMENT_3D ( 'NONE', #68839, #79328, #80607 ) ;
#83383 = DIRECTION ( 'NONE',  ( 0.000000000000000000, 0.000000000000000000, -1.000000000000000000 ) ) ;
#83384 = AXIS2_PLACEMENT_3D ( 'NONE', #62650, #24003, #114311 ) ;
#83385 = EDGE_CURVE ( 'NONE', #107774, #84934, #22438, .T. ) ;
#83386 = ADVANCED_FACE ( 'NONE', ( #102271 ), #78672, .T. ) ;
#83387 = VERTEX_POINT ( 'NONE', #110785 ) ;
#83389 = AXIS2_PLACEMENT_3D ( 'NONE', #105245, #27310, #77704 ) ;
#83388 = AXIS2_PLACEMENT_3D ( 'NONE', #74878, #84034, #112872 ) ;
#83390 = ORIENTED_EDGE ( 'NONE', *, *, #2569, .T. ) ;
#83391 = ORIENTED_EDGE ( 'NONE', *, *, #91944, .T. ) ;
#83392 = FACE_OUTER_BOUND ( 'NONE', #80729, .T. ) ;
#83393 = DIRECTION ( 'NONE',  ( -0.000000000000000000, 1.000000000000000000, -0.000000000000000000 ) ) ;
#83394 = ADVANCED_FACE ( 'NONE', ( #70875 ), #116199, .T. ) ;
#83395 = EDGE_CURVE ( 'NONE', #65903, #25992, #43172, .T. ) ;
#83396 = CARTESIAN_POINT ( 'NONE',  ( -7.050000000000016698, 12.50000000000000000, -2.165063509461101710 ) ) ;
#83397 = ADVANCED_FACE ( 'NONE', ( #89856 ), #20080, .T. ) ;
#83398 = ORIENTED_EDGE ( 'NONE', *, *, #47754, .F. ) ;
#83399 = EDGE_CURVE ( 'NONE', #25034, #25981, #10629, .T. ) ;
#83400 = CARTESIAN_POINT ( 'NONE',  ( 10.84999999999990905, 12.50000000000000000, -6.430097255199264339 ) ) ;
#83401 = CARTESIAN_POINT ( 'NONE',  ( 2.299999999999949640, 2.500000000000000000, -4.676537180435977881 ) ) ;
#83402 = ORIENTED_EDGE ( 'NONE', *, *, #94944, .T. ) ;
#83403 = CARTESIAN_POINT ( 'NONE',  ( -5.600000000000020073, 12.50000000000000000, 4.611443907251934426 ) ) ;
#83404 = CARTESIAN_POINT ( 'NONE',  ( 2.500000000000002220, 2.500000000000000000, -8.999999999999998224 ) ) ;
#83405 = CARTESIAN_POINT ( 'NONE',  ( -12.94999999999999218, 12.50000000000000000, -2.165063509461099489 ) ) ;
#83406 = CARTESIAN_POINT ( 'NONE',  ( -3.550000000000031797, 2.500000000000000000, -6.048780366869526581 ) ) ;
#83407 = CIRCLE ( 'NONE', #16476, 0.1000000000000002554 ) ;
#83408 = CARTESIAN_POINT ( 'NONE',  ( 9.149999999999916866, 12.50000000000000000, 5.802370205355744659 ) ) ;
#83409 = EDGE_CURVE ( 'NONE', #121198, #4792, #103708, .T. ) ;
#83410 = DIRECTION ( 'NONE',  ( 0.000000000000000000, 0.000000000000000000, 1.000000000000000000 ) ) ;
#83411 = CARTESIAN_POINT ( 'NONE',  ( -13.94999999999998685, 12.50000000000000000, 1.753560074763288013 ) ) ;
#83412 = AXIS2_PLACEMENT_3D ( 'NONE', #10410, #109916, #68686 ) ;
#83413 = EDGE_LOOP ( 'NONE', ( #47122, #9387 ) ) ;
#83414 = ORIENTED_EDGE ( 'NONE', *, *, #65260, .F. ) ;
#83415 = ORIENTED_EDGE ( 'NONE', *, *, #12751, .F. ) ;
#83416 = VERTEX_POINT ( 'NONE', #53802 ) ;
#83417 = CARTESIAN_POINT ( 'NONE',  ( -11.44999999999999751, 2.500000000000000000, 6.148780366869520897 ) ) ;
#83418 = DIRECTION ( 'NONE',  ( 0.000000000000000000, 0.000000000000000000, -1.000000000000000000 ) ) ;
#83419 = DIRECTION ( 'NONE',  ( -4.274815082592931898E-19, -0.9999939076577903929, -0.003490651415223739937 ) ) ;
#83420 = ORIENTED_EDGE ( 'NONE', *, *, #23427, .T. ) ;
#83421 = FACE_BOUND ( 'NONE', #31270, .T. ) ;
#83422 = PLANE ( 'NONE',  #79301 ) ;
#83423 = DIRECTION ( 'NONE',  ( 0.000000000000000000, 0.000000000000000000, 1.000000000000000000 ) ) ;
#83424 = CIRCLE ( 'NONE', #104340, 0.06509327318403745899 ) ;
#83425 = AXIS2_PLACEMENT_3D ( 'NONE', #120971, #129535, #111808 ) ;
#83426 = DIRECTION ( 'NONE',  ( 0.000000000000000000, 0.000000000000000000, -1.000000000000000000 ) ) ;
#83427 = AXIS2_PLACEMENT_3D ( 'NONE', #107765, #119510, #99251 ) ;
#83428 = DIRECTION ( 'NONE',  ( -0.000000000000000000, 1.000000000000000000, -0.000000000000000000 ) ) ;
#83429 = CARTESIAN_POINT ( 'NONE',  ( 4.999999999999933387, 2.500000000000000000, 5.022947341949748790 ) ) ;
#83430 = DIRECTION ( 'NONE',  ( 0.000000000000000000, 0.000000000000000000, -1.000000000000000000 ) ) ;
#83431 = CARTESIAN_POINT ( 'NONE',  ( -13.09999999999999254, 2.500000000000000000, 0.3464101615137777923 ) ) ;
#83432 = DIRECTION ( 'NONE',  ( 0.000000000000000000, 0.000000000000000000, 1.000000000000000000 ) ) ;
#83433 = EDGE_CURVE ( 'NONE', #128176, #27524, #99595, .T. ) ;
#83434 = CARTESIAN_POINT ( 'NONE',  ( -0.2000000000000399791, 2.500000000000000000, -4.776537180435977525 ) ) ;
#83435 = AXIS2_PLACEMENT_3D ( 'NONE', #24464, #64380, #87870 ) ;
#83436 = DIRECTION ( 'NONE',  ( -4.274815082592931898E-19, -0.9999939076577903929, -0.003490651415223739937 ) ) ;
#83437 = ORIENTED_EDGE ( 'NONE', *, *, #69040, .F. ) ;
#83438 = AXIS2_PLACEMENT_3D ( 'NONE', #101370, #70612, #3169 ) ;
#83439 = VERTEX_POINT ( 'NONE', #115948 ) ;
#83440 = ORIENTED_EDGE ( 'NONE', *, *, #107639, .T. ) ;
#83441 = ORIENTED_EDGE ( 'NONE', *, *, #15100, .T. ) ;
#83442 = ORIENTED_EDGE ( 'NONE', *, *, #76359, .F. ) ;
#83443 = ORIENTED_EDGE ( 'NONE', *, *, #17581, .F. ) ;
#83444 = EDGE_CURVE ( 'NONE', #61373, #41506, #84914, .T. ) ;
#83445 = CARTESIAN_POINT ( 'NONE',  ( -6.050000000000018474, 2.500000000000000000, 6.941600689897073018 ) ) ;
#83446 = EDGE_CURVE ( 'NONE', #29292, #10886, #3347, .T. ) ;
#83447 = EDGE_LOOP ( 'NONE', ( #38035, #4248, #101284, #70555 ) ) ;
#83448 = ORIENTED_EDGE ( 'NONE', *, *, #109740, .T. ) ;
#83449 = EDGE_CURVE ( 'NONE', #93629, #5464, #74455, .T. ) ;
#83450 = AXIS2_PLACEMENT_3D ( 'NONE', #1481, #182, #51260 ) ;
#83451 = EDGE_CURVE ( 'NONE', #42996, #49853, #32711, .T. ) ;
#83452 = CARTESIAN_POINT ( 'NONE',  ( 11.44999999999990514, 2.500000000000000000, -6.148780366869526226 ) ) ;
#83453 = CARTESIAN_POINT ( 'NONE',  ( -9.150000000000011013, 2.500000000000000000, -5.802370205355744659 ) ) ;
#83454 = DIRECTION ( 'NONE',  ( 0.000000000000000000, 0.000000000000000000, 1.000000000000000000 ) ) ;
#83455 = CONICAL_SURFACE ( 'NONE', #60479, 0.1000000000000002554, 0.003490658503988666988 ) ;
#83456 = EDGE_CURVE ( 'NONE', #20308, #30524, #66124, .T. ) ;
#83457 = EDGE_CURVE ( 'NONE', #40017, #13533, #47273, .T. ) ;
#83458 = EDGE_LOOP ( 'NONE', ( #105984, #15466, #52080, #87996 ) ) ;
#83459 = CARTESIAN_POINT ( 'NONE',  ( 11.69999999999990514, 12.50000000000000000, -2.276824562219559311E-15 ) ) ;
#83460 = ADVANCED_FACE ( 'NONE', ( #83899 ), #93242, .T. ) ;
#83461 = EDGE_CURVE ( 'NONE', #64597, #68062, #26433, .T. ) ;
#83462 = ORIENTED_EDGE ( 'NONE', *, *, #86730, .F. ) ;
#83463 = EDGE_CURVE ( 'NONE', #16935, #33066, #84558, .T. ) ;
#83464 = ORIENTED_EDGE ( 'NONE', *, *, #76093, .T. ) ;
#83465 = CARTESIAN_POINT ( 'NONE',  ( -3.150000000000032330, 2.500000000000000000, -6.148780366869526226 ) ) ;
#83466 = FACE_OUTER_BOUND ( 'NONE', #6260, .T. ) ;
#83467 = EDGE_LOOP ( 'NONE', ( #55893, #61383 ) ) ;
#83468 = AXIS2_PLACEMENT_3D ( 'NONE', #127106, #55134, #45326 ) ;
#83469 = ADVANCED_FACE ( 'NONE', ( #23709 ), #1286, .T. ) ;
#83470 = ORIENTED_EDGE ( 'NONE', *, *, #34939, .T. ) ;
#83471 = CARTESIAN_POINT ( 'NONE',  ( 12.89999999999990266, 12.50000000000000000, -4.957854068765716882 ) ) ;
#83472 = AXIS2_PLACEMENT_3D ( 'NONE', #107009, #25897, #76285 ) ;
#83473 = DIRECTION ( 'NONE',  ( 0.000000000000000000, 0.000000000000000000, -1.000000000000000000 ) ) ;
#83474 = LINE ( 'NONE', #23903, #102237 ) ;
#83475 = DIRECTION ( 'NONE',  ( 0.000000000000000000, 1.000000000000000000, 0.000000000000000000 ) ) ;
#83476 = CARTESIAN_POINT ( 'NONE',  ( 3.149999999999942624, 12.50000000000000000, 6.148780366869520897 ) ) ;
#83477 = VECTOR ( 'NONE', #17242, 1000.000000000000000 ) ;
#83478 = ORIENTED_EDGE ( 'NONE', *, *, #17635, .T. ) ;
#83479 = DIRECTION ( 'NONE',  ( 0.000000000000000000, 1.000000000000000000, 0.000000000000000000 ) ) ;
#83480 = ORIENTED_EDGE ( 'NONE', *, *, #96533, .T. ) ;
#83481 = DIRECTION ( 'NONE',  ( 1.000000000000000000, 0.000000000000000000, -0.000000000000000000 ) ) ;
#83482 = AXIS2_PLACEMENT_3D ( 'NONE', #79053, #50234, #20760 ) ;
#83483 = VERTEX_POINT ( 'NONE', #114025 ) ;
#83484 = CARTESIAN_POINT ( 'NONE',  ( -1.650000000000034772, 2.500000000000000000, 2.065063509461097624 ) ) ;
#83485 = DIRECTION ( 'NONE',  ( 0.000000000000000000, 1.000000000000000000, 0.000000000000000000 ) ) ;
#83486 = VECTOR ( 'NONE', #77595, 1000.000000000000000 ) ;
#83487 = CARTESIAN_POINT ( 'NONE',  ( -9.600000000000008527, 2.500000000000000000, -3.737306695894645259 ) ) ;
#83488 = DIRECTION ( 'NONE',  ( 0.000000000000000000, -0.9999939076577903929, 0.003490651415223739937 ) ) ;
#83489 = ORIENTED_EDGE ( 'NONE', *, *, #112991, .F. ) ;
#83490 = SURFACE_STYLE_USAGE ( .BOTH. , #94571 ) ;
#83492 = CIRCLE ( 'NONE', #35364, 0.1000000000000002554 ) ;
#83491 = VECTOR ( 'NONE', #14860, 1000.000000000000000 ) ;
#83493 = DIRECTION ( 'NONE',  ( -0.000000000000000000, -1.000000000000000000, -0.000000000000000000 ) ) ;
#83494 = ORIENTED_EDGE ( 'NONE', *, *, #126956, .T. ) ;
#83495 = EDGE_LOOP ( 'NONE', ( #74381, #17227, #67207, #45628 ) ) ;
#83496 = EDGE_LOOP ( 'NONE', ( #97660, #87152 ) ) ;
#83497 = PLANE ( 'NONE',  #102229 ) ;
#83498 = DIRECTION ( 'NONE',  ( -0.000000000000000000, 1.000000000000000000, -0.000000000000000000 ) ) ;
#83499 = CARTESIAN_POINT ( 'NONE',  ( 185.1093750003413732, 9.264065473108010111E-16, -7.564683531250000925 ) ) ;
#83500 = CARTESIAN_POINT ( 'NONE',  ( -0.8000000000000381251, 2.500000000000000000, 4.330127018922196314 ) ) ;
#83501 = CARTESIAN_POINT ( 'NONE',  ( -8.100000000000013856, 2.500000000000000000, -4.776537180435977525 ) ) ;
#83503 = EDGE_CURVE ( 'NONE', #55444, #121877, #5477, .T. ) ;
#83502 = CARTESIAN_POINT ( 'NONE',  ( 87.50000000000001421, 0.000000000000000000, 0.000000000000000000 ) ) ;
#83504 = FACE_OUTER_BOUND ( 'NONE', #108521, .T. ) ;
#83505 = AXIS2_PLACEMENT_3D ( 'NONE', #127843, #77454, #129165 ) ;
#83506 = VERTEX_POINT ( 'NONE', #24990 ) ;
#83507 = CARTESIAN_POINT ( 'NONE',  ( 9.999999999999911182, 2.500000000000000000, -3.737306695894649700 ) ) ;
#83508 = AXIS2_PLACEMENT_3D ( 'NONE', #42471, #110544, #51002 ) ;
#83509 = VECTOR ( 'NONE', #41171, 1000.000000000000000 ) ;
#83510 = ORIENTED_EDGE ( 'NONE', *, *, #96076, .T. ) ;
#83511 = DIRECTION ( 'NONE',  ( 0.000000000000000000, 1.000000000000000000, 0.000000000000000000 ) ) ;
#83512 = EDGE_CURVE ( 'NONE', #117253, #92392, #120425, .T. ) ;
#83513 = FACE_OUTER_BOUND ( 'NONE', #45360, .T. ) ;
#83514 = DIRECTION ( 'NONE',  ( -1.000000000000000000, -0.000000000000000000, -0.000000000000000000 ) ) ;
#83515 = DIRECTION ( 'NONE',  ( 0.000000000000000000, 0.000000000000000000, -1.000000000000000000 ) ) ;
#83516 = ORIENTED_EDGE ( 'NONE', *, *, #53579, .F. ) ;
#83517 = AXIS2_PLACEMENT_3D ( 'NONE', #14850, #125478, #33872 ) ;
#83518 = AXIS2_PLACEMENT_3D ( 'NONE', #114664, #66205, #74754 ) ;
#83519 = LINE ( 'NONE', #104432, #82709 ) ;
#83521 = VERTEX_POINT ( 'NONE', #103565 ) ;
#83520 = DIRECTION ( 'NONE',  ( -0.000000000000000000, 1.000000000000000000, -0.000000000000000000 ) ) ;
#83522 = CONICAL_SURFACE ( 'NONE', #87702, 0.1000000000000000472, 0.003490658503988666988 ) ;
#83523 = VERTEX_POINT ( 'NONE', #123204 ) ;
#83524 = PLANE ( 'NONE',  #76111 ) ;
#83525 = AXIS2_PLACEMENT_3D ( 'NONE', #43440, #42131, #82039 ) ;
#83526 = VERTEX_POINT ( 'NONE', #63638 ) ;
#83527 = ORIENTED_EDGE ( 'NONE', *, *, #123710, .F. ) ;
#83528 = FACE_OUTER_BOUND ( 'NONE', #93648, .T. ) ;
#83529 = VERTEX_POINT ( 'NONE', #24355 ) ;
#83530 = CARTESIAN_POINT ( 'NONE',  ( 15.44463772192102446, 2.469073678227471813, -4.264595835262737111 ) ) ;
#83531 = CARTESIAN_POINT ( 'NONE',  ( -9.150000000000009237, 2.500000000000000000, -1.472243186433550122 ) ) ;
#83532 = CARTESIAN_POINT ( 'NONE',  ( -6.450000000000016165, 2.500000000000000000, 2.511473670974873507 ) ) ;
#83533 = ORIENTED_EDGE ( 'NONE', *, *, #77912, .F. ) ;
#83534 = EDGE_CURVE ( 'NONE', #118050, #16181, #63988, .T. ) ;
#83535 = LINE ( 'NONE', #33151, #127780 ) ;
#83537 = ORIENTED_EDGE ( 'NONE', *, *, #27847, .T. ) ;
#83536 = CARTESIAN_POINT ( 'NONE',  ( 187.2500000000000000, 9.429780353434619030E-16, -7.700000000000000178 ) ) ;
#83538 = AXIS2_PLACEMENT_3D ( 'NONE', #111435, #83911, #72824 ) ;
#83539 = DIRECTION ( 'NONE',  ( 0.000000000000000000, 0.000000000000000000, 1.000000000000000000 ) ) ;
#83540 = LINE ( 'NONE', #54686, #46771 ) ;
#83541 = ADVANCED_FACE ( 'NONE', ( #64902 ), #104817, .T. ) ;
#83542 = ORIENTED_EDGE ( 'NONE', *, *, #54143, .F. ) ;
#83543 = ORIENTED_EDGE ( 'NONE', *, *, #27421, .T. ) ;
#83544 = ORIENTED_EDGE ( 'NONE', *, *, #46143, .F. ) ;
#83545 = EDGE_LOOP ( 'NONE', ( #22060, #74276, #57730, #118369 ) ) ;
#83546 = FACE_OUTER_BOUND ( 'NONE', #61325, .T. ) ;
#83547 = CARTESIAN_POINT ( 'NONE',  ( 3.709550432166843770, 1.500000000000382583, 10.00000000000000533 ) ) ;
#83548 = EDGE_CURVE ( 'NONE', #84561, #121566, #36810, .T. ) ;
#83549 = ADVANCED_FACE ( 'NONE', ( #75366 ), #68177, .T. ) ;
#83550 = FACE_OUTER_BOUND ( 'NONE', #6414, .T. ) ;
#83551 = EDGE_CURVE ( 'NONE', #80186, #127679, #16433, .T. ) ;
#83552 = FACE_BOUND ( 'NONE', #48981, .T. ) ;
#83554 = EDGE_CURVE ( 'NONE', #4826, #5152, #39351, .T. ) ;
#83553 = EDGE_LOOP ( 'NONE', ( #20085, #34280 ) ) ;
#83555 = CARTESIAN_POINT ( 'NONE',  ( 183.7812500006828031, 0.000000000000000000, 7.700000000000000178 ) ) ;
#83556 = EDGE_CURVE ( 'NONE', #31381, #19741, #76675, .T. ) ;
#83557 = DIRECTION ( 'NONE',  ( 0.000000000000000000, 0.000000000000000000, -1.000000000000000000 ) ) ;
#83558 = DIRECTION ( 'NONE',  ( 0.000000000000000000, -0.9999939076577903929, 0.003490651415223739937 ) ) ;
#83559 = LINE ( 'NONE', #43011, #4642 ) ;
#83560 = LINE ( 'NONE', #101902, #59406 ) ;
#83561 = CIRCLE ( 'NONE', #125407, 0.06509327318403745899 ) ;
#83562 = EDGE_CURVE ( 'NONE', #73190, #7558, #97426, .T. ) ;
#83563 = DIRECTION ( 'NONE',  ( -0.000000000000000000, -1.000000000000000000, -0.000000000000000000 ) ) ;
#83564 = EDGE_CURVE ( 'NONE', #80681, #55060, #61941, .T. ) ;
#83565 = ADVANCED_FACE ( 'NONE', ( #7915 ), #41025, .T. ) ;
#83566 = FACE_OUTER_BOUND ( 'NONE', #68955, .T. ) ;
#83568 = AXIS2_PLACEMENT_3D ( 'NONE', #55376, #86756, #27836 ) ;
#83567 = CIRCLE ( 'NONE', #39758, 0.06509327318403745899 ) ;
#83569 = ORIENTED_EDGE ( 'NONE', *, *, #52943, .T. ) ;
#83570 = ORIENTED_EDGE ( 'NONE', *, *, #51336, .T. ) ;
#83571 = ORIENTED_EDGE ( 'NONE', *, *, #10980, .F. ) ;
#83572 = ORIENTED_EDGE ( 'NONE', *, *, #99262, .F. ) ;
#83573 = EDGE_LOOP ( 'NONE', ( #33625, #118602 ) ) ;
#83574 = DIRECTION ( 'NONE',  ( 0.000000000000000000, 0.000000000000000000, 1.000000000000000000 ) ) ;
#83575 = CIRCLE ( 'NONE', #27132, 0.09999999999999982514 ) ;
#83576 = FACE_OUTER_BOUND ( 'NONE', #126265, .T. ) ;
#83577 = ORIENTED_EDGE ( 'NONE', *, *, #8457, .F. ) ;
#83578 = FACE_BOUND ( 'NONE', #70260, .T. ) ;
#83579 = LINE ( 'NONE', #54732, #123091 ) ;
#83581 = CIRCLE ( 'NONE', #27138, 0.09999999999999982514 ) ;
#83580 = CONICAL_SURFACE ( 'NONE', #4125, 0.1000000000000002554, 0.003490658503988666988 ) ;
#83582 = ORIENTED_EDGE ( 'NONE', *, *, #58484, .F. ) ;
#83583 = DIRECTION ( 'NONE',  ( -1.000000000000000000, -0.000000000000000000, -0.000000000000000000 ) ) ;
#83584 = LINE ( 'NONE', #123482, #99181 ) ;
#83585 = DIRECTION ( 'NONE',  ( 0.000000000000000000, 1.000000000000000000, 0.000000000000000000 ) ) ;
#83586 = ORIENTED_EDGE ( 'NONE', *, *, #109698, .T. ) ;
#83587 = DIRECTION ( 'NONE',  ( -0.000000000000000000, -1.000000000000000000, -0.000000000000000000 ) ) ;
#83588 = EDGE_LOOP ( 'NONE', ( #43529, #124147 ) ) ;
#83589 = ORIENTED_EDGE ( 'NONE', *, *, #85790, .T. ) ;
#83590 = ORIENTED_EDGE ( 'NONE', *, *, #109733, .F. ) ;
#83591 = DIRECTION ( 'NONE',  ( -4.274815082592931898E-19, -0.9999939076577903929, -0.003490651415223739937 ) ) ;
#83592 = CARTESIAN_POINT ( 'NONE',  ( 2.499999999999948930, 2.500000000000000000, -0.6928203230275541413 ) ) ;
#83593 = DIRECTION ( 'NONE',  ( 0.000000000000000000, 1.000000000000000000, 0.000000000000000000 ) ) ;
#83594 = EDGE_LOOP ( 'NONE', ( #106801, #127472, #39845, #14024 ) ) ;
#83595 = DIRECTION ( 'NONE',  ( -0.000000000000000000, -1.000000000000000000, -0.000000000000000000 ) ) ;
#83596 = CARTESIAN_POINT ( 'NONE',  ( 12.04999999999990834, 2.500000000000000000, 6.595190528383296780 ) ) ;
#83597 = CIRCLE ( 'NONE', #123295, 2.000000000000000000 ) ;
#83598 = DIRECTION ( 'NONE',  ( 0.000000000000000000, 0.000000000000000000, -1.000000000000000000 ) ) ;
#83599 = CARTESIAN_POINT ( 'NONE',  ( 186.9479166673494603, -6.668395609140176816, -3.850000000000003642 ) ) ;
#83600 = ORIENTED_EDGE ( 'NONE', *, *, #26484, .F. ) ;
#83601 = CARTESIAN_POINT ( 'NONE',  ( 6.849999999999929479, 2.500000000000000000, 6.941600689897073018 ) ) ;
#83602 = EDGE_CURVE ( 'NONE', #90022, #12489, #24271, .T. ) ;
#83603 = ORIENTED_EDGE ( 'NONE', *, *, #79409, .F. ) ;
#83604 = CARTESIAN_POINT ( 'NONE',  ( -6.450000000000016165, 12.50000000000000000, 6.841600689897072485 ) ) ;
#83605 = VECTOR ( 'NONE', #90357, 1000.000000000000000 ) ;
#83606 = EDGE_CURVE ( 'NONE', #41921, #116415, #79263, .T. ) ;
#83607 = ORIENTED_EDGE ( 'NONE', *, *, #22712, .F. ) ;
#83608 = ADVANCED_FACE ( 'NONE', ( #8548 ), #120517, .T. ) ;
#83609 = ORIENTED_EDGE ( 'NONE', *, *, #90543, .T. ) ;
#83610 = DIRECTION ( 'NONE',  ( 0.000000000000000000, -0.000000000000000000, 1.000000000000000000 ) ) ;
#83611 = CARTESIAN_POINT ( 'NONE',  ( -8.150000000000009237, 2.500000000000000000, 6.148780366869520009 ) ) ;
#83612 = DIRECTION ( 'NONE',  ( -0.000000000000000000, -1.000000000000000000, -0.000000000000000000 ) ) ;
#83613 = DIRECTION ( 'NONE',  ( 0.000000000000000000, 1.000000000000000000, 0.000000000000000000 ) ) ;
#83614 = FACE_OUTER_BOUND ( 'NONE', #11949, .T. ) ;
#83615 = VERTEX_POINT ( 'NONE', #38033 ) ;
#83616 = EDGE_CURVE ( 'NONE', #69443, #55889, #18386, .T. ) ;
#83617 = ORIENTED_EDGE ( 'NONE', *, *, #100222, .T. ) ;
#83618 = CONICAL_SURFACE ( 'NONE', #45967, 0.09999999999999982514, 0.003490658503988666988 ) ;
#83619 = DIRECTION ( 'NONE',  ( 0.000000000000000000, -0.9999939076577903929, 0.003490651415223739937 ) ) ;
#83620 = VECTOR ( 'NONE', #43303, 1000.000000000000000 ) ;
#83621 = CARTESIAN_POINT ( 'NONE',  ( 5.399999999999932854, 2.500000000000000000, 4.922947341949748257 ) ) ;
#83622 = PLANE ( 'NONE',  #52335 ) ;
#83623 = ORIENTED_EDGE ( 'NONE', *, *, #65383, .T. ) ;
#83624 = ORIENTED_EDGE ( 'NONE', *, *, #122540, .F. ) ;
#83625 = VECTOR ( 'NONE', #116578, 1000.000000000000000 ) ;
#83626 = DIRECTION ( 'NONE',  ( 0.000000000000000000, 0.000000000000000000, -1.000000000000000000 ) ) ;
#83627 = AXIS2_PLACEMENT_3D ( 'NONE', #26036, #5725, #106517 ) ;
#83628 = ORIENTED_EDGE ( 'NONE', *, *, #14658, .T. ) ;
#83629 = CARTESIAN_POINT ( 'NONE',  ( 5.649999999999934630, 2.500000000000000000, -2.611473670974877592 ) ) ;
#83630 = FACE_OUTER_BOUND ( 'NONE', #55710, .T. ) ;
#83631 = VERTEX_POINT ( 'NONE', #47868 ) ;
#83632 = DIRECTION ( 'NONE',  ( -0.000000000000000000, -1.000000000000000000, -0.000000000000000000 ) ) ;
#83633 = FACE_OUTER_BOUND ( 'NONE', #52802, .T. ) ;
#83634 = VECTOR ( 'NONE', #127654, 1000.000000000000000 ) ;
#83635 = PLANE ( 'NONE',  #65582 ) ;
#83636 = ADVANCED_FACE ( 'NONE', ( #117205 ), #118518, .F. ) ;
#83637 = DIRECTION ( 'NONE',  ( 0.000000000000000000, 0.000000000000000000, -1.000000000000000000 ) ) ;
#83638 = ORIENTED_EDGE ( 'NONE', *, *, #128667, .F. ) ;
#83639 = CARTESIAN_POINT ( 'NONE',  ( 2.699999999999946443, 12.50000000000000000, 0.3464101615137735735 ) ) ;
#83640 = CARTESIAN_POINT ( 'NONE',  ( 10.19999999999991225, 2.500000000000000000, -4.576537180435978236 ) ) ;
#83641 = ORIENTED_EDGE ( 'NONE', *, *, #89636, .T. ) ;
#83642 = VERTEX_POINT ( 'NONE', #98234 ) ;
#83643 = CARTESIAN_POINT ( 'NONE',  ( 186.1302083336747444, -4.367472073101514418, -7.564683531250002702 ) ) ;
#83644 = CARTESIAN_POINT ( 'NONE',  ( -6.650000000000014566, 2.500000000000000000, 6.595190528383296780 ) ) ;
#83645 = DIRECTION ( 'NONE',  ( -0.000000000000000000, 1.000000000000000000, -0.000000000000000000 ) ) ;
#83646 = CARTESIAN_POINT ( 'NONE',  ( 13.74999999999989519, 12.50000000000000000, -2.857883832488653741 ) ) ;
#83647 = DIRECTION ( 'NONE',  ( 0.000000000000000000, -0.9999939076577903929, 0.003490651415223739937 ) ) ;
#83648 = CARTESIAN_POINT ( 'NONE',  ( -9.150000000000009237, 2.500000000000000000, -6.395190528383296602 ) ) ;
#83650 = EDGE_CURVE ( 'NONE', #68081, #3295, #87761, .T. ) ;
#83649 = CARTESIAN_POINT ( 'NONE',  ( -7.500000000000001776, 1.500000000000000000, 1.734723475976807094E-15 ) ) ;
#83651 = CARTESIAN_POINT ( 'NONE',  ( -4.400000000000025224, 2.500000000000000000, 3.983716857408420076 ) ) ;
#83652 = CARTESIAN_POINT ( 'NONE',  ( -7.499999999999980460, 12.50000000000000000, -2.276824562219559311E-15 ) ) ;
#83653 = LINE ( 'NONE', #60321, #115184 ) ;
#83654 = CIRCLE ( 'NONE', #75230, 0.06509327318403745899 ) ;
#83655 = DIRECTION ( 'NONE',  ( 0.000000000000000000, 0.000000000000000000, 1.000000000000000000 ) ) ;
#83656 = ORIENTED_EDGE ( 'NONE', *, *, #7492, .T. ) ;
#83657 = ORIENTED_EDGE ( 'NONE', *, *, #75288, .F. ) ;
#83658 = AXIS2_PLACEMENT_3D ( 'NONE', #128655, #38990, #118798 ) ;
#83659 = EDGE_LOOP ( 'NONE', ( #14982, #91184 ) ) ;
#83660 = EDGE_LOOP ( 'NONE', ( #4527, #16328, #70045, #34933 ) ) ;
#83661 = ADVANCED_FACE ( 'NONE', ( #88404 ), #36763, .T. ) ;
#83662 = FACE_OUTER_BOUND ( 'NONE', #83734, .T. ) ;
#83663 = LINE ( 'NONE', #127295, #129424 ) ;
#83665 = ORIENTED_EDGE ( 'NONE', *, *, #3150, .T. ) ;
#83664 = CIRCLE ( 'NONE', #14590, 0.06509327318403745899 ) ;
#83666 = DIRECTION ( 'NONE',  ( 0.000000000000000000, 1.000000000000000000, 0.000000000000000000 ) ) ;
#83667 = DIRECTION ( 'NONE',  ( 0.000000000000000000, 0.000000000000000000, 1.000000000000000000 ) ) ;
#83669 = ORIENTED_EDGE ( 'NONE', *, *, #322, .T. ) ;
#83668 = CARTESIAN_POINT ( 'NONE',  ( -11.84999999999999609, 12.50000000000000000, 1.818653347947321475 ) ) ;
#83670 = DIRECTION ( 'NONE',  ( 0.000000000000000000, 1.000000000000000000, 0.000000000000000000 ) ) ;
#83671 = FACE_OUTER_BOUND ( 'NONE', #87933, .T. ) ;
#83672 = ORIENTED_EDGE ( 'NONE', *, *, #100227, .T. ) ;
#83673 = ORIENTED_EDGE ( 'NONE', *, *, #11145, .F. ) ;
#83674 = VERTEX_POINT ( 'NONE', #9218 ) ;
#83675 = ORIENTED_EDGE ( 'NONE', *, *, #101872, .T. ) ;
#83676 = DIRECTION ( 'NONE',  ( -0.000000000000000000, 1.000000000000000000, -0.000000000000000000 ) ) ;
#83677 = CARTESIAN_POINT ( 'NONE',  ( -15.19999999999998153, 2.500000000000000000, -0.3464101615137759604 ) ) ;
#83678 = CARTESIAN_POINT ( 'NONE',  ( 4.199999999999941558, 2.500000000000000000, -4.330127018922201643 ) ) ;
#83679 = DIRECTION ( 'NONE',  ( 0.000000000000000000, 0.000000000000000000, 1.000000000000000000 ) ) ;
#83680 = CIRCLE ( 'NONE', #14695, 0.06509327318403743123 ) ;
#83681 = ORIENTED_EDGE ( 'NONE', *, *, #96396, .T. ) ;
#83682 = AXIS2_PLACEMENT_3D ( 'NONE', #59127, #119312, #47367 ) ;
#83683 = EDGE_CURVE ( 'NONE', #41491, #118121, #28871, .T. ) ;
#83684 = DIRECTION ( 'NONE',  ( 0.000000000000000000, -0.9999939076577903929, 0.003490651415223739937 ) ) ;
#83685 = VERTEX_POINT ( 'NONE', #108703 ) ;
#83686 = DIRECTION ( 'NONE',  ( 0.000000000000000000, 0.000000000000000000, 1.000000000000000000 ) ) ;
#83687 = DIRECTION ( 'NONE',  ( -0.9961946980917455452, 0.000000000000000000, -0.08715574274765836016 ) ) ;
#83688 = CARTESIAN_POINT ( 'NONE',  ( -6.050000000000020250, 2.500000000000000000, -6.741600689897078169 ) ) ;
#83689 = DIRECTION ( 'NONE',  ( 0.000000000000000000, -0.9999939076577903929, 0.003490651415223739937 ) ) ;
#83690 = ADVANCED_FACE ( 'NONE', ( #19019 ), #49166, .T. ) ;
#83691 = VECTOR ( 'NONE', #52292, 1000.000000000000000 ) ;
#83692 = EDGE_CURVE ( 'NONE', #106597, #18843, #27545, .T. ) ;
#83693 = ORIENTED_EDGE ( 'NONE', *, *, #126096, .T. ) ;
#83694 = EDGE_LOOP ( 'NONE', ( #28894, #104447, #33503, #87723 ) ) ;
#83695 = ORIENTED_EDGE ( 'NONE', *, *, #38304, .F. ) ;
#83696 = DIRECTION ( 'NONE',  ( -0.000000000000000000, -1.000000000000000000, -0.000000000000000000 ) ) ;
#83697 = DIRECTION ( 'NONE',  ( 0.000000000000000000, -0.9999939076577903929, 0.003490651415223739937 ) ) ;
#83698 = ADVANCED_FACE ( 'NONE', ( #26928 ), #67462, .T. ) ;
#83699 = EDGE_CURVE ( 'NONE', #122964, #43427, #43263, .T. ) ;
#83700 = DIRECTION ( 'NONE',  ( 0.000000000000000000, 0.000000000000000000, 1.000000000000000000 ) ) ;
#83701 = ADVANCED_FACE ( 'NONE', ( #111933 ), #82960, .T. ) ;
#83702 = FACE_BOUND ( 'NONE', #103015, .T. ) ;
#83703 = ADVANCED_FACE ( 'NONE', ( #41913 ), #52363, .T. ) ;
#83704 = DIRECTION ( 'NONE',  ( 0.000000000000000000, 1.000000000000000000, 0.000000000000000000 ) ) ;
#83705 = CARTESIAN_POINT ( 'NONE',  ( -8.950000000000006395, 2.500000000000000000, 6.741600689897071952 ) ) ;
#83706 = DIRECTION ( 'NONE',  ( -0.000000000000000000, 1.000000000000000000, -0.000000000000000000 ) ) ;
#83707 = AXIS2_PLACEMENT_3D ( 'NONE', #59043, #30244, #110701 ) ;
#83708 = AXIS2_PLACEMENT_3D ( 'NONE', #86904, #7693, #109779 ) ;
#83709 = EDGE_CURVE ( 'NONE', #110285, #24530, #124715, .T. ) ;
#83710 = CARTESIAN_POINT ( 'NONE',  ( 1.049999999999953637, 2.500000000000000000, -1.818653347947326138 ) ) ;
#83711 = EDGE_CURVE ( 'NONE', #52810, #8036, #93328, .T. ) ;
#83712 = DIRECTION ( 'NONE',  ( 0.000000000000000000, 1.000000000000000000, 0.000000000000000000 ) ) ;
#83713 = EDGE_CURVE ( 'NONE', #85857, #53445, #87049, .T. ) ;
#83714 = CARTESIAN_POINT ( 'NONE',  ( 0.3999999999999628852, 2.500000000000000000, 0.7928203230275517877 ) ) ;
#83715 = VERTEX_POINT ( 'NONE', #102112 ) ;
#83716 = CIRCLE ( 'NONE', #39813, 0.1000000000000002554 ) ;
#83717 = ADVANCED_FACE ( 'NONE', ( #100181 ), #57826, .T. ) ;
#83718 = EDGE_CURVE ( 'NONE', #58034, #110840, #114248, .T. ) ;
#83719 = CARTESIAN_POINT ( 'NONE',  ( -2.100000000000034728, 2.500000000000000000, 4.330127018922196314 ) ) ;
#83720 = VERTEX_POINT ( 'NONE', #82483 ) ;
#83721 = ORIENTED_EDGE ( 'NONE', *, *, #95137, .T. ) ;
#83722 = ORIENTED_EDGE ( 'NONE', *, *, #3445, .F. ) ;
#83723 = ORIENTED_EDGE ( 'NONE', *, *, #80873, .F. ) ;
#83724 = PLANE ( 'NONE',  #8932 ) ;
#83725 = FACE_BOUND ( 'NONE', #31489, .T. ) ;
#83726 = EDGE_CURVE ( 'NONE', #104677, #62516, #41114, .T. ) ;
#83727 = DIRECTION ( 'NONE',  ( -0.000000000000000000, 1.000000000000000000, -0.000000000000000000 ) ) ;
#83728 = ORIENTED_EDGE ( 'NONE', *, *, #115750, .F. ) ;
#83729 = CARTESIAN_POINT ( 'NONE',  ( -11.44999999999999751, 2.500000000000000000, 2.411473670974873862 ) ) ;
#83730 = CARTESIAN_POINT ( 'NONE',  ( 165.4999999999999716, 0.000000000000000000, 1.500000000000000000 ) ) ;
#83731 = ORIENTED_EDGE ( 'NONE', *, *, #93940, .T. ) ;
#83732 = LINE ( 'NONE', #95477, #40683 ) ;
#83733 = FACE_OUTER_BOUND ( 'NONE', #119985, .T. ) ;
#83734 = EDGE_LOOP ( 'NONE', ( #12411, #39307, #10530, #117329 ) ) ;
#83735 = LINE ( 'NONE', #85660, #36058 ) ;
#83736 = CONICAL_SURFACE ( 'NONE', #27289, 0.1000000000000000472, 0.003490658503988666988 ) ;
#83737 = FACE_OUTER_BOUND ( 'NONE', #55367, .T. ) ;
#83738 = EDGE_LOOP ( 'NONE', ( #13036, #78649 ) ) ;
#83739 = DIRECTION ( 'NONE',  ( 0.000000000000000000, 0.000000000000000000, -1.000000000000000000 ) ) ;
#83740 = CONICAL_SURFACE ( 'NONE', #2242, 0.1000000000000002554, 0.003490658503988666988 ) ;
#83741 = CARTESIAN_POINT ( 'NONE',  ( 4.349999999999940137, 2.500000000000000000, -2.411473670974877859 ) ) ;
#83742 = DIRECTION ( 'NONE',  ( 0.000000000000000000, 1.000000000000000000, 0.000000000000000000 ) ) ;
#83743 = ORIENTED_EDGE ( 'NONE', *, *, #20603, .T. ) ;
#83744 = ORIENTED_EDGE ( 'NONE', *, *, #28582, .T. ) ;
#83745 = DIRECTION ( 'NONE',  ( 0.000000000000000000, -0.000000000000000000, 1.000000000000000000 ) ) ;
#83746 = ORIENTED_EDGE ( 'NONE', *, *, #46811, .T. ) ;
#83747 = FACE_OUTER_BOUND ( 'NONE', #122836, .T. ) ;
#83748 = CARTESIAN_POINT ( 'NONE',  ( 0.1999999999999636513, 12.50000000000000000, -0.3464101615137760715 ) ) ;
#83749 = EDGE_CURVE ( 'NONE', #38510, #24704, #118447, .T. ) ;
#83750 = ORIENTED_EDGE ( 'NONE', *, *, #40412, .T. ) ;
#83752 = EDGE_CURVE ( 'NONE', #90411, #63793, #74542, .T. ) ;
#83751 = FACE_OUTER_BOUND ( 'NONE', #6316, .T. ) ;
#83753 = DIRECTION ( 'NONE',  ( 0.000000000000000000, 0.000000000000000000, -1.000000000000000000 ) ) ;
#83754 = FACE_OUTER_BOUND ( 'NONE', #1944, .T. ) ;
#83755 = DIRECTION ( 'NONE',  ( -0.000000000000000000, 1.000000000000000000, -0.000000000000000000 ) ) ;
#83756 = CARTESIAN_POINT ( 'NONE',  ( 1.649999999999951505, 2.500000000000000000, 1.372243186433545370 ) ) ;
#83757 = ADVANCED_FACE ( 'NONE', ( #49805 ), #47360, .T. ) ;
#83758 = ORIENTED_EDGE ( 'NONE', *, *, #78213, .F. ) ;
#83759 = EDGE_LOOP ( 'NONE', ( #72864, #109227 ) ) ;
#83760 = CARTESIAN_POINT ( 'NONE',  ( 1.249999999999950262, 2.500000000000000000, 7.188010851410848723 ) ) ;
#83761 = CARTESIAN_POINT ( 'NONE',  ( 9.999999999999912959, 12.50000000000000000, -5.022947341949754119 ) ) ;
#83763 = EDGE_LOOP ( 'NONE', ( #112478, #86797, #128713, #20845 ) ) ;
#83762 = ORIENTED_EDGE ( 'NONE', *, *, #20561, .F. ) ;
#83764 = EDGE_LOOP ( 'NONE', ( #12522, #108016 ) ) ;
#83765 = CARTESIAN_POINT ( 'NONE',  ( 7.899999999999924860, 2.500000000000000000, -4.330127018922201643 ) ) ;
#83766 = CIRCLE ( 'NONE', #73294, 8.699999999999999289 ) ;
#83767 = LINE ( 'NONE', #62842, #38139 ) ;
#83768 = CIRCLE ( 'NONE', #60789, 0.5000000000000000000 ) ;
#83769 = CARTESIAN_POINT ( 'NONE',  ( 187.3203125005121024, 0.000000000000000000, 7.632341765625000107 ) ) ;
#83770 = DIRECTION ( 'NONE',  ( 0.000000000000000000, 0.000000000000000000, 1.000000000000000000 ) ) ;
#83771 = DIRECTION ( 'NONE',  ( 0.000000000000000000, 0.000000000000000000, -1.000000000000000000 ) ) ;
#83772 = DIRECTION ( 'NONE',  ( -0.000000000000000000, -1.000000000000000000, -0.000000000000000000 ) ) ;
#83773 = FACE_OUTER_BOUND ( 'NONE', #19027, .T. ) ;
#83774 = CARTESIAN_POINT ( 'NONE',  ( 6.849999999999929479, 2.500000000000000000, 6.048780366869520364 ) ) ;
#83775 = CARTESIAN_POINT ( 'NONE',  ( -11.89999999999999680, 2.500000000000000000, -0.4464101615137742174 ) ) ;
#83776 = DIRECTION ( 'NONE',  ( 0.000000000000000000, 1.000000000000000000, 0.000000000000000000 ) ) ;
#83777 = ORIENTED_EDGE ( 'NONE', *, *, #59324, .F. ) ;
#83778 = DIRECTION ( 'NONE',  ( 0.000000000000000000, 0.000000000000000000, 1.000000000000000000 ) ) ;
#83779 = VERTEX_POINT ( 'NONE', #39976 ) ;
#83780 = EDGE_LOOP ( 'NONE', ( #80071, #64984, #66430, #19495 ) ) ;
#83781 = DIRECTION ( 'NONE',  ( 0.000000000000000000, 0.000000000000000000, 1.000000000000000000 ) ) ;
#83782 = FACE_OUTER_BOUND ( 'NONE', #27859, .T. ) ;
#83783 = PLANE ( 'NONE',  #100904 ) ;
#83785 = EDGE_CURVE ( 'NONE', #127462, #82307, #84995, .T. ) ;
#83784 = CIRCLE ( 'NONE', #117206, 0.1000000000000002554 ) ;
#83786 = DIRECTION ( 'NONE',  ( -0.000000000000000000, 1.000000000000000000, -0.000000000000000000 ) ) ;
#83787 = AXIS2_PLACEMENT_3D ( 'NONE', #125396, #25906, #63898 ) ;
#83788 = DIRECTION ( 'NONE',  ( -0.000000000000000000, -1.000000000000000000, -0.000000000000000000 ) ) ;
#83789 = CARTESIAN_POINT ( 'NONE',  ( 10.39999999999991154, 12.50000000000000000, -5.088040615133791356 ) ) ;
#83790 = DIRECTION ( 'NONE',  ( 0.000000000000000000, 0.000000000000000000, 1.000000000000000000 ) ) ;
#83791 = EDGE_LOOP ( 'NONE', ( #78372, #52406, #85651, #39864 ) ) ;
#83792 = CARTESIAN_POINT ( 'NONE',  ( -8.750000000000008882, 2.500000000000000000, 1.472243186433545459 ) ) ;
#83793 = DIRECTION ( 'NONE',  ( 0.000000000000000000, -0.9999939076577903929, 0.003490651415223739937 ) ) ;
#83794 = VERTEX_POINT ( 'NONE', #79888 ) ;
#83795 = ORIENTED_EDGE ( 'NONE', *, *, #86145, .F. ) ;
#83796 = AXIS2_PLACEMENT_3D ( 'NONE', #36243, #14631, #65681 ) ;
#83797 = EDGE_LOOP ( 'NONE', ( #20848, #75148, #84625, #75153 ) ) ;
#83798 = ADVANCED_FACE ( 'NONE', ( #20968 ), #71341, .T. ) ;
#83800 = VERTEX_POINT ( 'NONE', #80547 ) ;
#83799 = EDGE_CURVE ( 'NONE', #96482, #124893, #64079, .T. ) ;
#83801 = DIRECTION ( 'NONE',  ( 0.000000000000000000, 1.000000000000000000, 0.000000000000000000 ) ) ;
#83802 = CARTESIAN_POINT ( 'NONE',  ( 9.799999999999918998, 12.50000000000000000, -0.3464101615137782364 ) ) ;
#83803 = CARTESIAN_POINT ( 'NONE',  ( -15.39999999999998082, 2.500000000000000000, 0.6928203230275518099 ) ) ;
#83804 = DIRECTION ( 'NONE',  ( 0.000000000000000000, 0.000000000000000000, -1.000000000000000000 ) ) ;
#83805 = LINE ( 'NONE', #54991, #34607 ) ;
#83806 = EDGE_LOOP ( 'NONE', ( #43778, #102982, #59186, #126784 ) ) ;
#83807 = CARTESIAN_POINT ( 'NONE',  ( -13.54999999999999005, 2.500000000000000000, -1.818653347947323917 ) ) ;
#83808 = EDGE_CURVE ( 'NONE', #72985, #37773, #7630, .T. ) ;
#83809 = DIRECTION ( 'NONE',  ( 0.000000000000000000, 0.000000000000000000, 1.000000000000000000 ) ) ;
#83810 = CARTESIAN_POINT ( 'NONE',  ( -3.150000000000030553, 2.500000000000000000, 6.248780366869520542 ) ) ;
#83811 = CARTESIAN_POINT ( 'NONE',  ( -8.749999999999976907, 12.50000000000000000, -6.495190528383297135 ) ) ;
#83812 = ORIENTED_EDGE ( 'NONE', *, *, #94784, .T. ) ;
#83813 = ORIENTED_EDGE ( 'NONE', *, *, #94601, .T. ) ;
#83814 = VERTEX_POINT ( 'NONE', #101470 ) ;
#83815 = CIRCLE ( 'NONE', #125570, 0.06509327318403745899 ) ;
#83816 = CARTESIAN_POINT ( 'NONE',  ( 194.5000000000000000, 4.898587196589412829E-16, 4.000000000000000000 ) ) ;
#83817 = CONICAL_SURFACE ( 'NONE', #85864, 0.1000000000000000056, 0.003490658503988666988 ) ;
#83818 = FACE_OUTER_BOUND ( 'NONE', #45301, .T. ) ;
#83819 = DIRECTION ( 'NONE',  ( -0.000000000000000000, -1.000000000000000000, -0.000000000000000000 ) ) ;
#83820 = AXIS2_PLACEMENT_3D ( 'NONE', #125043, #15723, #35385 ) ;
#83821 = EDGE_LOOP ( 'NONE', ( #54976, #89590 ) ) ;
#83822 = CARTESIAN_POINT ( 'NONE',  ( 10.39999999999990976, 12.50000000000000000, 4.395220292106234439 ) ) ;
#83823 = CARTESIAN_POINT ( 'NONE',  ( 12.94999999999989981, 2.500000000000000000, -2.165063509461101710 ) ) ;
#83824 = DIRECTION ( 'NONE',  ( 0.000000000000000000, 1.000000000000000000, 0.000000000000000000 ) ) ;
#83825 = DIRECTION ( 'NONE',  ( 0.000000000000000000, -0.9999939076577903929, 0.003490651415223739937 ) ) ;
#83826 = EDGE_CURVE ( 'NONE', #49661, #61872, #60890, .T. ) ;
#83827 = DIRECTION ( 'NONE',  ( 0.000000000000000000, 1.000000000000000000, 0.000000000000000000 ) ) ;
#83828 = ORIENTED_EDGE ( 'NONE', *, *, #30551, .T. ) ;
#83829 = ORIENTED_EDGE ( 'NONE', *, *, #103952, .T. ) ;
#83830 = ADVANCED_FACE ( 'NONE', ( #124331 ), #64752, .T. ) ;
#83831 = CARTESIAN_POINT ( 'NONE',  ( 15.83209681635555022, -2.500000000000000000, -5.404881881984138658 ) ) ;
#83832 = CARTESIAN_POINT ( 'NONE',  ( -6.450000000000016165, 2.500000000000000000, 2.511473670974873507 ) ) ;
#83833 = EDGE_CURVE ( 'NONE', #73941, #61976, #54929, .T. ) ;
#83834 = CARTESIAN_POINT ( 'NONE',  ( -4.150000000000027889, 2.500000000000000000, -7.188010851410854052 ) ) ;
#83835 = DIRECTION ( 'NONE',  ( -0.000000000000000000, -1.000000000000000000, -0.000000000000000000 ) ) ;
#83836 = DIRECTION ( 'NONE',  ( 1.000000000000000000, -0.000000000000000000, -0.000000000000000000 ) ) ;
#83837 = EDGE_LOOP ( 'NONE', ( #94717, #21298 ) ) ;
#83838 = EDGE_CURVE ( 'NONE', #106872, #72837, #4515, .T. ) ;
#83839 = EDGE_CURVE ( 'NONE', #36746, #126920, #93581, .T. ) ;
#83840 = ORIENTED_EDGE ( 'NONE', *, *, #64835, .T. ) ;
#83841 = FACE_OUTER_BOUND ( 'NONE', #106436, .T. ) ;
#83842 = DIRECTION ( 'NONE',  ( 0.000000000000000000, -0.000000000000000000, 1.000000000000000000 ) ) ;
#83843 = EDGE_CURVE ( 'NONE', #107104, #52720, #13053, .T. ) ;
#83844 = DIRECTION ( 'NONE',  ( 0.000000000000000000, -0.000000000000000000, 1.000000000000000000 ) ) ;
#83845 = CARTESIAN_POINT ( 'NONE',  ( 4.149999999999939959, 12.50000000000000000, 2.792790559304612064 ) ) ;
#83846 = ORIENTED_EDGE ( 'NONE', *, *, #24456, .T. ) ;
#83847 = AXIS2_PLACEMENT_3D ( 'NONE', #4567, #44522, #124386 ) ;
#83848 = DIRECTION ( 'NONE',  ( 0.000000000000000000, 1.000000000000000000, 0.000000000000000000 ) ) ;
#83849 = AXIS2_PLACEMENT_3D ( 'NONE', #49513, #51449, #90049 ) ;
#83850 = EDGE_CURVE ( 'NONE', #40065, #26773, #116386, .T. ) ;
#83851 = LINE ( 'NONE', #123147, #114187 ) ;
#83852 = ORIENTED_EDGE ( 'NONE', *, *, #115771, .F. ) ;
#83853 = CARTESIAN_POINT ( 'NONE',  ( 10.19999999999991047, 2.500000000000000000, 4.576537180435972019 ) ) ;
#83854 = VERTEX_POINT ( 'NONE', #103402 ) ;
#83856 = EDGE_CURVE ( 'NONE', #55517, #18996, #20162, .T. ) ;
#83855 = VECTOR ( 'NONE', #2160, 1000.000000000000000 ) ;
#83857 = CARTESIAN_POINT ( 'NONE',  ( -14.14999999999998792, 12.50000000000000000, -1.472243186433547901 ) ) ;
#83858 = VECTOR ( 'NONE', #38071, 1000.000000000000000 ) ;
#83859 = ORIENTED_EDGE ( 'NONE', *, *, #7505, .T. ) ;
#83860 = DIRECTION ( 'NONE',  ( 0.000000000000000000, 1.000000000000000000, 0.000000000000000000 ) ) ;
#83861 = CARTESIAN_POINT ( 'NONE',  ( 12.09999999999990195, 2.500000000000000000, -2.276824562219559311E-15 ) ) ;
#83862 = ORIENTED_EDGE ( 'NONE', *, *, #107375, .F. ) ;
#83863 = ORIENTED_EDGE ( 'NONE', *, *, #110405, .F. ) ;
#83864 = CARTESIAN_POINT ( 'NONE',  ( 186.5468750003414300, -8.734944146203032389, -1.604583208406768146E-15 ) ) ;
#83865 = PLANE ( 'NONE',  #106267 ) ;
#83867 = CARTESIAN_POINT ( 'NONE',  ( 186.9635416670080303, -4.367472073101520635, 7.564683531249999149 ) ) ;
#83866 = VECTOR ( 'NONE', #98627, 1000.000000000000000 ) ;
#83868 = CARTESIAN_POINT ( 'NONE',  ( 185.7760416670080588, 6.551208109652274736, 3.782341765625001351 ) ) ;
#83869 = CIRCLE ( 'NONE', #119377, 0.1000000000000002554 ) ;
#83870 = DIRECTION ( 'NONE',  ( 0.000000000000000000, 0.000000000000000000, 1.000000000000000000 ) ) ;
#83871 = DIRECTION ( 'NONE',  ( 0.000000000000000000, 0.000000000000000000, 1.000000000000000000 ) ) ;
#83872 = PLANE ( 'NONE',  #114295 ) ;
#83873 = LINE ( 'NONE', #5311, #84069 ) ;
#83874 = VERTEX_POINT ( 'NONE', #104666 ) ;
#83875 = VERTEX_POINT ( 'NONE', #14353 ) ;
#83876 = CARTESIAN_POINT ( 'NONE',  ( 12.29999999999990301, 2.500000000000000000, -0.3464101615137782364 ) ) ;
#83877 = VERTEX_POINT ( 'NONE', #92944 ) ;
#83878 = CIRCLE ( 'NONE', #125724, 0.06509327318403745899 ) ;
#83879 = AXIS2_PLACEMENT_3D ( 'NONE', #14218, #54170, #37111 ) ;
#83880 = DIRECTION ( 'NONE',  ( 0.000000000000000000, 0.000000000000000000, -1.000000000000000000 ) ) ;
#83881 = CARTESIAN_POINT ( 'NONE',  ( -8.350000000000013856, 12.50000000000000000, 2.230156782645134950 ) ) ;
#83882 = CARTESIAN_POINT ( 'NONE',  ( 4.349999999999938360, 12.50000000000000000, 1.818653347947321475 ) ) ;
#83884 = ORIENTED_EDGE ( 'NONE', *, *, #68461, .T. ) ;
#83883 = ORIENTED_EDGE ( 'NONE', *, *, #78984, .T. ) ;
#83885 = FACE_BOUND ( 'NONE', #19530, .T. ) ;
#83886 = VERTEX_POINT ( 'NONE', #3266 ) ;
#83887 = CARTESIAN_POINT ( 'NONE',  ( 14.79999999999989413, 12.50000000000000000, -0.3464101615137782364 ) ) ;
#83888 = DIRECTION ( 'NONE',  ( -0.000000000000000000, -1.000000000000000000, -0.000000000000000000 ) ) ;
#83889 = ORIENTED_EDGE ( 'NONE', *, *, #33540, .T. ) ;
#83890 = CARTESIAN_POINT ( 'NONE',  ( 8.349999999999923261, 12.50000000000000000, 1.472243186433545459 ) ) ;
#83891 = DIRECTION ( 'NONE',  ( 0.000000000000000000, 1.000000000000000000, 0.000000000000000000 ) ) ;
#83892 = EDGE_CURVE ( 'NONE', #54782, #109687, #22913, .T. ) ;
#83893 = CARTESIAN_POINT ( 'NONE',  ( -5.200000000000024158, 2.500000000000000000, -4.676537180435977881 ) ) ;
#83894 = DIRECTION ( 'NONE',  ( 0.000000000000000000, 1.000000000000000000, 0.000000000000000000 ) ) ;
#83895 = CARTESIAN_POINT ( 'NONE',  ( -12.04999999999999716, 2.500000000000000000, -6.495190528383298911 ) ) ;
#83896 = FACE_OUTER_BOUND ( 'NONE', #121103, .T. ) ;
#83897 = CARTESIAN_POINT ( 'NONE',  ( 187.2760416670080588, 6.551208109652274736, 3.782341765625001351 ) ) ;
#83898 = FACE_OUTER_BOUND ( 'NONE', #27068, .T. ) ;
#83899 = FACE_OUTER_BOUND ( 'NONE', #22463, .T. ) ;
#83900 = EDGE_CURVE ( 'NONE', #53205, #53076, #105936, .T. ) ;
#83901 = EDGE_LOOP ( 'NONE', ( #33139, #87545, #65899, #87384 ) ) ;
#83902 = ORIENTED_EDGE ( 'NONE', *, *, #49453, .F. ) ;
#83903 = ORIENTED_EDGE ( 'NONE', *, *, #46181, .T. ) ;
#83904 = DIRECTION ( 'NONE',  ( -0.000000000000000000, 1.000000000000000000, -0.000000000000000000 ) ) ;
#83905 = ORIENTED_EDGE ( 'NONE', *, *, #17314, .T. ) ;
#83906 = AXIS2_PLACEMENT_3D ( 'NONE', #106805, #59010, #117252 ) ;
#83907 = AXIS2_PLACEMENT_3D ( 'NONE', #18585, #98413, #67016 ) ;
#83909 = ORIENTED_EDGE ( 'NONE', *, *, #91763, .F. ) ;
#83908 = ORIENTED_EDGE ( 'NONE', *, *, #110867, .F. ) ;
#83910 = ORIENTED_EDGE ( 'NONE', *, *, #101432, .T. ) ;
#83911 = DIRECTION ( 'NONE',  ( 0.000000000000000000, 1.000000000000000000, 0.000000000000000000 ) ) ;
#83912 = CIRCLE ( 'NONE', #44202, 0.06509327318403745899 ) ;
#83913 = LINE ( 'NONE', #94379, #57289 ) ;
#83914 = AXIS2_PLACEMENT_3D ( 'NONE', #109015, #17408, #76996 ) ;
#83915 = CARTESIAN_POINT ( 'NONE',  ( 6.449999999999931788, 12.50000000000000000, -2.511473670974877948 ) ) ;
#83916 = DIRECTION ( 'NONE',  ( 0.000000000000000000, 1.000000000000000000, 0.000000000000000000 ) ) ;
#83917 = VECTOR ( 'NONE', #114200, 1000.000000000000000 ) ;
#83918 = CARTESIAN_POINT ( 'NONE',  ( 2.949999999999946887, 2.500000000000000000, -2.065063509461102065 ) ) ;
#83919 = ORIENTED_EDGE ( 'NONE', *, *, #85901, .T. ) ;
#83920 = DIRECTION ( 'NONE',  ( 0.000000000000000000, -0.9999939076577903929, 0.003490651415223739937 ) ) ;
#83921 = ORIENTED_EDGE ( 'NONE', *, *, #4222, .T. ) ;
#83922 = ORIENTED_EDGE ( 'NONE', *, *, #36838, .F. ) ;
#83923 = ORIENTED_EDGE ( 'NONE', *, *, #35316, .T. ) ;
#83924 = PLANE ( 'NONE',  #54712 ) ;
#83925 = VERTEX_POINT ( 'NONE', #84396 ) ;
#83926 = EDGE_LOOP ( 'NONE', ( #85902, #127427, #13646, #25217 ) ) ;
#83927 = ORIENTED_EDGE ( 'NONE', *, *, #99841, .T. ) ;
#83928 = DIRECTION ( 'NONE',  ( 0.000000000000000000, 1.000000000000000000, 0.000000000000000000 ) ) ;
#83929 = ADVANCED_FACE ( 'NONE', ( #83126 ), #97517, .T. ) ;
#83930 = DIRECTION ( 'NONE',  ( -0.000000000000000000, 1.000000000000000000, -0.000000000000000000 ) ) ;
#83931 = DIRECTION ( 'NONE',  ( 0.000000000000000000, 0.000000000000000000, -1.000000000000000000 ) ) ;
#83932 = FACE_OUTER_BOUND ( 'NONE', #74767, .T. ) ;
#83933 = FACE_OUTER_BOUND ( 'NONE', #94130, .T. ) ;
#83934 = DIRECTION ( 'NONE',  ( 0.000000000000000000, 1.000000000000000000, 0.000000000000000000 ) ) ;
#83935 = DIRECTION ( 'NONE',  ( 0.000000000000000000, -0.000000000000000000, 1.000000000000000000 ) ) ;
#83936 = AXIS2_PLACEMENT_3D ( 'NONE', #117592, #115680, #127452 ) ;
#83937 = ADVANCED_FACE ( 'NONE', ( #34679 ), #18100, .T. ) ;
#83938 = CONICAL_SURFACE ( 'NONE', #92253, 0.09999999999999982514, 0.003490658503988666988 ) ;
#83939 = ORIENTED_EDGE ( 'NONE', *, *, #90739, .F. ) ;
#83940 = DIRECTION ( 'NONE',  ( -4.274815082592931898E-19, -0.9999939076577903929, -0.003490651415223739937 ) ) ;
#83941 = ORIENTED_EDGE ( 'NONE', *, *, #110104, .F. ) ;
#83942 = DIRECTION ( 'NONE',  ( 0.000000000000000000, 0.000000000000000000, 1.000000000000000000 ) ) ;
#83943 = ORIENTED_EDGE ( 'NONE', *, *, #11403, .T. ) ;
#83944 = EDGE_CURVE ( 'NONE', #114247, #39021, #70335, .T. ) ;
#83945 = ADVANCED_FACE ( 'NONE', ( #123657 ), #106030, .T. ) ;
#83946 = EDGE_LOOP ( 'NONE', ( #48911, #120788 ) ) ;
#83947 = CONICAL_SURFACE ( 'NONE', #71420, 0.09999999999999982514, 0.003490658503988666988 ) ;
#83948 = CARTESIAN_POINT ( 'NONE',  ( 12.29999999999990479, 2.500000000000000000, 4.776537180435972196 ) ) ;
#83949 = DIRECTION ( 'NONE',  ( 0.000000000000000000, 1.000000000000000000, 0.000000000000000000 ) ) ;
#83950 = CONICAL_SURFACE ( 'NONE', #111128, 0.1000000000000000056, 0.003490658503988666988 ) ;
#83951 = VECTOR ( 'NONE', #9599, 1000.000000000000000 ) ;
#83952 = EDGE_CURVE ( 'NONE', #74899, #11954, #45398, .T. ) ;
#83953 = CARTESIAN_POINT ( 'NONE',  ( -7.100000000000013856, 2.500000000000000000, 3.637306695894644726 ) ) ;
#83954 = ORIENTED_EDGE ( 'NONE', *, *, #52785, .T. ) ;
#83955 = ORIENTED_EDGE ( 'NONE', *, *, #54688, .T. ) ;
#83956 = CARTESIAN_POINT ( 'NONE',  ( -7.950000000000016165, 2.500000000000000000, -6.495190528383297135 ) ) ;
#83957 = DIRECTION ( 'NONE',  ( 0.000000000000000000, 0.000000000000000000, 1.000000000000000000 ) ) ;
#83958 = ADVANCED_FACE ( 'NONE', ( #55587 ), #28674, .T. ) ;
#83959 = CARTESIAN_POINT ( 'NONE',  ( 4.349999999999939249, 12.50000000000000000, 2.576566944158910744 ) ) ;
#83960 = DIRECTION ( 'NONE',  ( 0.000000000000000000, 1.000000000000000000, 0.000000000000000000 ) ) ;
#83961 = VECTOR ( 'NONE', #44895, 1000.000000000000000 ) ;
#83962 = AXIS2_PLACEMENT_3D ( 'NONE', #56481, #68888, #96404 ) ;
#83963 = PLANE ( 'NONE',  #79316 ) ;
#83964 = VERTEX_POINT ( 'NONE', #13710 ) ;
#83965 = AXIS2_PLACEMENT_3D ( 'NONE', #122160, #83520, #123418 ) ;
#83966 = VECTOR ( 'NONE', #49429, 1000.000000000000000 ) ;
#83967 = ORIENTED_EDGE ( 'NONE', *, *, #76880, .T. ) ;
#83968 = CARTESIAN_POINT ( 'NONE',  ( 6.049999999999934097, 2.500000000000000000, -6.148780366869526226 ) ) ;
#83969 = DIRECTION ( 'NONE',  ( 0.000000000000000000, 0.000000000000000000, -1.000000000000000000 ) ) ;
#83970 = AXIS2_PLACEMENT_3D ( 'NONE', #74066, #34148, #106103 ) ;
#83971 = VECTOR ( 'NONE', #23914, 1000.000000000000000 ) ;
#83972 = CARTESIAN_POINT ( 'NONE',  ( 185.5885416670080872, -6.551208109652273848, -3.782341765625003571 ) ) ;
#83973 = DIRECTION ( 'NONE',  ( 0.000000000000000000, 0.000000000000000000, 1.000000000000000000 ) ) ;
#83974 = CARTESIAN_POINT ( 'NONE',  ( -12.69999999999999396, 2.500000000000000000, 0.3464101615137776813 ) ) ;
#83975 = DIRECTION ( 'NONE',  ( 0.000000000000000000, -0.9999939076577903929, 0.003490651415223739937 ) ) ;
#83976 = CARTESIAN_POINT ( 'NONE',  ( -9.550000000000002487, 2.500000000000000000, 6.495190528383297135 ) ) ;
#83977 = ORIENTED_EDGE ( 'NONE', *, *, #44271, .F. ) ;
#83978 = DIRECTION ( 'NONE',  ( 0.000000000000000000, 0.000000000000000000, 1.000000000000000000 ) ) ;
#83979 = ADVANCED_FACE ( 'NONE', ( #23541 ), #85091, .T. ) ;
#83980 = CARTESIAN_POINT ( 'NONE',  ( 5.599999999999931255, 12.50000000000000000, 4.048810130592458201 ) ) ;
#83981 = CARTESIAN_POINT ( 'NONE',  ( -6.450000000000017941, 2.500000000000000000, -6.841600689897077814 ) ) ;
#83982 = ORIENTED_EDGE ( 'NONE', *, *, #86480, .T. ) ;
#83983 = ADVANCED_FACE ( 'NONE', ( #16282 ), #83057, .T. ) ;
#83984 = EDGE_CURVE ( 'NONE', #84019, #109827, #22430, .T. ) ;
#83985 = DIRECTION ( 'NONE',  ( 0.000000000000000000, 0.000000000000000000, 1.000000000000000000 ) ) ;
#83986 = ORIENTED_EDGE ( 'NONE', *, *, #127278, .F. ) ;
#83987 = CARTESIAN_POINT ( 'NONE',  ( -11.84999999999999787, 2.500000000000000000, -6.148780366869522673 ) ) ;
#83988 = CIRCLE ( 'NONE', #23346, 0.06509327318403745899 ) ;
#83989 = CONICAL_SURFACE ( 'NONE', #29624, 0.1000000000000002554, 0.003490658503988666988 ) ;
#83990 = ADVANCED_FACE ( 'NONE', ( #28713 ), #5657, .T. ) ;
#83991 = AXIS2_PLACEMENT_3D ( 'NONE', #116620, #68815, #46593 ) ;
#83992 = ORIENTED_EDGE ( 'NONE', *, *, #16280, .T. ) ;
#83993 = DIRECTION ( 'NONE',  ( 0.000000000000000000, -0.9999939076577903929, 0.003490651415223739937 ) ) ;
#83994 = DIRECTION ( 'NONE',  ( 0.000000000000000000, 0.000000000000000000, 1.000000000000000000 ) ) ;
#83995 = EDGE_CURVE ( 'NONE', #80322, #97094, #98081, .T. ) ;
#83996 = DIRECTION ( 'NONE',  ( 0.000000000000000000, 0.000000000000000000, 1.000000000000000000 ) ) ;
#83997 = ADVANCED_FACE ( 'NONE', ( #107903 ), #26609, .T. ) ;
#83998 = ORIENTED_EDGE ( 'NONE', *, *, #45936, .F. ) ;
#84000 = CARTESIAN_POINT ( 'NONE',  ( 13.09999999999989839, 12.50000000000000000, -0.2813168883297409439 ) ) ;
#83999 = VECTOR ( 'NONE', #4443, 1000.000000000000000 ) ;
#84001 = AXIS2_PLACEMENT_3D ( 'NONE', #52691, #40308, #80228 ) ;
#84002 = EDGE_CURVE ( 'NONE', #21282, #129137, #6443, .T. ) ;
#84003 = CARTESIAN_POINT ( 'NONE',  ( 11.64999999999990266, 12.50000000000000000, 2.165063509461097713 ) ) ;
#84004 = AXIS2_PLACEMENT_3D ( 'NONE', #99211, #46886, #126732 ) ;
#84005 = AXIS2_PLACEMENT_3D ( 'NONE', #97678, #124573, #125210 ) ;
#84006 = VERTEX_POINT ( 'NONE', #127550 ) ;
#84007 = ADVANCED_FACE ( 'NONE', ( #46394 ), #108552, .T. ) ;
#84008 = AXIS2_PLACEMENT_3D ( 'NONE', #35124, #123470, #63925 ) ;
#84009 = CARTESIAN_POINT ( 'NONE',  ( 4.199999999999938005, 2.500000000000000000, 4.330127018922196314 ) ) ;
#84010 = EDGE_CURVE ( 'NONE', #58932, #70277, #27390, .T. ) ;
#84011 = ORIENTED_EDGE ( 'NONE', *, *, #82460, .F. ) ;
#84012 = ORIENTED_EDGE ( 'NONE', *, *, #94342, .F. ) ;
#84013 = CARTESIAN_POINT ( 'NONE',  ( 13.09999999999989839, 12.50000000000000000, 0.3464101615137735735 ) ) ;
#84014 = CARTESIAN_POINT ( 'NONE',  ( 8.949999999999921130, 2.500000000000000000, -6.741600689897078169 ) ) ;
#84015 = CARTESIAN_POINT ( 'NONE',  ( 2.699999999999947331, 2.500000000000000000, -0.3464101615137783474 ) ) ;
#84016 = ORIENTED_EDGE ( 'NONE', *, *, #44377, .F. ) ;
#84017 = CARTESIAN_POINT ( 'NONE',  ( -4.400000000000028777, 2.500000000000000000, -3.983716857408426293 ) ) ;
#84018 = DIRECTION ( 'NONE',  ( -0.000000000000000000, 1.000000000000000000, -0.000000000000000000 ) ) ;
#84019 = VERTEX_POINT ( 'NONE', #47066 ) ;
#84020 = DIRECTION ( 'NONE',  ( 0.000000000000000000, 1.000000000000000000, 0.000000000000000000 ) ) ;
#84021 = DIRECTION ( 'NONE',  ( 0.000000000000000000, 1.000000000000000000, 0.000000000000000000 ) ) ;
#84022 = DIRECTION ( 'NONE',  ( 0.000000000000000000, -0.000000000000000000, 1.000000000000000000 ) ) ;
#84023 = CARTESIAN_POINT ( 'NONE',  ( -1.450000000000035927, 2.500000000000000000, -6.048780366869526581 ) ) ;
#84024 = DIRECTION ( 'NONE',  ( 0.000000000000000000, 1.000000000000000000, 0.000000000000000000 ) ) ;
#84025 = CARTESIAN_POINT ( 'NONE',  ( 5.399999999999931966, 12.50000000000000000, 4.330127018922196314 ) ) ;
#84026 = PLANE ( 'NONE',  #94261 ) ;
#84027 = CIRCLE ( 'NONE', #27588, 0.06509327318403745899 ) ;
#84028 = AXIS2_PLACEMENT_3D ( 'NONE', #95072, #45336, #85245 ) ;
#84029 = EDGE_LOOP ( 'NONE', ( #121406, #45110 ) ) ;
#84030 = VERTEX_POINT ( 'NONE', #107258 ) ;
#84031 = EDGE_LOOP ( 'NONE', ( #98718, #64803 ) ) ;
#84032 = ORIENTED_EDGE ( 'NONE', *, *, #104492, .F. ) ;
#84033 = CARTESIAN_POINT ( 'NONE',  ( -11.44999999999999751, 12.50000000000000000, 6.841600689897072485 ) ) ;
#84034 = DIRECTION ( 'NONE',  ( 0.000000000000000000, -1.000000000000000000, 0.000000000000000000 ) ) ;
#84035 = CARTESIAN_POINT ( 'NONE',  ( -12.29999999999999538, 2.500000000000000000, 4.776537180435972196 ) ) ;
#84036 = ORIENTED_EDGE ( 'NONE', *, *, #28397, .T. ) ;
#84037 = FACE_BOUND ( 'NONE', #128590, .T. ) ;
#84038 = VECTOR ( 'NONE', #14907, 1000.000000000000000 ) ;
#84039 = DIRECTION ( 'NONE',  ( 0.000000000000000000, 0.000000000000000000, 1.000000000000000000 ) ) ;
#84040 = DIRECTION ( 'NONE',  ( -0.000000000000000000, 1.000000000000000000, -0.000000000000000000 ) ) ;
#84041 = AXIS2_PLACEMENT_3D ( 'NONE', #42913, #20675, #69765 ) ;
#84043 = CARTESIAN_POINT ( 'NONE',  ( -6.850000000000013856, 12.50000000000000000, 2.446380397790835826 ) ) ;
#84042 = AXIS2_PLACEMENT_3D ( 'NONE', #41493, #113426, #21841 ) ;
#84044 = AXIS2_PLACEMENT_3D ( 'NONE', #92672, #13454, #3644 ) ;
#84045 = EDGE_CURVE ( 'NONE', #98668, #47201, #93417, .T. ) ;
#84046 = DIRECTION ( 'NONE',  ( -0.000000000000000000, 1.000000000000000000, -0.000000000000000000 ) ) ;
#84047 = CARTESIAN_POINT ( 'NONE',  ( -2.500000000000030642, 12.50000000000000000, -5.022947341949754119 ) ) ;
#84048 = DIRECTION ( 'NONE',  ( 0.000000000000000000, 1.000000000000000000, 0.000000000000000000 ) ) ;
#84049 = CARTESIAN_POINT ( 'NONE',  ( 4.399999999999939071, 12.50000000000000000, -0.3464101615137782364 ) ) ;
#84050 = CARTESIAN_POINT ( 'NONE',  ( -3.150000000000029221, 2.500000000000000000, -1.818653347947326138 ) ) ;
#84051 = CARTESIAN_POINT ( 'NONE',  ( 5.849999999999933920, 2.500000000000000000, 5.702370205355745014 ) ) ;
#84052 = CONICAL_SURFACE ( 'NONE', #61084, 0.1000000000000002554, 0.003490658503988666988 ) ;
#84053 = DIRECTION ( 'NONE',  ( -4.274815082592931898E-19, -0.9999939076577903929, -0.003490651415223739937 ) ) ;
#84054 = VERTEX_POINT ( 'NONE', #37250 ) ;
#84055 = CIRCLE ( 'NONE', #127976, 0.06509327318403745899 ) ;
#84056 = ADVANCED_FACE ( 'NONE', ( #58812 ), #67970, .T. ) ;
#84057 = ORIENTED_EDGE ( 'NONE', *, *, #1246, .F. ) ;
#84058 = EDGE_LOOP ( 'NONE', ( #107655, #77339, #92101, #92248 ) ) ;
#84059 = VERTEX_POINT ( 'NONE', #75857 ) ;
#84061 = ORIENTED_EDGE ( 'NONE', *, *, #102573, .T. ) ;
#84060 = CIRCLE ( 'NONE', #102828, 0.06509327318403745899 ) ;
#84062 = AXIS2_PLACEMENT_3D ( 'NONE', #8575, #87788, #6626 ) ;
#84063 = CIRCLE ( 'NONE', #113307, 0.06509327318403745899 ) ;
#84064 = ORIENTED_EDGE ( 'NONE', *, *, #4510, .T. ) ;
#84065 = DIRECTION ( 'NONE',  ( 0.000000000000000000, -0.9999939076577903929, 0.003490651415223739937 ) ) ;
#84066 = VERTEX_POINT ( 'NONE', #76521 ) ;
#84067 = VERTEX_POINT ( 'NONE', #117700 ) ;
#84068 = VECTOR ( 'NONE', #48449, 1000.000000000000000 ) ;
#84069 = VECTOR ( 'NONE', #84529, 1000.000000000000000 ) ;
#84070 = FACE_OUTER_BOUND ( 'NONE', #86404, .T. ) ;
#84071 = DIRECTION ( 'NONE',  ( 0.000000000000000000, 0.000000000000000000, -1.000000000000000000 ) ) ;
#84072 = DIRECTION ( 'NONE',  ( -0.000000000000000000, 1.000000000000000000, -0.000000000000000000 ) ) ;
#84073 = DIRECTION ( 'NONE',  ( 0.000000000000000000, -0.000000000000000000, 1.000000000000000000 ) ) ;
#84074 = ORIENTED_EDGE ( 'NONE', *, *, #21618, .F. ) ;
#84075 = DIRECTION ( 'NONE',  ( 0.000000000000000000, -0.000000000000000000, 1.000000000000000000 ) ) ;
#84076 = ORIENTED_EDGE ( 'NONE', *, *, #93874, .T. ) ;
#84077 = ORIENTED_EDGE ( 'NONE', *, *, #74794, .F. ) ;
#84079 = VERTEX_POINT ( 'NONE', #86974 ) ;
#84078 = DIRECTION ( 'NONE',  ( 0.000000000000000000, -0.000000000000000000, 1.000000000000000000 ) ) ;
#84080 = DIRECTION ( 'NONE',  ( 0.000000000000000000, -0.000000000000000000, 1.000000000000000000 ) ) ;
#84081 = ORIENTED_EDGE ( 'NONE', *, *, #70830, .T. ) ;
#84082 = VERTEX_POINT ( 'NONE', #77160 ) ;
#84083 = CARTESIAN_POINT ( 'NONE',  ( -12.09999999999999609, 12.50000000000000000, -0.6928203230275501445 ) ) ;
#84084 = DIRECTION ( 'NONE',  ( 0.000000000000000000, 0.000000000000000000, 1.000000000000000000 ) ) ;
#84085 = DIRECTION ( 'NONE',  ( -0.000000000000000000, 1.000000000000000000, -0.000000000000000000 ) ) ;
#84087 = CARTESIAN_POINT ( 'NONE',  ( -1.850000000000033840, 12.50000000000000000, 2.511473670974873507 ) ) ;
#84086 = AXIS2_PLACEMENT_3D ( 'NONE', #12216, #33800, #2382 ) ;
#84088 = AXIS2_PLACEMENT_3D ( 'NONE', #129109, #78707, #19777 ) ;
#84089 = CARTESIAN_POINT ( 'NONE',  ( -10.60000000000000142, 12.50000000000000000, -0.3464101615137782364 ) ) ;
#84090 = ORIENTED_EDGE ( 'NONE', *, *, #57255, .T. ) ;
#84091 = CARTESIAN_POINT ( 'NONE',  ( -8.950000000000004619, 2.500000000000000000, 6.148780366869520897 ) ) ;
#84092 = ADVANCED_FACE ( 'NONE', ( #9055 ), #76694, .T. ) ;
#84093 = AXIS2_PLACEMENT_3D ( 'NONE', #43462, #3521, #95127 ) ;
#84094 = ORIENTED_EDGE ( 'NONE', *, *, #88795, .T. ) ;
#84095 = CARTESIAN_POINT ( 'NONE',  ( 17.50000000000000000, 2.499999999999999556, -3.666666666666662522 ) ) ;
#84096 = AXIS2_PLACEMENT_3D ( 'NONE', #70728, #10503, #119826 ) ;
#84097 = EDGE_LOOP ( 'NONE', ( #84057, #29794 ) ) ;
#84098 = DIRECTION ( 'NONE',  ( -0.000000000000000000, -1.000000000000000000, -0.000000000000000000 ) ) ;
#84099 = DIRECTION ( 'NONE',  ( 0.000000000000000000, 1.000000000000000000, 0.000000000000000000 ) ) ;
#84100 = CIRCLE ( 'NONE', #61126, 0.06509327318403745899 ) ;
#84101 = AXIS2_PLACEMENT_3D ( 'NONE', #119666, #58825, #49667 ) ;
#84103 = EDGE_CURVE ( 'NONE', #66863, #57597, #122756, .T. ) ;
#84102 = CARTESIAN_POINT ( 'NONE',  ( -7.050000000000013145, 12.50000000000000000, 2.165063509461097713 ) ) ;
#84104 = CARTESIAN_POINT ( 'NONE',  ( -8.749999999999971578, 2.500000000000000000, 6.395190528383296602 ) ) ;
#84105 = EDGE_CURVE ( 'NONE', #35498, #22187, #21858, .T. ) ;
#84106 = ORIENTED_EDGE ( 'NONE', *, *, #27520, .F. ) ;
#84107 = AXIS2_PLACEMENT_3D ( 'NONE', #11671, #101356, #42438 ) ;
#84108 = EDGE_CURVE ( 'NONE', #77492, #78495, #74630, .T. ) ;
#84109 = DIRECTION ( 'NONE',  ( 0.000000000000000000, 0.000000000000000000, -1.000000000000000000 ) ) ;
#84110 = ORIENTED_EDGE ( 'NONE', *, *, #69111, .T. ) ;
#84111 = EDGE_CURVE ( 'NONE', #21874, #64587, #30746, .T. ) ;
#84112 = VERTEX_POINT ( 'NONE', #70553 ) ;
#84113 = EDGE_LOOP ( 'NONE', ( #60895, #90914, #82855, #52062 ) ) ;
#84114 = DIRECTION ( 'NONE',  ( -0.000000000000000000, -1.000000000000000000, -0.000000000000000000 ) ) ;
#84115 = DIRECTION ( 'NONE',  ( 0.000000000000000000, 0.000000000000000000, 1.000000000000000000 ) ) ;
#84116 = EDGE_CURVE ( 'NONE', #122938, #39770, #36986, .T. ) ;
#84117 = CARTESIAN_POINT ( 'NONE',  ( 185.9010416670080303, -4.367472073101519747, 7.564683531249999149 ) ) ;
#84118 = LINE ( 'NONE', #16654, #40848 ) ;
#84119 = AXIS2_PLACEMENT_3D ( 'NONE', #16826, #128779, #78381 ) ;
#84120 = CARTESIAN_POINT ( 'NONE',  ( 4.349999999999940137, 2.500000000000000000, -2.511473670974877948 ) ) ;
#84121 = DIRECTION ( 'NONE',  ( -0.000000000000000000, -1.000000000000000000, -0.000000000000000000 ) ) ;
#84122 = AXIS2_PLACEMENT_3D ( 'NONE', #101051, #129256, #29112 ) ;
#84123 = ORIENTED_EDGE ( 'NONE', *, *, #80631, .F. ) ;
#84124 = CARTESIAN_POINT ( 'NONE',  ( 9.599999999999914380, 2.500000000000000000, -3.537306695894649966 ) ) ;
#84125 = EDGE_LOOP ( 'NONE', ( #105632, #80026 ) ) ;
#84126 = CARTESIAN_POINT ( 'NONE',  ( 4.799999999999937650, 12.50000000000000000, -0.2813168883297408329 ) ) ;
#84127 = CARTESIAN_POINT ( 'NONE',  ( 4.999999999999933387, 2.500000000000000000, 5.022947341949748790 ) ) ;
#84128 = DIRECTION ( 'NONE',  ( 0.000000000000000000, 1.000000000000000000, 0.000000000000000000 ) ) ;
#84129 = AXIS2_PLACEMENT_3D ( 'NONE', #108946, #97213, #76933 ) ;
#84130 = VECTOR ( 'NONE', #69606, 1000.000000000000000 ) ;
#84131 = ORIENTED_EDGE ( 'NONE', *, *, #127711, .F. ) ;
#84132 = CONICAL_SURFACE ( 'NONE', #10958, 0.1000000000000002554, 0.003490658503988666988 ) ;
#84133 = DIRECTION ( 'NONE',  ( -4.274815082592931898E-19, -0.9999939076577903929, -0.003490651415223739937 ) ) ;
#84134 = DIRECTION ( 'NONE',  ( 1.000000000000000000, -0.000000000000000000, -0.000000000000000000 ) ) ;
#84135 = CIRCLE ( 'NONE', #6849, 0.06509327318403745899 ) ;
#84136 = VERTEX_POINT ( 'NONE', #121580 ) ;
#84138 = AXIS2_PLACEMENT_3D ( 'NONE', #7222, #98197, #77274 ) ;
#84137 = FACE_OUTER_BOUND ( 'NONE', #18325, .T. ) ;
#84139 = VERTEX_POINT ( 'NONE', #41767 ) ;
#84140 = AXIS2_PLACEMENT_3D ( 'NONE', #15002, #36629, #16299 ) ;
#84142 = ORIENTED_EDGE ( 'NONE', *, *, #86763, .F. ) ;
#84141 = AXIS2_PLACEMENT_3D ( 'NONE', #1991, #100208, #72043 ) ;
#84143 = VECTOR ( 'NONE', #49165, 1000.000000000000000 ) ;
#84144 = CARTESIAN_POINT ( 'NONE',  ( -12.89999999999999147, 2.500000000000000000, 4.922947341949748257 ) ) ;
#84145 = ADVANCED_FACE ( 'NONE', ( #62042 ), #49651, .T. ) ;
#84146 = EDGE_CURVE ( 'NONE', #24096, #64597, #20820, .T. ) ;
#84148 = ORIENTED_EDGE ( 'NONE', *, *, #64388, .T. ) ;
#84147 = CONICAL_SURFACE ( 'NONE', #86201, 0.1000000000000002554, 0.003490658503988666988 ) ;
#84149 = PLANE ( 'NONE',  #40522 ) ;
#84151 = EDGE_CURVE ( 'NONE', #27897, #83521, #1172, .T. ) ;
#84150 = DIRECTION ( 'NONE',  ( 0.000000000000000000, 1.000000000000000000, 0.000000000000000000 ) ) ;
#84152 = FACE_OUTER_BOUND ( 'NONE', #2221, .T. ) ;
#84153 = EDGE_LOOP ( 'NONE', ( #69226, #42655, #15970, #119342 ) ) ;
#84154 = AXIS2_PLACEMENT_3D ( 'NONE', #91615, #2570, #1935 ) ;
#84155 = ADVANCED_FACE ( 'NONE', ( #71861 ), #11932, .T. ) ;
#84156 = CARTESIAN_POINT ( 'NONE',  ( 3.349999999999944578, 12.50000000000000000, -5.802370205355749988 ) ) ;
#84158 = ORIENTED_EDGE ( 'NONE', *, *, #37959, .F. ) ;
#84157 = DIRECTION ( 'NONE',  ( 0.000000000000000000, 0.000000000000000000, 1.000000000000000000 ) ) ;
#84159 = ADVANCED_FACE ( 'NONE', ( #100648 ), #64161, .T. ) ;
#84160 = CARTESIAN_POINT ( 'NONE',  ( -3.750000000000027534, 2.500000000000000000, 2.957883832488649389 ) ) ;
#84161 = CARTESIAN_POINT ( 'NONE',  ( 1.449999999999950440, 12.50000000000000000, 6.083687093685482772 ) ) ;
#84162 = ORIENTED_EDGE ( 'NONE', *, *, #3509, .F. ) ;
#84163 = EDGE_CURVE ( 'NONE', #60727, #18083, #89302, .T. ) ;
#84164 = EDGE_CURVE ( 'NONE', #63903, #32296, #9887, .T. ) ;
#84165 = EDGE_LOOP ( 'NONE', ( #109699, #81108, #95973, #19312 ) ) ;
#84166 = VERTEX_POINT ( 'NONE', #10348 ) ;
#84167 = DIRECTION ( 'NONE',  ( 0.000000000000000000, 1.000000000000000000, 0.000000000000000000 ) ) ;
#84168 = LINE ( 'NONE', #44244, #85470 ) ;
#84169 = DIRECTION ( 'NONE',  ( -0.000000000000000000, 1.000000000000000000, -0.000000000000000000 ) ) ;
#84170 = FACE_BOUND ( 'NONE', #33700, .T. ) ;
#84171 = ORIENTED_EDGE ( 'NONE', *, *, #83379, .T. ) ;
#84172 = CARTESIAN_POINT ( 'NONE',  ( 185.8177083336747444, 4.367472073101515306, 7.564683531250000925 ) ) ;
#84173 = ADVANCED_FACE ( 'NONE', ( #111781 ), #22131, .T. ) ;
#84174 = DIRECTION ( 'NONE',  ( 0.000000000000000000, 0.000000000000000000, 1.000000000000000000 ) ) ;
#84175 = CARTESIAN_POINT ( 'NONE',  ( -14.59999999999998366, 2.500000000000000000, 0.6928203230275518099 ) ) ;
#84176 = CIRCLE ( 'NONE', #27746, 0.06509327318403741736 ) ;
#84177 = AXIS2_PLACEMENT_3D ( 'NONE', #61549, #111251, #21615 ) ;
#84179 = AXIS2_PLACEMENT_3D ( 'NONE', #94252, #123079, #82523 ) ;
#84178 = DIRECTION ( 'NONE',  ( 0.000000000000000000, 0.000000000000000000, -1.000000000000000000 ) ) ;
#84180 = FACE_OUTER_BOUND ( 'NONE', #123144, .T. ) ;
#84181 = DIRECTION ( 'NONE',  ( 0.000000000000000000, 0.000000000000000000, 1.000000000000000000 ) ) ;
#84182 = AXIS2_PLACEMENT_3D ( 'NONE', #75896, #74614, #25494 ) ;
#84184 = CARTESIAN_POINT ( 'NONE',  ( 184.2500000000000000, 9.429780353434619030E-16, -7.700000000000000178 ) ) ;
#84183 = CIRCLE ( 'NONE', #73715, 0.1000000000000000472 ) ;
#84185 = ORIENTED_EDGE ( 'NONE', *, *, #3558, .T. ) ;
#84186 = EDGE_LOOP ( 'NONE', ( #28183, #46230, #18439, #55001 ) ) ;
#84187 = ORIENTED_EDGE ( 'NONE', *, *, #62145, .F. ) ;
#84188 = VERTEX_POINT ( 'NONE', #79109 ) ;
#84190 = EDGE_LOOP ( 'NONE', ( #27063, #10029 ) ) ;
#84189 = CIRCLE ( 'NONE', #75781, 0.1000000000000002554 ) ;
#84191 = LINE ( 'NONE', #114304, #21320 ) ;
#84192 = CIRCLE ( 'NONE', #126050, 0.06509327318403745899 ) ;
#84193 = CONICAL_SURFACE ( 'NONE', #27763, 0.09999999999999982514, 0.003490658503988666988 ) ;
#84194 = FACE_OUTER_BOUND ( 'NONE', #75987, .T. ) ;
#84195 = ORIENTED_EDGE ( 'NONE', *, *, #108221, .T. ) ;
#84196 = FACE_BOUND ( 'NONE', #36, .T. ) ;
#84197 = CARTESIAN_POINT ( 'NONE',  ( -3.350000000000031619, 2.500000000000000000, -7.288010851410854585 ) ) ;
#84198 = CARTESIAN_POINT ( 'NONE',  ( 6.449999999999928235, 2.500000000000000000, 2.411473670974873862 ) ) ;
#84199 = ORIENTED_EDGE ( 'NONE', *, *, #88894, .T. ) ;
#84200 = DIRECTION ( 'NONE',  ( 0.000000000000000000, -0.000000000000000000, 1.000000000000000000 ) ) ;
#84201 = DIRECTION ( 'NONE',  ( 0.000000000000000000, 0.000000000000000000, 1.000000000000000000 ) ) ;
#84202 = CARTESIAN_POINT ( 'NONE',  ( 4.799999999999935874, 2.500000000000000000, 0.2464101615137735679 ) ) ;
#84203 = ORIENTED_EDGE ( 'NONE', *, *, #64785, .F. ) ;
#84204 = DIRECTION ( 'NONE',  ( 0.000000000000000000, 0.000000000000000000, 1.000000000000000000 ) ) ;
#84205 = AXIS2_PLACEMENT_3D ( 'NONE', #91254, #109613, #61150 ) ;
#84206 = ORIENTED_EDGE ( 'NONE', *, *, #117667, .T. ) ;
#84207 = EDGE_CURVE ( 'NONE', #37050, #40175, #59487, .T. ) ;
#84208 = EDGE_LOOP ( 'NONE', ( #46405, #80934, #154, #17669 ) ) ;
#84209 = VERTEX_POINT ( 'NONE', #99387 ) ;
#84210 = DIRECTION ( 'NONE',  ( 0.000000000000000000, 0.000000000000000000, 1.000000000000000000 ) ) ;
#84211 = CARTESIAN_POINT ( 'NONE',  ( -11.04999999999999893, 2.500000000000000000, 1.918653347947321564 ) ) ;
#84212 = CARTESIAN_POINT ( 'NONE',  ( -3.950000000000025491, 12.50000000000000000, 6.213873640053559022 ) ) ;
#84213 = ORIENTED_EDGE ( 'NONE', *, *, #34960, .T. ) ;
#84214 = FACE_OUTER_BOUND ( 'NONE', #64652, .T. ) ;
#84215 = AXIS2_PLACEMENT_3D ( 'NONE', #107704, #58612, #87398 ) ;
#84216 = DIRECTION ( 'NONE',  ( -0.000000000000000000, 1.000000000000000000, -0.000000000000000000 ) ) ;
#84217 = FACE_OUTER_BOUND ( 'NONE', #91806, .T. ) ;
#84218 = FACE_OUTER_BOUND ( 'NONE', #56129, .T. ) ;
#84219 = ORIENTED_EDGE ( 'NONE', *, *, #117121, .F. ) ;
#84220 = LINE ( 'NONE', #34515, #22411 ) ;
#84221 = AXIS2_PLACEMENT_3D ( 'NONE', #120720, #113311, #124430 ) ;
#84222 = ORIENTED_EDGE ( 'NONE', *, *, #98279, .T. ) ;
#84223 = CARTESIAN_POINT ( 'NONE',  ( 8.349999999999919709, 2.500000000000000000, -2.065063509461102065 ) ) ;
#84224 = AXIS2_PLACEMENT_3D ( 'NONE', #5374, #94395, #85231 ) ;
#84225 = ORIENTED_EDGE ( 'NONE', *, *, #30986, .T. ) ;
#84226 = AXIS2_PLACEMENT_3D ( 'NONE', #747, #79338, #28292 ) ;
#84227 = VERTEX_POINT ( 'NONE', #129513 ) ;
#84228 = CARTESIAN_POINT ( 'NONE',  ( 3.349999999999942801, 12.50000000000000000, 2.922977105672686982 ) ) ;
#84229 = DIRECTION ( 'NONE',  ( 0.000000000000000000, 1.000000000000000000, 0.000000000000000000 ) ) ;
#84230 = DIRECTION ( 'NONE',  ( 0.000000000000000000, 0.000000000000000000, 1.000000000000000000 ) ) ;
#84231 = DIRECTION ( 'NONE',  ( -4.274815082592931898E-19, -0.9999939076577903929, -0.003490651415223739937 ) ) ;
#84232 = CARTESIAN_POINT ( 'NONE',  ( 184.5000000000000284, -3.559465329748744633, -6.843514285309209022 ) ) ;
#84233 = CIRCLE ( 'NONE', #88136, 0.06509327318403745899 ) ;
#84234 = ORIENTED_EDGE ( 'NONE', *, *, #80522, .T. ) ;
#84235 = EDGE_LOOP ( 'NONE', ( #34574, #105885, #70908, #53736 ) ) ;
#84236 = AXIS2_PLACEMENT_3D ( 'NONE', #88802, #87497, #128757 ) ;
#84237 = CARTESIAN_POINT ( 'NONE',  ( 11.64999999999990621, 2.500000000000000000, -2.265063509461101798 ) ) ;
#84239 = AXIS2_PLACEMENT_3D ( 'NONE', #128225, #78489, #118383 ) ;
#84238 = CARTESIAN_POINT ( 'NONE',  ( 76.44225496929378494, 3.905139198807624723, -5.869654418954768360 ) ) ;
#84240 = CIRCLE ( 'NONE', #67504, 0.06509327318403745899 ) ;
#84241 = CIRCLE ( 'NONE', #123950, 0.06509327318403745899 ) ;
#84242 = DIRECTION ( 'NONE',  ( 0.000000000000000000, -0.9999939076577903929, 0.003490651415223739937 ) ) ;
#84243 = VERTEX_POINT ( 'NONE', #39835 ) ;
#84244 = VERTEX_POINT ( 'NONE', #90176 ) ;
#84245 = CARTESIAN_POINT ( 'NONE',  ( 4.349999999999941025, 2.500000000000000000, -6.048780366869526581 ) ) ;
#84246 = AXIS2_PLACEMENT_3D ( 'NONE', #22727, #113016, #62647 ) ;
#84247 = ORIENTED_EDGE ( 'NONE', *, *, #82821, .T. ) ;
#84248 = DIRECTION ( 'NONE',  ( -0.000000000000000000, -1.000000000000000000, -0.000000000000000000 ) ) ;
#84249 = EDGE_CURVE ( 'NONE', #108498, #67661, #20256, .T. ) ;
#84250 = DIRECTION ( 'NONE',  ( -0.000000000000000000, -1.000000000000000000, -0.000000000000000000 ) ) ;
#84251 = ORIENTED_EDGE ( 'NONE', *, *, #47028, .T. ) ;
#84252 = AXIS2_PLACEMENT_3D ( 'NONE', #48318, #37848, #78447 ) ;
#84253 = CARTESIAN_POINT ( 'NONE',  ( 7.049999999999926992, 2.500000000000000000, 2.065063509461097624 ) ) ;
#84254 = DIRECTION ( 'NONE',  ( -0.000000000000000000, 1.000000000000000000, -0.000000000000000000 ) ) ;
#84255 = CARTESIAN_POINT ( 'NONE',  ( 6.049999999999930544, 2.500000000000000000, 2.611473670974873151 ) ) ;
#84256 = ADVANCED_FACE ( 'NONE', ( #109849 ), #7716, .T. ) ;
#84257 = DIRECTION ( 'NONE',  ( 0.000000000000000000, 0.000000000000000000, -1.000000000000000000 ) ) ;
#84258 = EDGE_CURVE ( 'NONE', #72199, #41083, #80394, .T. ) ;
#84259 = ORIENTED_EDGE ( 'NONE', *, *, #32775, .T. ) ;
#84260 = DIRECTION ( 'NONE',  ( 0.000000000000000000, 1.000000000000000000, 0.000000000000000000 ) ) ;
#84261 = CARTESIAN_POINT ( 'NONE',  ( 32.15727368887977633, -2.842525632566917704, 4.549395963656282404 ) ) ;
#84262 = EDGE_CURVE ( 'NONE', #27061, #54972, #65650, .T. ) ;
#84263 = ORIENTED_EDGE ( 'NONE', *, *, #121865, .T. ) ;
#84264 = EDGE_CURVE ( 'NONE', #70303, #100605, #54774, .T. ) ;
#84265 = ORIENTED_EDGE ( 'NONE', *, *, #4412, .T. ) ;
#84266 = VECTOR ( 'NONE', #61579, 1000.000000000000000 ) ;
#84267 = CIRCLE ( 'NONE', #52976, 0.1000000000000002554 ) ;
#84268 = ADVANCED_FACE ( 'NONE', ( #92120 ), #22772, .T. ) ;
#84269 = CARTESIAN_POINT ( 'NONE',  ( 184.5468750003414300, -8.734944146203032389, -1.604583208406768146E-15 ) ) ;
#84271 = EDGE_CURVE ( 'NONE', #125100, #23084, #85189, .T. ) ;
#84270 = DIRECTION ( 'NONE',  ( -0.000000000000000000, 1.000000000000000000, -0.000000000000000000 ) ) ;
#84272 = ADVANCED_FACE ( 'NONE', ( #72507 ), #112429, .T. ) ;
#84273 = CARTESIAN_POINT ( 'NONE',  ( -13.14999999999999147, 2.500000000000000000, 2.511473670974877503 ) ) ;
#84274 = DIRECTION ( 'NONE',  ( 0.000000000000000000, 0.000000000000000000, 1.000000000000000000 ) ) ;
#84275 = CARTESIAN_POINT ( 'NONE',  ( -2.300000000000032685, 12.50000000000000000, -4.741630453620016006 ) ) ;
#84276 = CARTESIAN_POINT ( 'NONE',  ( -10.20000000000000462, 12.50000000000000000, -4.676537180435973440 ) ) ;
#84277 = FACE_OUTER_BOUND ( 'NONE', #36703, .T. ) ;
#84278 = CONICAL_SURFACE ( 'NONE', #123984, 0.1000000000000002554, 0.003490658503988666988 ) ;
#84279 = DIRECTION ( 'NONE',  ( 0.000000000000000000, -0.000000000000000000, 1.000000000000000000 ) ) ;
#84280 = DIRECTION ( 'NONE',  ( 0.000000000000000000, 0.000000000000000000, 1.000000000000000000 ) ) ;
#84281 = DIRECTION ( 'NONE',  ( 0.000000000000000000, 1.000000000000000000, 0.000000000000000000 ) ) ;
#84282 = AXIS2_PLACEMENT_3D ( 'NONE', #50021, #29089, #87961 ) ;
#84283 = EDGE_CURVE ( 'NONE', #68896, #12189, #62223, .T. ) ;
#84284 = PLANE ( 'NONE',  #22954 ) ;
#84285 = VERTEX_POINT ( 'NONE', #65234 ) ;
#84286 = CIRCLE ( 'NONE', #109323, 0.06509327318403745899 ) ;
#84287 = VERTEX_POINT ( 'NONE', #82326 ) ;
#84288 = AXIS2_PLACEMENT_3D ( 'NONE', #124876, #65940, #64659 ) ;
#84289 = AXIS2_PLACEMENT_3D ( 'NONE', #23122, #120686, #70938 ) ;
#84290 = ORIENTED_EDGE ( 'NONE', *, *, #38473, .F. ) ;
#84291 = CIRCLE ( 'NONE', #98859, 0.1000000000000000472 ) ;
#84292 = CIRCLE ( 'NONE', #21600, 0.06509327318403745899 ) ;
#84293 = ORIENTED_EDGE ( 'NONE', *, *, #24651, .T. ) ;
#84294 = LINE ( 'NONE', #21023, #83355 ) ;
#84295 = DIRECTION ( 'NONE',  ( 0.000000000000000000, 1.000000000000000000, 0.000000000000000000 ) ) ;
#84296 = DIRECTION ( 'NONE',  ( 0.000000000000000000, 1.000000000000000000, 0.000000000000000000 ) ) ;
#84297 = VECTOR ( 'NONE', #51145, 1000.000000000000000 ) ;
#84298 = ORIENTED_EDGE ( 'NONE', *, *, #6545, .T. ) ;
#84299 = CARTESIAN_POINT ( 'NONE',  ( 13.34999999999990017, 12.50000000000000000, 2.857883832488649301 ) ) ;
#84300 = DIRECTION ( 'NONE',  ( -0.000000000000000000, -1.000000000000000000, -0.000000000000000000 ) ) ;
#84302 = EDGE_LOOP ( 'NONE', ( #63876, #19856 ) ) ;
#84301 = LINE ( 'NONE', #105878, #14080 ) ;
#84303 = DIRECTION ( 'NONE',  ( -0.000000000000000000, -1.000000000000000000, -0.000000000000000000 ) ) ;
#84305 = PLANE ( 'NONE',  #27058 ) ;
#84304 = AXIS2_PLACEMENT_3D ( 'NONE', #68227, #116045, #55204 ) ;
#84306 = ORIENTED_EDGE ( 'NONE', *, *, #120346, .T. ) ;
#84307 = VERTEX_POINT ( 'NONE', #14199 ) ;
#84308 = VERTEX_POINT ( 'NONE', #12270 ) ;
#84309 = VERTEX_POINT ( 'NONE', #122253 ) ;
#84310 = DIRECTION ( 'NONE',  ( 0.000000000000000000, -0.9999939076577903929, 0.003490651415223739937 ) ) ;
#84311 = ADVANCED_FACE ( 'NONE', ( #44315 ), #108161, .T. ) ;
#84313 = CONICAL_SURFACE ( 'NONE', #48830, 0.1000000000000000472, 0.003490658503988666988 ) ;
#84312 = CARTESIAN_POINT ( 'NONE',  ( -12.69999999999999041, 2.500000000000000000, 4.083716857408421497 ) ) ;
#84315 = EDGE_CURVE ( 'NONE', #40907, #56932, #14829, .T. ) ;
#84314 = DIRECTION ( 'NONE',  ( 0.000000000000000000, 1.000000000000000000, 0.000000000000000000 ) ) ;
#84316 = VECTOR ( 'NONE', #93226, 1000.000000000000000 ) ;
#84317 = CARTESIAN_POINT ( 'NONE',  ( -1.650000000000034328, 2.500000000000000000, -6.395190528383301931 ) ) ;
#84318 = ORIENTED_EDGE ( 'NONE', *, *, #54396, .F. ) ;
#84319 = ADVANCED_FACE ( 'NONE', ( #83614 ), #126963, .T. ) ;
#84320 = DIRECTION ( 'NONE',  ( -4.274815082592931898E-19, -0.9999939076577903929, -0.003490651415223739937 ) ) ;
#84321 = EDGE_LOOP ( 'NONE', ( #37689, #22529, #71808, #100251 ) ) ;
#84322 = CARTESIAN_POINT ( 'NONE',  ( 2.699999999999946443, 12.50000000000000000, 0.2813168883297361700 ) ) ;
#84323 = DIRECTION ( 'NONE',  ( -0.000000000000000000, -1.000000000000000000, -0.000000000000000000 ) ) ;
#84324 = CARTESIAN_POINT ( 'NONE',  ( 11.04999999999990834, 2.500000000000000000, 1.718653347947321386 ) ) ;
#84325 = CARTESIAN_POINT ( 'NONE',  ( 20.64614705758971525, -2.669560853935425637, 2.247897417627709338 ) ) ;
#84326 = EDGE_CURVE ( 'NONE', #44264, #78788, #47547, .T. ) ;
#84327 = CIRCLE ( 'NONE', #2851, 0.06509327318403745899 ) ;
#84328 = AXIS2_PLACEMENT_3D ( 'NONE', #62713, #13583, #53534 ) ;
#84329 = EDGE_CURVE ( 'NONE', #72026, #117286, #101921, .T. ) ;
#84330 = CONICAL_SURFACE ( 'NONE', #27896, 0.1000000000000000472, 0.003490658503988666988 ) ;
#84331 = VERTEX_POINT ( 'NONE', #73141 ) ;
#84332 = EDGE_CURVE ( 'NONE', #129616, #36522, #120697, .T. ) ;
#84333 = EDGE_LOOP ( 'NONE', ( #24973, #100390 ) ) ;
#84334 = ORIENTED_EDGE ( 'NONE', *, *, #62308, .T. ) ;
#84335 = CARTESIAN_POINT ( 'NONE',  ( 11.89999999999990443, 2.500000000000000000, 0.3464101615137736845 ) ) ;
#84336 = FACE_OUTER_BOUND ( 'NONE', #12767, .T. ) ;
#84337 = DIRECTION ( 'NONE',  ( 0.000000000000000000, 1.000000000000000000, 0.000000000000000000 ) ) ;
#84338 = FACE_BOUND ( 'NONE', #77982, .T. ) ;
#84339 = AXIS2_PLACEMENT_3D ( 'NONE', #29490, #26908, #38686 ) ;
#84340 = DIRECTION ( 'NONE',  ( -0.000000000000000000, 1.000000000000000000, -0.000000000000000000 ) ) ;
#84341 = DIRECTION ( 'NONE',  ( 0.000000000000000000, 1.000000000000000000, 0.000000000000000000 ) ) ;
#84342 = EDGE_CURVE ( 'NONE', #119121, #36522, #13559, .T. ) ;
#84343 = CARTESIAN_POINT ( 'NONE',  ( 12.69999999999990159, 2.500000000000000000, -3.983716857408426293 ) ) ;
#84344 = CONICAL_SURFACE ( 'NONE', #65560, 0.1000000000000002554, 0.003490658503988666988 ) ;
#84345 = AXIS2_PLACEMENT_3D ( 'NONE', #6810, #74303, #64465 ) ;
#84346 = AXIS2_PLACEMENT_3D ( 'NONE', #77002, #117541, #108391 ) ;
#84347 = CARTESIAN_POINT ( 'NONE',  ( 186.7968750003414300, 8.734944146203032389, 5.348610694689227483E-16 ) ) ;
#84348 = CARTESIAN_POINT ( 'NONE',  ( 6.449999999999928235, 12.50000000000000000, 2.511473670974873507 ) ) ;
#84349 = AXIS2_PLACEMENT_3D ( 'NONE', #50104, #10159, #117495 ) ;
#84350 = PLANE ( 'NONE',  #55271 ) ;
#84351 = VERTEX_POINT ( 'NONE', #3750 ) ;
#84352 = CONICAL_SURFACE ( 'NONE', #17529, 0.09999999999999999167, 0.003490658503988666988 ) ;
#84353 = CARTESIAN_POINT ( 'NONE',  ( -1.650000000000035660, 2.500000000000000000, 2.857883832488649301 ) ) ;
#84354 = EDGE_LOOP ( 'NONE', ( #21740, #25462, #5960, #107698 ) ) ;
#84355 = ORIENTED_EDGE ( 'NONE', *, *, #23064, .T. ) ;
#84356 = EDGE_LOOP ( 'NONE', ( #34860, #16080, #72477, #47523 ) ) ;
#84357 = ORIENTED_EDGE ( 'NONE', *, *, #97466, .F. ) ;
#84358 = DIRECTION ( 'NONE',  ( 0.000000000000000000, -0.000000000000000000, 1.000000000000000000 ) ) ;
#84359 = EDGE_CURVE ( 'NONE', #47322, #35537, #43706, .T. ) ;
#84360 = FACE_BOUND ( 'NONE', #26051, .T. ) ;
#84361 = CARTESIAN_POINT ( 'NONE',  ( 115.5000000000000000, -1.500000000000000222, 1.322875655532295136 ) ) ;
#84363 = ORIENTED_EDGE ( 'NONE', *, *, #40879, .F. ) ;
#84362 = VECTOR ( 'NONE', #97463, 1000.000000000000000 ) ;
#84365 = AXIS2_PLACEMENT_3D ( 'NONE', #71252, #50996, #39888 ) ;
#84364 = DIRECTION ( 'NONE',  ( 0.000000000000000000, 1.000000000000000000, 0.000000000000000000 ) ) ;
#84366 = CARTESIAN_POINT ( 'NONE',  ( 9.999999999999948486, 2.500000000000000000, -4.330127018922201643 ) ) ;
#84367 = ORIENTED_EDGE ( 'NONE', *, *, #56962, .T. ) ;
#84368 = CARTESIAN_POINT ( 'NONE',  ( -4.400000000000028777, 12.50000000000000000, -3.983716857408426293 ) ) ;
#84369 = FACE_OUTER_BOUND ( 'NONE', #59534, .T. ) ;
#84370 = CONICAL_SURFACE ( 'NONE', #119974, 0.1000000000000002554, 0.003490658503988666988 ) ;
#84371 = AXIS2_PLACEMENT_3D ( 'NONE', #74469, #14239, #122932 ) ;
#84372 = EDGE_CURVE ( 'NONE', #44029, #109510, #28771, .T. ) ;
#84373 = AXIS2_PLACEMENT_3D ( 'NONE', #11601, #51548, #1769 ) ;
#84374 = CONICAL_SURFACE ( 'NONE', #101100, 0.1000000000000002554, 0.003490658503988666988 ) ;
#84375 = ORIENTED_EDGE ( 'NONE', *, *, #105688, .T. ) ;
#84376 = CARTESIAN_POINT ( 'NONE',  ( 0.3999999999999559464, 2.500000000000000000, -4.430127018922202176 ) ) ;
#84377 = CARTESIAN_POINT ( 'NONE',  ( 5.649999999999932854, 12.50000000000000000, 1.883746621131358934 ) ) ;
#84379 = EDGE_LOOP ( 'NONE', ( #14490, #31285, #71822, #129326 ) ) ;
#84378 = AXIS2_PLACEMENT_3D ( 'NONE', #51268, #111437, #42078 ) ;
#84380 = DIRECTION ( 'NONE',  ( 0.000000000000000000, 0.000000000000000000, 1.000000000000000000 ) ) ;
#84381 = CARTESIAN_POINT ( 'NONE',  ( 9.399999999999915090, 2.500000000000000000, 3.983716857408420964 ) ) ;
#84382 = CARTESIAN_POINT ( 'NONE',  ( 8.349999999999923261, 2.500000000000000000, 2.165063509461097713 ) ) ;
#84384 = ORIENTED_EDGE ( 'NONE', *, *, #46646, .F. ) ;
#84383 = AXIS2_PLACEMENT_3D ( 'NONE', #64147, #85080, #93616 ) ;
#84385 = EDGE_LOOP ( 'NONE', ( #27203, #66667, #102706, #2275 ) ) ;
#84386 = EDGE_CURVE ( 'NONE', #4566, #38948, #32981, .T. ) ;
#84387 = CARTESIAN_POINT ( 'NONE',  ( 9.599999999999917932, 2.500000000000000000, 0.7928203230275495672 ) ) ;
#84388 = ORIENTED_EDGE ( 'NONE', *, *, #65834, .F. ) ;
#84389 = CARTESIAN_POINT ( 'NONE',  ( -14.14999999999998792, 12.50000000000000000, 2.922977105672690534 ) ) ;
#84390 = DIRECTION ( 'NONE',  ( -0.000000000000000000, -1.000000000000000000, -0.000000000000000000 ) ) ;
#84391 = VERTEX_POINT ( 'NONE', #17915 ) ;
#84392 = DIRECTION ( 'NONE',  ( 0.000000000000000000, 0.000000000000000000, -1.000000000000000000 ) ) ;
#84393 = DIRECTION ( 'NONE',  ( 0.000000000000000000, 0.000000000000000000, -1.000000000000000000 ) ) ;
#84394 = DIRECTION ( 'NONE',  ( 0.000000000000000000, -0.000000000000000000, 1.000000000000000000 ) ) ;
#84395 = DIRECTION ( 'NONE',  ( 1.000000000000000000, -0.000000000000000000, -0.000000000000000000 ) ) ;
#84396 = CARTESIAN_POINT ( 'NONE',  ( -3.550000000000031797, 12.50000000000000000, -6.213873640053564351 ) ) ;
#84397 = CIRCLE ( 'NONE', #80210, 0.06509327318403745899 ) ;
#84398 = ORIENTED_EDGE ( 'NONE', *, *, #103214, .T. ) ;
#84399 = ORIENTED_EDGE ( 'NONE', *, *, #100961, .F. ) ;
#84400 = DIRECTION ( 'NONE',  ( -0.000000000000000000, -1.000000000000000000, -0.000000000000000000 ) ) ;
#84401 = DIRECTION ( 'NONE',  ( 0.000000000000000000, -0.000000000000000000, 1.000000000000000000 ) ) ;
#84402 = DIRECTION ( 'NONE',  ( 0.000000000000000000, -0.9999939076577903929, 0.003490651415223739937 ) ) ;
#84404 = VERTEX_POINT ( 'NONE', #77484 ) ;
#84403 = ORIENTED_EDGE ( 'NONE', *, *, #63330, .F. ) ;
#84405 = ORIENTED_EDGE ( 'NONE', *, *, #45118, .F. ) ;
#84406 = CARTESIAN_POINT ( 'NONE',  ( -3.350000000000028955, 2.500000000000000000, 2.165063509461097713 ) ) ;
#84407 = CIRCLE ( 'NONE', #10936, 0.06509327318403745899 ) ;
#84408 = CIRCLE ( 'NONE', #27975, 0.1000000000000000472 ) ;
#84409 = CARTESIAN_POINT ( 'NONE',  ( 8.099999999999923261, 12.50000000000000000, 4.676537180435972552 ) ) ;
#84410 = CIRCLE ( 'NONE', #15343, 0.06509327318403745899 ) ;
#84411 = FACE_OUTER_BOUND ( 'NONE', #66600, .T. ) ;
#84412 = ADVANCED_FACE ( 'NONE', ( #29053 ), #48043, .T. ) ;
#84413 = FILL_AREA_STYLE ('',( #14367 ) ) ;
#84414 = CARTESIAN_POINT ( 'NONE',  ( 9.599999999999914380, 12.50000000000000000, 3.637306695894644726 ) ) ;
#84415 = DIRECTION ( 'NONE',  ( -4.274815082592931898E-19, -0.9999939076577903929, -0.003490651415223739937 ) ) ;
#84416 = CARTESIAN_POINT ( 'NONE',  ( -0.6000000000000383915, 2.500000000000000000, -4.576537180435977348 ) ) ;
#84417 = CARTESIAN_POINT ( 'NONE',  ( 108.0000000000000142, 8.500000000000000000, -2.249999999999996891 ) ) ;
#84418 = CARTESIAN_POINT ( 'NONE',  ( 8.349999999999919709, 12.50000000000000000, -1.472243186433550122 ) ) ;
#84419 = CIRCLE ( 'NONE', #17505, 0.1000000000000000472 ) ;
#84420 = DIRECTION ( 'NONE',  ( -4.274815082592931898E-19, -0.9999939076577903929, -0.003490651415223739937 ) ) ;
#84421 = VECTOR ( 'NONE', #112264, 1000.000000000000000 ) ;
#84422 = VERTEX_POINT ( 'NONE', #129203 ) ;
#84423 = VECTOR ( 'NONE', #7515, 1000.000000000000000 ) ;
#84424 = PLANE ( 'NONE',  #117582 ) ;
#84425 = EDGE_CURVE ( 'NONE', #3854, #8978, #45500, .T. ) ;
#84426 = ORIENTED_EDGE ( 'NONE', *, *, #62293, .T. ) ;
#84427 = EDGE_CURVE ( 'NONE', #103166, #79180, #83152, .T. ) ;
#84428 = ORIENTED_EDGE ( 'NONE', *, *, #51081, .F. ) ;
#84429 = EDGE_CURVE ( 'NONE', #94365, #118, #57862, .T. ) ;
#84430 = DIRECTION ( 'NONE',  ( 0.000000000000000000, 0.000000000000000000, 1.000000000000000000 ) ) ;
#84433 = ADVANCED_FACE ( 'NONE', ( #127874 ), #68454, .T. ) ;
#84432 = CIRCLE ( 'NONE', #27998, 0.06509327318403745899 ) ;
#84431 = DIRECTION ( 'NONE',  ( 0.000000000000000000, 0.000000000000000000, 1.000000000000000000 ) ) ;
#84434 = CARTESIAN_POINT ( 'NONE',  ( 10.19999999999991047, 12.50000000000000000, 4.611443907251934426 ) ) ;
#84435 = CARTESIAN_POINT ( 'NONE',  ( -12.29999999999999716, 12.50000000000000000, -4.048810130592460865 ) ) ;
#84436 = LINE ( 'NONE', #3301, #100898 ) ;
#84438 = EDGE_CURVE ( 'NONE', #108779, #97111, #74730, .T. ) ;
#84437 = AXIS2_PLACEMENT_3D ( 'NONE', #7373, #77416, #127802 ) ;
#84439 = DIRECTION ( 'NONE',  ( 0.000000000000000000, 0.000000000000000000, 1.000000000000000000 ) ) ;
#84440 = VECTOR ( 'NONE', #108028, 1000.000000000000000 ) ;
#84441 = CONICAL_SURFACE ( 'NONE', #15465, 0.1000000000000002554, 0.003490658503988666988 ) ;
#84442 = CARTESIAN_POINT ( 'NONE',  ( 10.39999999999990976, 2.500000000000000000, -4.330127018922201643 ) ) ;
#84443 = EDGE_LOOP ( 'NONE', ( #76808, #38534 ) ) ;
#84444 = CARTESIAN_POINT ( 'NONE',  ( -4.600000000000024514, 12.50000000000000000, 0.6277270498435120194 ) ) ;
#84445 = CIRCLE ( 'NONE', #96956, 0.09999999999999982514 ) ;
#84446 = EDGE_CURVE ( 'NONE', #4103, #69263, #7815, .T. ) ;
#84447 = CIRCLE ( 'NONE', #21667, 0.06509327318403745899 ) ;
#84449 = EDGE_CURVE ( 'NONE', #1478, #47032, #28399, .T. ) ;
#84448 = DIRECTION ( 'NONE',  ( -0.000000000000000000, -1.000000000000000000, -0.000000000000000000 ) ) ;
#84450 = EDGE_LOOP ( 'NONE', ( #127148, #35645, #14992, #37596 ) ) ;
#84451 = ADVANCED_FACE ( 'NONE', ( #38891 ), #20438, .T. ) ;
#84452 = ORIENTED_EDGE ( 'NONE', *, *, #32359, .F. ) ;
#84453 = EDGE_LOOP ( 'NONE', ( #111816, #127330, #107355, #89712 ) ) ;
#84454 = ORIENTED_EDGE ( 'NONE', *, *, #126904, .F. ) ;
#84455 = EDGE_CURVE ( 'NONE', #18847, #68325, #30837, .T. ) ;
#84456 = DIRECTION ( 'NONE',  ( 0.000000000000000000, 1.000000000000000000, 0.000000000000000000 ) ) ;
#84457 = CARTESIAN_POINT ( 'NONE',  ( -6.850000000000017408, 12.50000000000000000, -6.841600689897077814 ) ) ;
#84458 = DIRECTION ( 'NONE',  ( 0.000000000000000000, 0.000000000000000000, -1.000000000000000000 ) ) ;
#84459 = DIRECTION ( 'NONE',  ( 0.000000000000000000, 0.000000000000000000, -1.000000000000000000 ) ) ;
#84460 = CIRCLE ( 'NONE', #107728, 0.1000000000000002554 ) ;
#84461 = CARTESIAN_POINT ( 'NONE',  ( 13.54999999999989768, 2.500000000000000000, -2.411473670974877859 ) ) ;
#84462 = ORIENTED_EDGE ( 'NONE', *, *, #81030, .T. ) ;
#84464 = VECTOR ( 'NONE', #113739, 1000.000000000000000 ) ;
#84463 = DIRECTION ( 'NONE',  ( -0.000000000000000000, -1.000000000000000000, -0.000000000000000000 ) ) ;
#84465 = AXIS2_PLACEMENT_3D ( 'NONE', #59463, #37851, #126891 ) ;
#84466 = DIRECTION ( 'NONE',  ( 0.000000000000000000, 0.000000000000000000, 1.000000000000000000 ) ) ;
#84467 = LINE ( 'NONE', #36672, #56195 ) ;
#84468 = ORIENTED_EDGE ( 'NONE', *, *, #58219, .F. ) ;
#84469 = CIRCLE ( 'NONE', #11300, 0.06509327318403745899 ) ;
#84470 = AXIS2_PLACEMENT_3D ( 'NONE', #54650, #42281, #52734 ) ;
#84471 = AXIS2_PLACEMENT_3D ( 'NONE', #68359, #118106, #59214 ) ;
#84472 = ORIENTED_EDGE ( 'NONE', *, *, #80438, .F. ) ;
#84473 = AXIS2_PLACEMENT_3D ( 'NONE', #20668, #1651, #52695 ) ;
#84474 = ORIENTED_EDGE ( 'NONE', *, *, #56849, .F. ) ;
#84475 = DIRECTION ( 'NONE',  ( 0.000000000000000000, 1.000000000000000000, 0.000000000000000000 ) ) ;
#84476 = CARTESIAN_POINT ( 'NONE',  ( -1.250000000000035749, 12.50000000000000000, -7.188010851410854052 ) ) ;
#84477 = CARTESIAN_POINT ( 'NONE',  ( 0.000000000000000000, 2.500000000000000000, 0.000000000000000000 ) ) ;
#84478 = CONICAL_SURFACE ( 'NONE', #101205, 0.1000000000000002554, 0.003490658503988666988 ) ;
#84479 = AXIS2_PLACEMENT_3D ( 'NONE', #5354, #87137, #127085 ) ;
#84480 = VECTOR ( 'NONE', #17620, 1000.000000000000000 ) ;
#84481 = ORIENTED_EDGE ( 'NONE', *, *, #57677, .T. ) ;
#84482 = CARTESIAN_POINT ( 'NONE',  ( 3.099999999999945022, 2.500000000000000000, -0.3464101615137783474 ) ) ;
#84483 = DIRECTION ( 'NONE',  ( 0.000000000000000000, 0.000000000000000000, 1.000000000000000000 ) ) ;
#84484 = DIRECTION ( 'NONE',  ( -4.274815082592931898E-19, -0.9999939076577903929, -0.003490651415223739937 ) ) ;
#84485 = CARTESIAN_POINT ( 'NONE',  ( 176.5000000000000000, 0.000000000000000000, -5.000000000000000000 ) ) ;
#84486 = CARTESIAN_POINT ( 'NONE',  ( 4.149999999999941735, 2.500000000000000000, -7.188010851410854052 ) ) ;
#84487 = EDGE_CURVE ( 'NONE', #94071, #23072, #80990, .T. ) ;
#84488 = EDGE_LOOP ( 'NONE', ( #90625, #71095, #28681, #79882 ) ) ;
#84489 = CARTESIAN_POINT ( 'NONE',  ( 105.5000000000000142, 0.000000000000000000, 0.000000000000000000 ) ) ;
#84490 = EDGE_CURVE ( 'NONE', #104091, #1010, #3708, .T. ) ;
#84491 = AXIS2_PLACEMENT_3D ( 'NONE', #89878, #108232, #198 ) ;
#84492 = ORIENTED_EDGE ( 'NONE', *, *, #56890, .F. ) ;
#84493 = ORIENTED_EDGE ( 'NONE', *, *, #59750, .F. ) ;
#84494 = DIRECTION ( 'NONE',  ( -0.000000000000000000, -1.000000000000000000, -0.000000000000000000 ) ) ;
#84495 = DIRECTION ( 'NONE',  ( 0.000000000000000000, 0.000000000000000000, -1.000000000000000000 ) ) ;
#84496 = DIRECTION ( 'NONE',  ( 0.000000000000000000, 0.000000000000000000, -1.000000000000000000 ) ) ;
#84497 = AXIS2_PLACEMENT_3D ( 'NONE', #15522, #96031, #77040 ) ;
#84498 = DIRECTION ( 'NONE',  ( 0.000000000000000000, 0.000000000000000000, 1.000000000000000000 ) ) ;
#84499 = ADVANCED_FACE ( 'NONE', ( #37580 ), #27732, .T. ) ;
#84500 = DIRECTION ( 'NONE',  ( 0.000000000000000000, 0.000000000000000000, -1.000000000000000000 ) ) ;
#84501 = ORIENTED_EDGE ( 'NONE', *, *, #64001, .T. ) ;
#84502 = ORIENTED_EDGE ( 'NONE', *, *, #60104, .F. ) ;
#84503 = DIRECTION ( 'NONE',  ( 0.000000000000000000, 0.000000000000000000, -1.000000000000000000 ) ) ;
#84504 = CARTESIAN_POINT ( 'NONE',  ( 5.599999999999934808, 12.50000000000000000, -4.048810130592463530 ) ) ;
#84505 = CARTESIAN_POINT ( 'NONE',  ( 7.099999999999928590, 2.500000000000000000, -4.330127018922201643 ) ) ;
#84506 = CARTESIAN_POINT ( 'NONE',  ( -10.00000000000000533, 2.500000000000000000, -5.022947341949749678 ) ) ;
#84507 = ORIENTED_EDGE ( 'NONE', *, *, #59895, .T. ) ;
#84508 = CONICAL_SURFACE ( 'NONE', #101231, 0.09999999999999982514, 0.003490658503988666988 ) ;
#84509 = DIRECTION ( 'NONE',  ( 0.000000000000000000, 0.000000000000000000, 1.000000000000000000 ) ) ;
#84510 = DIRECTION ( 'NONE',  ( 0.000000000000000000, 0.000000000000000000, 1.000000000000000000 ) ) ;
#84511 = ORIENTED_EDGE ( 'NONE', *, *, #45706, .F. ) ;
#84512 = CARTESIAN_POINT ( 'NONE',  ( -11.24999999999996447, 12.50000000000000000, -2.230156782645135394 ) ) ;
#84513 = ORIENTED_EDGE ( 'NONE', *, *, #39944, .F. ) ;
#84514 = DIRECTION ( 'NONE',  ( -0.000000000000000000, 1.000000000000000000, -0.000000000000000000 ) ) ;
#84515 = ORIENTED_EDGE ( 'NONE', *, *, #57497, .F. ) ;
#84516 = CARTESIAN_POINT ( 'NONE',  ( -11.69999999999999574, 2.500000000000000000, 4.230127018922196669 ) ) ;
#84517 = LINE ( 'NONE', #35429, #129601 ) ;
#84518 = ORIENTED_EDGE ( 'NONE', *, *, #10020, .F. ) ;
#84519 = ORIENTED_EDGE ( 'NONE', *, *, #39747, .F. ) ;
#84520 = CARTESIAN_POINT ( 'NONE',  ( 186.3385416670080872, 6.551208109652274736, 3.782341765625001351 ) ) ;
#84521 = DIRECTION ( 'NONE',  ( 0.000000000000000000, 0.000000000000000000, -1.000000000000000000 ) ) ;
#84522 = DIRECTION ( 'NONE',  ( 0.000000000000000000, 0.000000000000000000, 1.000000000000000000 ) ) ;
#84523 = CONICAL_SURFACE ( 'NONE', #44832, 0.1000000000000002554, 0.003490658503988666988 ) ;
#84524 = AXIS2_PLACEMENT_3D ( 'NONE', #112043, #81292, #111370 ) ;
#84525 = DIRECTION ( 'NONE',  ( 0.000000000000000000, 1.000000000000000000, 0.000000000000000000 ) ) ;
#84526 = DIRECTION ( 'NONE',  ( -0.000000000000000000, -1.000000000000000000, -0.000000000000000000 ) ) ;
#84527 = CARTESIAN_POINT ( 'NONE',  ( 10.84999999999990905, 2.500000000000000000, -5.802370205355749988 ) ) ;
#84528 = CIRCLE ( 'NONE', #74065, 0.06509327318403745899 ) ;
#84529 = DIRECTION ( 'NONE',  ( 0.000000000000000000, -0.9999939076577903929, 0.003490651415223739937 ) ) ;
#84530 = AXIS2_PLACEMENT_3D ( 'NONE', #16706, #46851, #75635 ) ;
#84531 = EDGE_LOOP ( 'NONE', ( #15395, #99225, #2293, #72350 ) ) ;
#84532 = ORIENTED_EDGE ( 'NONE', *, *, #40689, .T. ) ;
#84533 = DIRECTION ( 'NONE',  ( 0.000000000000000000, 1.000000000000000000, 0.000000000000000000 ) ) ;
#84534 = CARTESIAN_POINT ( 'NONE',  ( -2.700000000000029932, 2.500000000000000000, -0.3464101615137782364 ) ) ;
#84535 = LINE ( 'NONE', #102872, #72174 ) ;
#84536 = ADVANCED_FACE ( 'NONE', ( #79440 ), #128554, .T. ) ;
#84537 = DIRECTION ( 'NONE',  ( 0.000000000000000000, 1.000000000000000000, 0.000000000000000000 ) ) ;
#84539 = ORIENTED_EDGE ( 'NONE', *, *, #102634, .F. ) ;
#84538 = ORIENTED_EDGE ( 'NONE', *, *, #105157, .T. ) ;
#84540 = DIRECTION ( 'NONE',  ( -0.000000000000000000, -1.000000000000000000, -0.000000000000000000 ) ) ;
#84541 = ORIENTED_EDGE ( 'NONE', *, *, #1351, .F. ) ;
#84542 = ADVANCED_FACE ( 'NONE', ( #49990 ), #24553, .T. ) ;
#84543 = CARTESIAN_POINT ( 'NONE',  ( 8.549999999999920774, 2.500000000000000000, 6.248780366869521430 ) ) ;
#84544 = DIRECTION ( 'NONE',  ( 0.000000000000000000, 0.000000000000000000, -1.000000000000000000 ) ) ;
#84545 = VERTEX_POINT ( 'NONE', #15491 ) ;
#84546 = CARTESIAN_POINT ( 'NONE',  ( 7.499999999999923617, 12.50000000000000000, 0.6928203230275494784 ) ) ;
#84547 = DIRECTION ( 'NONE',  ( 0.000000000000000000, 0.000000000000000000, 1.000000000000000000 ) ) ;
#84548 = DIRECTION ( 'NONE',  ( -0.000000000000000000, -1.000000000000000000, -0.000000000000000000 ) ) ;
#84550 = CARTESIAN_POINT ( 'NONE',  ( -8.950000000000008171, 12.50000000000000000, 1.753560074763284016 ) ) ;
#84549 = VECTOR ( 'NONE', #31479, 1000.000000000000000 ) ;
#84551 = AXIS2_PLACEMENT_3D ( 'NONE', #4396, #113092, #23416 ) ;
#84552 = DIRECTION ( 'NONE',  ( -0.000000000000000000, -1.000000000000000000, -0.000000000000000000 ) ) ;
#84553 = DIRECTION ( 'NONE',  ( 0.000000000000000000, -0.9999939076577903929, 0.003490651415223739937 ) ) ;
#84554 = AXIS2_PLACEMENT_3D ( 'NONE', #82844, #82181, #52715 ) ;
#84555 = EDGE_CURVE ( 'NONE', #12752, #9105, #129131, .T. ) ;
#84556 = DIRECTION ( 'NONE',  ( 0.000000000000000000, 0.000000000000000000, 1.000000000000000000 ) ) ;
#84557 = FACE_OUTER_BOUND ( 'NONE', #54982, .T. ) ;
#84558 = LINE ( 'NONE', #45935, #22238 ) ;
#84560 = EDGE_LOOP ( 'NONE', ( #85289, #70251, #122634, #7343 ) ) ;
#84559 = AXIS2_PLACEMENT_3D ( 'NONE', #7127, #28079, #67987 ) ;
#84561 = VERTEX_POINT ( 'NONE', #81995 ) ;
#84562 = ORIENTED_EDGE ( 'NONE', *, *, #91212, .T. ) ;
#84563 = DIRECTION ( 'NONE',  ( -0.000000000000000000, 1.000000000000000000, -0.000000000000000000 ) ) ;
#84564 = ORIENTED_EDGE ( 'NONE', *, *, #71309, .F. ) ;
#84565 = DIRECTION ( 'NONE',  ( -0.000000000000000000, 1.000000000000000000, -0.000000000000000000 ) ) ;
#84567 = EDGE_LOOP ( 'NONE', ( #26778, #18803, #14598, #47508 ) ) ;
#84566 = VERTEX_POINT ( 'NONE', #62376 ) ;
#84568 = VERTEX_POINT ( 'NONE', #61069 ) ;
#84569 = CARTESIAN_POINT ( 'NONE',  ( -5.600000000000020073, 2.500000000000000000, 3.983716857408420964 ) ) ;
#84570 = CONICAL_SURFACE ( 'NONE', #103450, 0.09999999999999999167, 0.003490658503988666988 ) ;
#84571 = DIRECTION ( 'NONE',  ( 0.000000000000000000, 0.000000000000000000, 1.000000000000000000 ) ) ;
#84572 = EDGE_CURVE ( 'NONE', #128871, #55439, #58014, .T. ) ;
#84573 = CARTESIAN_POINT ( 'NONE',  ( 12.89999999999989733, 12.50000000000000000, -2.385244779468109755E-15 ) ) ;
#84574 = CARTESIAN_POINT ( 'NONE',  ( -8.350000000000013856, 2.500000000000000000, -2.065063509461102065 ) ) ;
#84575 = AXIS2_PLACEMENT_3D ( 'NONE', #77046, #58062, #97965 ) ;
#84576 = CARTESIAN_POINT ( 'NONE',  ( -6.900000000000019007, 2.500000000000000000, -0.2464101615137783419 ) ) ;
#84577 = ORIENTED_EDGE ( 'NONE', *, *, #38627, .T. ) ;
#84578 = DIRECTION ( 'NONE',  ( 0.000000000000000000, 0.000000000000000000, -1.000000000000000000 ) ) ;
#84579 = ORIENTED_EDGE ( 'NONE', *, *, #104284, .F. ) ;
#84580 = EDGE_CURVE ( 'NONE', #35226, #97598, #21142, .T. ) ;
#84581 = ORIENTED_EDGE ( 'NONE', *, *, #80139, .T. ) ;
#84582 = EDGE_LOOP ( 'NONE', ( #104894, #69905 ) ) ;
#84583 = DIRECTION ( 'NONE',  ( 0.000000000000000000, 1.000000000000000000, 0.000000000000000000 ) ) ;
#84584 =( BOUNDED_SURFACE ( )  B_SPLINE_SURFACE ( 1, 2, ( 
 ( #110515, #80425, #28092, #38580, #50970, #77821, #120347, #68008, #78503, #127582, #117734, #109212, #69283, #60778, #89592, #129543, #548, #58215, #39235, #8432, #118397, #37905, #40513, #28747, #79141, #107934, #98110, #19558, #9089, #48375, #60153, #90211, #88271, #108583, #119054, #18900, #128242, #109880, #58841, #79766, #98749, #9739, #49041, #119680, #59516, #30688, #99426, #30038, #100680, #100058, #29394, #10382, #69955, #20207, #70595, #11008, #90874, #62720, #14232, #111137, #1204, #103283, #13588, #51610, #83005, #113750, #101993, #92823, #41802, #82365, #102618, #33886, #43096, #71895, #22162, #122925, #12938, #24075, #81693, #12306, #61437, #32637, #73803, #43735, #121612 ),
 ( #21491, #22804, #11667, #31972, #41156, #120982, #62074, #42434, #33268, #52248, #122284, #113087, #63994, #103921, #101351, #92157, #123542, #73173, #81068, #72539, #23412, #31331, #71228, #53540, #91524, #2475, #3151, #1841, #111817, #112464, #63352, #83643, #52889, #93453, #3786, #46277, #27279, #15520, #37122, #77037, #5061, #14858, #26650, #6327, #96651, #65916, #36489, #54803, #67177, #24719, #55466, #45009, #86184, #35195, #107122, #76398, #26011, #116297, #105851, #115656, #56718, #74461, #125486, #86848, #95388, #66556, #5699, #116939, #6974, #84269, #94734, #54182, #4393, #35823, #75733, #94098, #16151, #56094, #46948, #114371, #45655, #64632, #84919, #44345, #126786 ) ),
 .UNSPECIFIED., .F., .F., .F. ) 
 B_SPLINE_SURFACE_WITH_KNOTS ( ( 2, 2 ),
 ( 3, 2, 2, 2, 2, 2, 2, 2, 2, 2, 2, 2, 2, 2, 2, 2, 2, 2, 2, 2, 2, 2, 2, 2, 2, 2, 2, 2, 2, 2, 2, 2, 2, 2, 2, 2, 2, 2, 2, 2, 2, 2, 3 ),
 ( 0.000000000000000000, 1.000000000000000000 ),
 ( 0.000000000000000000, 0.02380952380952380820, 0.04761904761904761640, 0.07142857142857142461, 0.09523809523809523281, 0.1190476190476190410, 0.1428571428571428492, 0.1666666666666666574, 0.1904761904761904656, 0.2142857142857142738, 0.2380952380952380820, 0.2619047619047619180, 0.2857142857142856984, 0.3095238095238095344, 0.3333333333333333148, 0.3571428571428571508, 0.3809523809523809312, 0.4047619047619047672, 0.4285714285714285476, 0.4523809523809523836, 0.4761904761904761640, 0.5000000000000000000, 0.5238095238095238360, 0.5476190476190476719, 0.5714285714285713969, 0.5952380952380952328, 0.6190476190476190688, 0.6428571428571429047, 0.6666666666666666297, 0.6904761904761904656, 0.7142857142857143016, 0.7380952380952381375, 0.7619047619047618625, 0.7857142857142856984, 0.8095238095238095344, 0.8333333333333333703, 0.8571428571428570953, 0.8809523809523809312, 0.9047619047619047672, 0.9285714285714286031, 0.9523809523809523281, 0.9761904761904761640, 1.000000000000000000 ),
 .UNSPECIFIED. ) 
 GEOMETRIC_REPRESENTATION_ITEM ( )  RATIONAL_B_SPLINE_SURFACE ( (
 ( 1.000000000000000000, 0.8660254037844387076, 1.000000000000000000, 0.8660254037844387076, 1.000000000000000000, 0.8660254037844387076, 1.000000000000000000, 0.8660254037844387076, 1.000000000000000000, 0.8660254037844387076, 1.000000000000000000, 0.8660254037844387076, 1.000000000000000000, 0.8660254037844387076, 1.000000000000000000, 0.8660254037844387076, 1.000000000000000000, 0.8660254037844387076, 1.000000000000000000, 0.8660254037844387076, 1.000000000000000000, 0.8660254037844387076, 1.000000000000000000, 0.8660254037844387076, 1.000000000000000000, 0.8660254037844387076, 1.000000000000000000, 0.8660254037844387076, 1.000000000000000000, 0.8660254037844387076, 1.000000000000000000, 0.8660254037844387076, 1.000000000000000000, 0.8660254037844387076, 1.000000000000000000, 0.8660254037844387076, 1.000000000000000000, 0.8660254037844387076, 1.000000000000000000, 0.8660254037844387076, 1.000000000000000000, 0.8660254037844387076, 1.000000000000000000, 0.8660254037844387076, 1.000000000000000000, 0.8660254037844387076, 1.000000000000000000, 0.8660254037844387076, 1.000000000000000000, 0.8660254037844387076, 1.000000000000000000, 0.8660254037844387076, 1.000000000000000000, 0.8660254037844387076, 1.000000000000000000, 0.8660254037844387076, 1.000000000000000000, 0.8660254037844387076, 1.000000000000000000, 0.8660254037844387076, 1.000000000000000000, 0.8660254037844387076, 1.000000000000000000, 0.8660254037844387076, 1.000000000000000000, 0.8660254037844387076, 1.000000000000000000, 0.8660254037844387076, 1.000000000000000000, 0.8660254037844387076, 1.000000000000000000, 0.8660254037844387076, 1.000000000000000000, 0.8660254037844387076, 1.000000000000000000, 0.8660254037844387076, 1.000000000000000000, 0.8660254037844387076, 1.000000000000000000, 0.8660254037844387076, 1.000000000000000000, 0.8660254037844387076, 1.000000000000000000, 0.8660254037844387076, 1.000000000000000000),
 ( 1.000000000000000000, 0.8660254037844387076, 1.000000000000000000, 0.8660254037844387076, 1.000000000000000000, 0.8660254037844387076, 1.000000000000000000, 0.8660254037844387076, 1.000000000000000000, 0.8660254037844387076, 1.000000000000000000, 0.8660254037844387076, 1.000000000000000000, 0.8660254037844387076, 1.000000000000000000, 0.8660254037844387076, 1.000000000000000000, 0.8660254037844387076, 1.000000000000000000, 0.8660254037844387076, 1.000000000000000000, 0.8660254037844387076, 1.000000000000000000, 0.8660254037844387076, 1.000000000000000000, 0.8660254037844387076, 1.000000000000000000, 0.8660254037844387076, 1.000000000000000000, 0.8660254037844387076, 1.000000000000000000, 0.8660254037844387076, 1.000000000000000000, 0.8660254037844387076, 1.000000000000000000, 0.8660254037844387076, 1.000000000000000000, 0.8660254037844387076, 1.000000000000000000, 0.8660254037844387076, 1.000000000000000000, 0.8660254037844387076, 1.000000000000000000, 0.8660254037844387076, 1.000000000000000000, 0.8660254037844387076, 1.000000000000000000, 0.8660254037844387076, 1.000000000000000000, 0.8660254037844387076, 1.000000000000000000, 0.8660254037844387076, 1.000000000000000000, 0.8660254037844387076, 1.000000000000000000, 0.8660254037844387076, 1.000000000000000000, 0.8660254037844387076, 1.000000000000000000, 0.8660254037844387076, 1.000000000000000000, 0.8660254037844387076, 1.000000000000000000, 0.8660254037844387076, 1.000000000000000000, 0.8660254037844387076, 1.000000000000000000, 0.8660254037844387076, 1.000000000000000000, 0.8660254037844387076, 1.000000000000000000, 0.8660254037844387076, 1.000000000000000000, 0.8660254037844387076, 1.000000000000000000, 0.8660254037844387076, 1.000000000000000000, 0.8660254037844387076, 1.000000000000000000, 0.8660254037844387076, 1.000000000000000000, 0.8660254037844387076, 1.000000000000000000, 0.8660254037844387076, 1.000000000000000000) ) ) 
 REPRESENTATION_ITEM ( '' )  SURFACE ( )  );
#84585 = EDGE_CURVE ( 'NONE', #47459, #37524, #120637, .T. ) ;
#84586 = ORIENTED_EDGE ( 'NONE', *, *, #114404, .T. ) ;
#84587 = EDGE_CURVE ( 'NONE', #4707, #85507, #16209, .T. ) ;
#84588 = ORIENTED_EDGE ( 'NONE', *, *, #36327, .T. ) ;
#84589 = EDGE_CURVE ( 'NONE', #93106, #111188, #51751, .T. ) ;
#84590 = EDGE_LOOP ( 'NONE', ( #83256, #112251, #118988, #107399 ) ) ;
#84591 = EDGE_CURVE ( 'NONE', #74727, #103978, #12020, .T. ) ;
#84592 = VECTOR ( 'NONE', #44691, 1000.000000000000000 ) ;
#84593 = DIRECTION ( 'NONE',  ( -0.000000000000000000, 1.000000000000000000, -0.000000000000000000 ) ) ;
#84594 = CARTESIAN_POINT ( 'NONE',  ( -13.74999999999995381, 12.50000000000000000, 2.099970236277064028 ) ) ;
#84595 = CARTESIAN_POINT ( 'NONE',  ( 2.699999999999947331, 12.50000000000000000, -0.2813168883297409439 ) ) ;
#84596 = DIRECTION ( 'NONE',  ( 0.000000000000000000, 0.000000000000000000, 1.000000000000000000 ) ) ;
#84597 = EDGE_CURVE ( 'NONE', #72456, #40560, #66491, .T. ) ;
#84598 = CARTESIAN_POINT ( 'NONE',  ( 11.24999999999991118, 12.50000000000000000, 5.802370205355744659 ) ) ;
#84599 = EDGE_LOOP ( 'NONE', ( #82023, #53838, #67982, #61967 ) ) ;
#84600 = ADVANCED_FACE ( 'NONE', ( #92458 ), #81091, .T. ) ;
#84601 = DIRECTION ( 'NONE',  ( 0.000000000000000000, 1.000000000000000000, 0.000000000000000000 ) ) ;
#84602 = AXIS2_PLACEMENT_3D ( 'NONE', #17383, #97252, #47521 ) ;
#84603 = AXIS2_PLACEMENT_3D ( 'NONE', #17528, #86916, #124921 ) ;
#84604 = ADVANCED_FACE ( 'NONE', ( #864 ), #56024, .T. ) ;
#84605 = ORIENTED_EDGE ( 'NONE', *, *, #17149, .F. ) ;
#84606 = DIRECTION ( 'NONE',  ( 0.000000000000000000, 0.000000000000000000, -1.000000000000000000 ) ) ;
#84607 = ADVANCED_FACE ( 'NONE', ( #70252 ), #89487, .T. ) ;
#84608 = ORIENTED_EDGE ( 'NONE', *, *, #9213, .T. ) ;
#84609 = ORIENTED_EDGE ( 'NONE', *, *, #61176, .F. ) ;
#84610 = VERTEX_POINT ( 'NONE', #111447 ) ;
#84611 = EDGE_CURVE ( 'NONE', #41152, #10139, #16304, .T. ) ;
#84612 = CARTESIAN_POINT ( 'NONE',  ( 12.09999999999990195, 12.50000000000000000, -0.6928203230275541413 ) ) ;
#84613 = DIRECTION ( 'NONE',  ( 0.000000000000000000, 1.000000000000000000, 0.000000000000000000 ) ) ;
#84614 = CONICAL_SURFACE ( 'NONE', #40717, 0.1000000000000000472, 0.003490658503988666988 ) ;
#84615 = CARTESIAN_POINT ( 'NONE',  ( 6.249999999999930722, 2.500000000000000000, 7.188010851410848723 ) ) ;
#84616 = CIRCLE ( 'NONE', #36512, 0.1000000000000000472 ) ;
#84617 = ORIENTED_EDGE ( 'NONE', *, *, #91078, .T. ) ;
#84618 = CARTESIAN_POINT ( 'NONE',  ( 5.199999999999933564, 2.500000000000000000, 4.083716857408420609 ) ) ;
#84619 = ORIENTED_EDGE ( 'NONE', *, *, #53512, .T. ) ;
#84620 = DIRECTION ( 'NONE',  ( 0.000000000000000000, 1.000000000000000000, 0.000000000000000000 ) ) ;
#84621 = CARTESIAN_POINT ( 'NONE',  ( -1.850000000000033396, 2.500000000000000000, -1.718653347947325827 ) ) ;
#84622 = CARTESIAN_POINT ( 'NONE',  ( 6.649999999999927525, 2.500000000000000000, 2.065063509461097624 ) ) ;
#84623 = CARTESIAN_POINT ( 'NONE',  ( -12.49999999999995737, 12.50000000000000000, 4.265033745738159077 ) ) ;
#84624 = CARTESIAN_POINT ( 'NONE',  ( -10.45000000000000107, 12.50000000000000000, 2.099970236277060032 ) ) ;
#84625 = ORIENTED_EDGE ( 'NONE', *, *, #118549, .T. ) ;
#84626 = AXIS2_PLACEMENT_3D ( 'NONE', #74369, #11081, #90280 ) ;
#84627 = AXIS2_PLACEMENT_3D ( 'NONE', #48815, #69073, #28520 ) ;
#84628 = ORIENTED_EDGE ( 'NONE', *, *, #11719, .T. ) ;
#84629 = CIRCLE ( 'NONE', #101062, 0.1000000000000002554 ) ;
#84630 = EDGE_LOOP ( 'NONE', ( #128047, #23955, #73229, #109542 ) ) ;
#84631 = VECTOR ( 'NONE', #19294, 1000.000000000000000 ) ;
#84632 = DIRECTION ( 'NONE',  ( 0.000000000000000000, -1.000000000000000000, 0.000000000000000000 ) ) ;
#84633 = DIRECTION ( 'NONE',  ( 0.000000000000000000, 0.000000000000000000, 1.000000000000000000 ) ) ;
#84634 = CARTESIAN_POINT ( 'NONE',  ( 185.2135416670080872, 4.367472073101518859, -7.564683531249999149 ) ) ;
#84635 = DIRECTION ( 'NONE',  ( -4.274815082592931898E-19, -0.9999939076577903929, -0.003490651415223739937 ) ) ;
#84636 = CARTESIAN_POINT ( 'NONE',  ( 7.699999999999923794, 2.500000000000000000, 4.676537180435972552 ) ) ;
#84637 = LINE ( 'NONE', #122632, #4209 ) ;
#84638 = CARTESIAN_POINT ( 'NONE',  ( 8.099999999999923261, 2.500000000000000000, 3.983716857408420076 ) ) ;
#84639 = EDGE_LOOP ( 'NONE', ( #82599, #100465, #12677, #125303 ) ) ;
#84640 = EDGE_CURVE ( 'NONE', #97955, #56748, #43385, .T. ) ;
#84642 = DIRECTION ( 'NONE',  ( 0.000000000000000000, 0.000000000000000000, 1.000000000000000000 ) ) ;
#84641 = CIRCLE ( 'NONE', #49156, 0.09999999999999982514 ) ;
#84643 = CARTESIAN_POINT ( 'NONE',  ( -0.2000000000000399791, 2.500000000000000000, -4.676537180435977881 ) ) ;
#84644 = CONICAL_SURFACE ( 'NONE', #19802, 0.1000000000000002554, 0.003490658503988666988 ) ;
#84645 = ADVANCED_FACE ( 'NONE', ( #32928 ), #124993, .T. ) ;
#84646 = ORIENTED_EDGE ( 'NONE', *, *, #14795, .T. ) ;
#84647 = CIRCLE ( 'NONE', #47003, 0.06509327318403741736 ) ;
#84648 = DIRECTION ( 'NONE',  ( 0.000000000000000000, 0.000000000000000000, 1.000000000000000000 ) ) ;
#84649 = AXIS2_PLACEMENT_3D ( 'NONE', #115640, #56706, #114360 ) ;
#84650 = EDGE_LOOP ( 'NONE', ( #107826, #23382, #21680, #25391 ) ) ;
#84651 = AXIS2_PLACEMENT_3D ( 'NONE', #8746, #48704, #38907 ) ;
#84652 = DIRECTION ( 'NONE',  ( 0.000000000000000000, -0.000000000000000000, 1.000000000000000000 ) ) ;
#84653 = CIRCLE ( 'NONE', #124376, 0.1000000000000000472 ) ;
#84654 = VERTEX_POINT ( 'NONE', #3437 ) ;
#84655 = DIRECTION ( 'NONE',  ( 0.000000000000000000, 0.000000000000000000, 1.000000000000000000 ) ) ;
#84656 = CARTESIAN_POINT ( 'NONE',  ( -2.050000000000033129, 12.50000000000000000, 2.165063509461097713 ) ) ;
#84657 = CARTESIAN_POINT ( 'NONE',  ( -7.900000000000011013, 2.500000000000000000, 4.922947341949748257 ) ) ;
#84658 = EDGE_LOOP ( 'NONE', ( #64739, #61638, #56801, #77453 ) ) ;
#84659 = AXIS2_PLACEMENT_3D ( 'NONE', #88110, #77038, #87482 ) ;
#84660 = AXIS2_PLACEMENT_3D ( 'NONE', #101770, #23193, #63125 ) ;
#84661 = CARTESIAN_POINT ( 'NONE',  ( 185.5312500006828031, 9.429780353434619030E-16, -7.700000000000000178 ) ) ;
#84662 = DIRECTION ( 'NONE',  ( 0.000000000000000000, 0.000000000000000000, 1.000000000000000000 ) ) ;
#84663 = ORIENTED_EDGE ( 'NONE', *, *, #4075, .T. ) ;
#84664 = CARTESIAN_POINT ( 'NONE',  ( 5.649999999999936406, 2.500000000000000000, -6.148780366869526226 ) ) ;
#84665 = ORIENTED_EDGE ( 'NONE', *, *, #118114, .T. ) ;
#84666 = ORIENTED_EDGE ( 'NONE', *, *, #39437, .T. ) ;
#84667 = CARTESIAN_POINT ( 'NONE',  ( 1.849999999999948130, 12.50000000000000000, 6.213873640053558134 ) ) ;
#84668 = DIRECTION ( 'NONE',  ( 0.000000000000000000, 0.000000000000000000, -1.000000000000000000 ) ) ;
#84669 = VERTEX_POINT ( 'NONE', #82660 ) ;
#84670 = DIRECTION ( 'NONE',  ( 0.000000000000000000, -0.000000000000000000, 1.000000000000000000 ) ) ;
#84671 = DIRECTION ( 'NONE',  ( 0.000000000000000000, 1.000000000000000000, 0.000000000000000000 ) ) ;
#84672 = AXIS2_PLACEMENT_3D ( 'NONE', #71487, #111401, #49306 ) ;
#84673 = VERTEX_POINT ( 'NONE', #112760 ) ;
#84675 = ADVANCED_FACE ( 'NONE', ( #20514 ), #37273, .T. ) ;
#84674 = DIRECTION ( 'NONE',  ( 0.000000000000000000, 0.000000000000000000, 1.000000000000000000 ) ) ;
#84676 = FACE_OUTER_BOUND ( 'NONE', #93604, .T. ) ;
#84677 = FACE_OUTER_BOUND ( 'NONE', #61097, .T. ) ;
#84678 = CARTESIAN_POINT ( 'NONE',  ( 17.49862860983166257, -2.500000000000000000, -4.081131818001380474 ) ) ;
#84679 = FACE_OUTER_BOUND ( 'NONE', #34519, .T. ) ;
#84680 = PLANE ( 'NONE',  #5439 ) ;
#84681 = DIRECTION ( 'NONE',  ( 0.000000000000000000, 0.000000000000000000, 1.000000000000000000 ) ) ;
#84682 = CIRCLE ( 'NONE', #82554, 0.06509327318403745899 ) ;
#84683 = CONICAL_SURFACE ( 'NONE', #24149, 0.09999999999999982514, 0.003490658503988666988 ) ;
#84684 = ORIENTED_EDGE ( 'NONE', *, *, #116327, .F. ) ;
#84685 = VERTEX_POINT ( 'NONE', #10653 ) ;
#84686 = ORIENTED_EDGE ( 'NONE', *, *, #24187, .T. ) ;
#84687 = VERTEX_POINT ( 'NONE', #50599 ) ;
#84688 = CARTESIAN_POINT ( 'NONE',  ( 21.23528140090950700, 2.699413673072311948, 2.293764360948889802 ) ) ;
#84689 = DIRECTION ( 'NONE',  ( 0.000000000000000000, 0.000000000000000000, 1.000000000000000000 ) ) ;
#84690 = ADVANCED_FACE ( 'NONE', ( #31621 ), #23085, .T. ) ;
#84691 = DIRECTION ( 'NONE',  ( 0.000000000000000000, 0.000000000000000000, 1.000000000000000000 ) ) ;
#84692 = ORIENTED_EDGE ( 'NONE', *, *, #6701, .F. ) ;
#84693 = FACE_BOUND ( 'NONE', #55912, .T. ) ;
#84694 = ADVANCED_FACE ( 'NONE', ( #105514 ), #110407, .T. ) ;
#84695 = CARTESIAN_POINT ( 'NONE',  ( 12.49999999999990585, 12.50000000000000000, -5.022947341949754119 ) ) ;
#84696 = CARTESIAN_POINT ( 'NONE',  ( -7.950000000000009059, 12.50000000000000000, 6.495190528383297135 ) ) ;
#84697 = AXIS2_PLACEMENT_3D ( 'NONE', #49896, #61641, #89798 ) ;
#84698 = CARTESIAN_POINT ( 'NONE',  ( -2.900000000000030109, 2.500000000000000000, 0.7928203230275495672 ) ) ;
#84699 = DIRECTION ( 'NONE',  ( -4.274815082592931898E-19, -0.9999939076577903929, -0.003490651415223739937 ) ) ;
#84700 = CONICAL_SURFACE ( 'NONE', #24072, 0.1000000000000000472, 0.003490658503988666988 ) ;
#84701 = FACE_OUTER_BOUND ( 'NONE', #67567, .T. ) ;
#84702 = CARTESIAN_POINT ( 'NONE',  ( -10.40000000000000213, 2.500000000000000000, 0.6928203230275494784 ) ) ;
#84703 = DIRECTION ( 'NONE',  ( 0.000000000000000000, 1.000000000000000000, 0.000000000000000000 ) ) ;
#84704 = CARTESIAN_POINT ( 'NONE',  ( 3.149999999999946176, 2.500000000000000000, -6.248780366869526759 ) ) ;
#84705 = ADVANCED_FACE ( 'NONE', ( #34855 ), #1647, .T. ) ;
#84706 = DIRECTION ( 'NONE',  ( 0.000000000000000000, 0.000000000000000000, -1.000000000000000000 ) ) ;
#84707 = CARTESIAN_POINT ( 'NONE',  ( -6.050000000000022027, 2.500000000000000000, -1.718653347947326049 ) ) ;
#84708 = AXIS2_PLACEMENT_3D ( 'NONE', #128658, #118157, #120736 ) ;
#84709 = VERTEX_POINT ( 'NONE', #15824 ) ;
#84710 = ORIENTED_EDGE ( 'NONE', *, *, #121225, .T. ) ;
#84711 = VECTOR ( 'NONE', #117345, 1000.000000000000000 ) ;
#84712 = EDGE_LOOP ( 'NONE', ( #10952, #45630, #120825, #69930 ) ) ;
#84713 = EDGE_LOOP ( 'NONE', ( #46326, #88168, #65712, #95405 ) ) ;
#84714 = DIRECTION ( 'NONE',  ( 0.000000000000000000, 1.000000000000000000, 0.000000000000000000 ) ) ;
#84715 = ORIENTED_EDGE ( 'NONE', *, *, #11944, .T. ) ;
#84716 = DIRECTION ( 'NONE',  ( 0.000000000000000000, 0.000000000000000000, 1.000000000000000000 ) ) ;
#84717 = ORIENTED_EDGE ( 'NONE', *, *, #72761, .F. ) ;
#84718 = EDGE_LOOP ( 'NONE', ( #122047, #101291, #10109, #117310 ) ) ;
#84719 = AXIS2_PLACEMENT_3D ( 'NONE', #103243, #43702, #113049 ) ;
#84720 = LINE ( 'NONE', #35634, #78981 ) ;
#84721 = DIRECTION ( 'NONE',  ( 0.000000000000000000, 0.000000000000000000, 1.000000000000000000 ) ) ;
#84722 = CARTESIAN_POINT ( 'NONE',  ( -8.100000000000013856, 12.50000000000000000, -0.4115034346978156399 ) ) ;
#84723 = CARTESIAN_POINT ( 'NONE',  ( 0.8499999999999536815, 12.50000000000000000, 5.867463478539781896 ) ) ;
#84724 = ORIENTED_EDGE ( 'NONE', *, *, #64887, .F. ) ;
#84725 = ORIENTED_EDGE ( 'NONE', *, *, #25035, .T. ) ;
#84726 = EDGE_CURVE ( 'NONE', #3657, #44118, #87324, .T. ) ;
#84728 = EDGE_LOOP ( 'NONE', ( #63006, #44211 ) ) ;
#84727 = AXIS2_PLACEMENT_3D ( 'NONE', #89377, #120124, #30472 ) ;
#84730 = ORIENTED_EDGE ( 'NONE', *, *, #53365, .T. ) ;
#84729 = DIRECTION ( 'NONE',  ( 0.000000000000000000, 1.000000000000000000, 0.000000000000000000 ) ) ;
#84731 = CIRCLE ( 'NONE', #76330, 0.1000000000000002554 ) ;
#84732 = CIRCLE ( 'NONE', #76331, 0.1000000000000002554 ) ;
#84733 = CARTESIAN_POINT ( 'NONE',  ( 3.749999999999976907, 2.500000000000000000, 2.165063509461097713 ) ) ;
#84734 = ORIENTED_EDGE ( 'NONE', *, *, #14231, .T. ) ;
#84735 = EDGE_CURVE ( 'NONE', #120064, #6156, #4074, .T. ) ;
#84736 = VERTEX_POINT ( 'NONE', #5360 ) ;
#84737 = EDGE_CURVE ( 'NONE', #20333, #98360, #85850, .T. ) ;
#84738 = CARTESIAN_POINT ( 'NONE',  ( -10.60000000000000320, 2.500000000000000000, -4.576537180435972907 ) ) ;
#84739 = AXIS2_PLACEMENT_3D ( 'NONE', #47903, #87798, #127109 ) ;
#84740 = CIRCLE ( 'NONE', #109790, 2.000000000000000000 ) ;
#84741 = CONICAL_SURFACE ( 'NONE', #117895, 0.09999999999999982514, 0.003490658503988666988 ) ;
#84742 = DIRECTION ( 'NONE',  ( -0.000000000000000000, -1.000000000000000000, -0.000000000000000000 ) ) ;
#84743 = CARTESIAN_POINT ( 'NONE',  ( -1.900000000000035438, 2.500000000000000000, 3.983716857408420076 ) ) ;
#84744 = CARTESIAN_POINT ( 'NONE',  ( -8.749999999999975131, 2.500000000000000000, 2.165063509461097713 ) ) ;
#84745 = EDGE_CURVE ( 'NONE', #61621, #19851, #45312, .T. ) ;
#84746 = AXIS2_PLACEMENT_3D ( 'NONE', #80938, #59384, #81569 ) ;
#84747 = EDGE_CURVE ( 'NONE', #47889, #22314, #74821, .T. ) ;
#84748 = FACE_OUTER_BOUND ( 'NONE', #1699, .T. ) ;
#84749 = EDGE_CURVE ( 'NONE', #39552, #64505, #60268, .T. ) ;
#84750 = EDGE_CURVE ( 'NONE', #44501, #105738, #103586, .T. ) ;
#84751 = ORIENTED_EDGE ( 'NONE', *, *, #3046, .F. ) ;
#84752 = CARTESIAN_POINT ( 'NONE',  ( -11.44999999999999751, 12.50000000000000000, 6.906693963081109722 ) ) ;
#84753 = AXIS2_PLACEMENT_3D ( 'NONE', #95243, #65110, #92657 ) ;
#84754 = AXIS2_PLACEMENT_3D ( 'NONE', #128526, #29018, #38859 ) ;
#84755 = ORIENTED_EDGE ( 'NONE', *, *, #118049, .F. ) ;
#84756 = DIRECTION ( 'NONE',  ( 0.000000000000000000, -0.000000000000000000, 1.000000000000000000 ) ) ;
#84757 = AXIS2_PLACEMENT_3D ( 'NONE', #89238, #81988, #60449 ) ;
#84758 = EDGE_CURVE ( 'NONE', #117920, #53276, #99954, .T. ) ;
#84759 = VERTEX_POINT ( 'NONE', #46576 ) ;
#84760 = DIRECTION ( 'NONE',  ( 0.000000000000000000, 0.000000000000000000, 1.000000000000000000 ) ) ;
#84761 = CARTESIAN_POINT ( 'NONE',  ( -0.8500000000000395017, 2.500000000000000000, 2.265063509461097357 ) ) ;
#84762 = AXIS2_PLACEMENT_3D ( 'NONE', #103459, #15696, #13770 ) ;
#84763 = DIRECTION ( 'NONE',  ( 0.000000000000000000, -0.000000000000000000, 1.000000000000000000 ) ) ;
#84764 = DIRECTION ( 'NONE',  ( -0.000000000000000000, 1.000000000000000000, -0.000000000000000000 ) ) ;
#84765 = ORIENTED_EDGE ( 'NONE', *, *, #107531, .T. ) ;
#84766 = EDGE_CURVE ( 'NONE', #91186, #122791, #76969, .T. ) ;
#84767 = PRESENTATION_STYLE_ASSIGNMENT (( #83490 ) ) ;
#84768 = CARTESIAN_POINT ( 'NONE',  ( -12.89999999999999147, 12.50000000000000000, -5.022947341949751454 ) ) ;
#84769 = ORIENTED_EDGE ( 'NONE', *, *, #68252, .T. ) ;
#84770 = EDGE_LOOP ( 'NONE', ( #75215, #96954 ) ) ;
#84771 = ORIENTED_EDGE ( 'NONE', *, *, #97027, .F. ) ;
#84772 = CARTESIAN_POINT ( 'NONE',  ( -4.800000000000022915, 2.500000000000000000, 3.983716857408420076 ) ) ;
#84773 = CARTESIAN_POINT ( 'NONE',  ( 3.949999999999941558, 2.500000000000000000, -6.148780366869526226 ) ) ;
#84774 = CARTESIAN_POINT ( 'NONE',  ( 184.4010416670080872, -4.367472073101519747, 7.564683531249999149 ) ) ;
#84775 = AXIS2_PLACEMENT_3D ( 'NONE', #125106, #55078, #64880 ) ;
#84776 = CARTESIAN_POINT ( 'NONE',  ( 4.149999999999936406, 2.500000000000000000, 6.495190528383297135 ) ) ;
#84777 = DIRECTION ( 'NONE',  ( 0.000000000000000000, 1.000000000000000000, 0.000000000000000000 ) ) ;
#84778 = FACE_OUTER_BOUND ( 'NONE', #110208, .T. ) ;
#84779 = VECTOR ( 'NONE', #108844, 1000.000000000000000 ) ;
#84780 = VERTEX_POINT ( 'NONE', #45956 ) ;
#84781 = CIRCLE ( 'NONE', #38843, 0.06509327318403745899 ) ;
#84782 = CARTESIAN_POINT ( 'NONE',  ( -1.250000000000035749, 2.500000000000000000, -7.088010851410853519 ) ) ;
#84783 = ORIENTED_EDGE ( 'NONE', *, *, #97147, .T. ) ;
#84784 = CARTESIAN_POINT ( 'NONE',  ( 6.449999999999930012, 2.500000000000000000, 6.741600689897071952 ) ) ;
#84785 = CARTESIAN_POINT ( 'NONE',  ( 13.54999999999989946, 2.500000000000000000, 2.411473670974873862 ) ) ;
#84786 = PLANE ( 'NONE',  #110732 ) ;
#84787 = EDGE_LOOP ( 'NONE', ( #86146, #86501, #122878, #43196 ) ) ;
#84788 = CONICAL_SURFACE ( 'NONE', #82752, 0.1000000000000000472, 0.003490658503988666988 ) ;
#84789 = EDGE_CURVE ( 'NONE', #119412, #71724, #124516, .T. ) ;
#84790 = DIRECTION ( 'NONE',  ( 0.000000000000000000, -0.9999939076577903929, 0.003490651415223739937 ) ) ;
#84791 = DIRECTION ( 'NONE',  ( -0.000000000000000000, -1.000000000000000000, -0.000000000000000000 ) ) ;
#84792 = ORIENTED_EDGE ( 'NONE', *, *, #17607, .T. ) ;
#84793 = DIRECTION ( 'NONE',  ( 0.000000000000000000, 0.000000000000000000, 1.000000000000000000 ) ) ;
#84794 = ADVANCED_FACE ( 'NONE', ( #115969 ), #68547, .T. ) ;
#84795 = CIRCLE ( 'NONE', #122887, 0.1000000000000002554 ) ;
#84796 = EDGE_LOOP ( 'NONE', ( #10988, #42256, #114260, #14062 ) ) ;
#84797 = ORIENTED_EDGE ( 'NONE', *, *, #38679, .F. ) ;
#84798 = DIRECTION ( 'NONE',  ( 0.000000000000000000, 0.000000000000000000, 1.000000000000000000 ) ) ;
#84799 = ORIENTED_EDGE ( 'NONE', *, *, #97921, .F. ) ;
#84800 = CARTESIAN_POINT ( 'NONE',  ( -5.200000000000020606, 2.500000000000000000, -0.2464101615137782308 ) ) ;
#84801 = CARTESIAN_POINT ( 'NONE',  ( 10.19999999999991047, 2.500000000000000000, 4.676537180435972552 ) ) ;
#84802 = CARTESIAN_POINT ( 'NONE',  ( 7.699999999999923794, 12.50000000000000000, -4.048810130592463530 ) ) ;
#84803 = ORIENTED_EDGE ( 'NONE', *, *, #123477, .T. ) ;
#84804 = FACE_BOUND ( 'NONE', #29319, .T. ) ;
#84805 = DIRECTION ( 'NONE',  ( 0.000000000000000000, 1.000000000000000000, 0.000000000000000000 ) ) ;
#84807 = ORIENTED_EDGE ( 'NONE', *, *, #21504, .T. ) ;
#84806 = LINE ( 'NONE', #16050, #6069 ) ;
#84808 = DIRECTION ( 'NONE',  ( 0.000000000000000000, 0.000000000000000000, 1.000000000000000000 ) ) ;
#84809 = CARTESIAN_POINT ( 'NONE',  ( -12.94999999999999218, 12.50000000000000000, -2.230156782645137170 ) ) ;
#84810 = EDGE_LOOP ( 'NONE', ( #12554, #114307 ) ) ;
#84811 = VECTOR ( 'NONE', #101632, 1000.000000000000000 ) ;
#84812 = VERTEX_POINT ( 'NONE', #63662 ) ;
#84813 = AXIS2_PLACEMENT_3D ( 'NONE', #106200, #74806, #125192 ) ;
#84814 = ORIENTED_EDGE ( 'NONE', *, *, #93890, .F. ) ;
#84815 = CARTESIAN_POINT ( 'NONE',  ( 4.999999999999969802, 12.50000000000000000, 4.395220292106234439 ) ) ;
#84816 = CARTESIAN_POINT ( 'NONE',  ( -12.04999999999999716, 2.500000000000000000, -2.065063509461098068 ) ) ;
#84817 = CARTESIAN_POINT ( 'NONE',  ( -13.34999999999999076, 2.500000000000000000, -2.857883832488651521 ) ) ;
#84818 = APPLICATION_CONTEXT ( 'automotive_design' ) ;
#84819 = FACE_BOUND ( 'NONE', #2771, .T. ) ;
#84820 = EDGE_LOOP ( 'NONE', ( #31067, #95050 ) ) ;
#84821 = CARTESIAN_POINT ( 'NONE',  ( 185.3593750003413732, 0.000000000000000000, 7.564683531250000925 ) ) ;
#84822 = PLANE ( 'NONE',  #126308 ) ;
#84823 = CARTESIAN_POINT ( 'NONE',  ( 2.499999999999947153, 12.50000000000000000, 3.702399969078682407 ) ) ;
#84824 = ADVANCED_FACE ( 'NONE', ( #16461 ), #56395, .T. ) ;
#84825 = DIRECTION ( 'NONE',  ( 0.000000000000000000, 0.000000000000000000, 1.000000000000000000 ) ) ;
#84826 = B_SPLINE_CURVE_WITH_KNOTS ( 'NONE', 3,
 ( #71939, #123586, #61479, #101391, #1249, #11707 ),
 .UNSPECIFIED., .F., .F.,
 ( 4, 2, 4 ),
 ( 0.000000000000000000, 0.5000000000000000000, 1.000000000000000000 ),
 .UNSPECIFIED. ) ;
#84827 = DIRECTION ( 'NONE',  ( 0.000000000000000000, -0.9999939076577903929, 0.003490651415223739937 ) ) ;
#84828 = AXIS2_PLACEMENT_3D ( 'NONE', #80794, #29742, #10102 ) ;
#84829 = CARTESIAN_POINT ( 'NONE',  ( 194.5000000000000000, 0.000000000000000000, 0.000000000000000000 ) ) ;
#84830 = CARTESIAN_POINT ( 'NONE',  ( -14.14999999999998614, 2.500000000000000000, 1.472243186433549456 ) ) ;
#84831 = CONICAL_SURFACE ( 'NONE', #109893, 0.09999999999999982514, 0.003490658503988666988 ) ;
#84833 = EDGE_CURVE ( 'NONE', #52780, #56136, #47634, .T. ) ;
#84832 = AXIS2_PLACEMENT_3D ( 'NONE', #49153, #2586, #60880 ) ;
#84834 = DIRECTION ( 'NONE',  ( 0.000000000000000000, -0.000000000000000000, 1.000000000000000000 ) ) ;
#84835 = AXIS2_PLACEMENT_3D ( 'NONE', #7284, #37420, #77328 ) ;
#84836 = EDGE_LOOP ( 'NONE', ( #128151, #56921 ) ) ;
#84837 = VERTEX_POINT ( 'NONE', #113386 ) ;
#84838 = VERTEX_POINT ( 'NONE', #25013 ) ;
#84839 = ORIENTED_EDGE ( 'NONE', *, *, #99982, .T. ) ;
#84840 = CONICAL_SURFACE ( 'NONE', #99529, 0.1000000000000002554, 0.003490658503988666988 ) ;
#84841 = ORIENTED_EDGE ( 'NONE', *, *, #66063, .F. ) ;
#84842 = DIRECTION ( 'NONE',  ( 0.000000000000000000, 0.000000000000000000, 1.000000000000000000 ) ) ;
#84843 = EDGE_CURVE ( 'NONE', #116415, #101569, #14160, .T. ) ;
#84844 = CARTESIAN_POINT ( 'NONE',  ( -7.100000000000014744, 12.50000000000000000, 4.330127018922196314 ) ) ;
#84845 = ORIENTED_EDGE ( 'NONE', *, *, #83241, .F. ) ;
#84846 = FACE_BOUND ( 'NONE', #25904, .T. ) ;
#84847 = EDGE_CURVE ( 'NONE', #93338, #49329, #14529, .T. ) ;
#84848 = DIRECTION ( 'NONE',  ( 0.000000000000000000, 0.000000000000000000, 1.000000000000000000 ) ) ;
#84849 = ADVANCED_FACE ( 'NONE', ( #44659 ), #127092, .T. ) ;
#84850 = DIRECTION ( 'NONE',  ( 0.000000000000000000, -0.9999939076577903929, 0.003490651415223739937 ) ) ;
#84851 = EDGE_LOOP ( 'NONE', ( #69147, #125885, #98670, #30855 ) ) ;
#84852 = DIRECTION ( 'NONE',  ( 0.000000000000000000, 0.000000000000000000, -1.000000000000000000 ) ) ;
#84853 = DIRECTION ( 'NONE',  ( -0.000000000000000000, -1.000000000000000000, -0.000000000000000000 ) ) ;
#84854 = EDGE_CURVE ( 'NONE', #125708, #35689, #91546, .T. ) ;
#84855 = DIRECTION ( 'NONE',  ( 0.000000000000000000, 1.000000000000000000, 0.000000000000000000 ) ) ;
#84857 = ORIENTED_EDGE ( 'NONE', *, *, #54871, .T. ) ;
#84856 = CONICAL_SURFACE ( 'NONE', #59856, 0.09999999999999982514, 0.003490658503988666988 ) ;
#84858 = CARTESIAN_POINT ( 'NONE',  ( 6.649999999999930189, 12.50000000000000000, 7.253104124594885960 ) ) ;
#84859 = ORIENTED_EDGE ( 'NONE', *, *, #10262, .T. ) ;
#84860 = ORIENTED_EDGE ( 'NONE', *, *, #16992, .F. ) ;
#84861 = ORIENTED_EDGE ( 'NONE', *, *, #52775, .F. ) ;
#84862 = CARTESIAN_POINT ( 'NONE',  ( 9.999999999999948486, 2.500000000000000000, -4.430127018922202176 ) ) ;
#84863 = DIRECTION ( 'NONE',  ( -0.000000000000000000, -1.000000000000000000, -0.000000000000000000 ) ) ;
#84864 = CIRCLE ( 'NONE', #9568, 0.06509327318403741736 ) ;
#84865 = DIRECTION ( 'NONE',  ( 0.000000000000000000, 0.000000000000000000, 1.000000000000000000 ) ) ;
#84866 = EDGE_LOOP ( 'NONE', ( #32381, #67416, #104239, #21688 ) ) ;
#84867 = CARTESIAN_POINT ( 'NONE',  ( 10.28037028451818458, 2.500000000000381029, -9.136909653096239481 ) ) ;
#84868 = VECTOR ( 'NONE', #42030, 1000.000000000000000 ) ;
#84869 = AXIS2_PLACEMENT_3D ( 'NONE', #64395, #53939, #94488 ) ;
#84870 = DIRECTION ( 'NONE',  ( 0.000000000000000000, 1.000000000000000000, 0.000000000000000000 ) ) ;
#84871 = AXIS2_PLACEMENT_3D ( 'NONE', #20933, #40607, #30127 ) ;
#84872 = DIRECTION ( 'NONE',  ( -0.000000000000000000, 1.000000000000000000, -0.000000000000000000 ) ) ;
#84873 = CARTESIAN_POINT ( 'NONE',  ( 184.6145833340161175, 6.668395609140177704, -3.849999999999998312 ) ) ;
#84874 = CARTESIAN_POINT ( 'NONE',  ( 127.5000000000000000, -2.000000000000000000, 2.000000000000001776 ) ) ;
#84875 = CARTESIAN_POINT ( 'NONE',  ( 8.349999999999919709, 12.50000000000000000, -1.472243186433550122 ) ) ;
#84876 = VERTEX_POINT ( 'NONE', #59665 ) ;
#84877 = DIRECTION ( 'NONE',  ( 0.000000000000000000, 0.000000000000000000, 1.000000000000000000 ) ) ;
#84878 = CIRCLE ( 'NONE', #120484, 0.06509327318403745899 ) ;
#84879 = ORIENTED_EDGE ( 'NONE', *, *, #111624, .F. ) ;
#84881 = VECTOR ( 'NONE', #22429, 1000.000000000000000 ) ;
#84880 = AXIS2_PLACEMENT_3D ( 'NONE', #56852, #5183, #106613 ) ;
#84882 = ORIENTED_EDGE ( 'NONE', *, *, #96371, .F. ) ;
#84883 = LINE ( 'NONE', #82320, #78488 ) ;
#84884 = CARTESIAN_POINT ( 'NONE',  ( 187.3906250003414016, 0.000000000000000000, 7.564683531250000925 ) ) ;
#84885 = CARTESIAN_POINT ( 'NONE',  ( 3.299999999999944755, 2.500000000000000000, -4.330127018922201643 ) ) ;
#84886 = DIRECTION ( 'NONE',  ( 0.000000000000000000, 0.000000000000000000, -1.000000000000000000 ) ) ;
#84887 = CARTESIAN_POINT ( 'NONE',  ( -10.40000000000000213, 2.500000000000000000, 5.022947341949748790 ) ) ;
#84888 = ORIENTED_EDGE ( 'NONE', *, *, #45404, .F. ) ;
#84890 = ADVANCED_FACE ( 'NONE', ( #128394 ), #106216, .T. ) ;
#84889 = ORIENTED_EDGE ( 'NONE', *, *, #106328, .T. ) ;
#84891 = PLANE ( 'NONE',  #83203 ) ;
#84892 = DIRECTION ( 'NONE',  ( -0.000000000000000000, 1.000000000000000000, -0.000000000000000000 ) ) ;
#84894 = EDGE_CURVE ( 'NONE', #107837, #49056, #35131, .T. ) ;
#84893 = CARTESIAN_POINT ( 'NONE',  ( -3.750000000000025757, 2.500000000000000000, 1.472243186433545459 ) ) ;
#84895 = ORIENTED_EDGE ( 'NONE', *, *, #74897, .T. ) ;
#84896 = ORIENTED_EDGE ( 'NONE', *, *, #37309, .T. ) ;
#84897 = EDGE_CURVE ( 'NONE', #78919, #35564, #102011, .T. ) ;
#84898 = CARTESIAN_POINT ( 'NONE',  ( -9.350000000000008527, 2.500000000000000000, -6.248780366869521430 ) ) ;
#84899 = ADVANCED_FACE ( 'NONE', ( #58993 ), #37362, .T. ) ;
#84900 = EDGE_CURVE ( 'NONE', #101832, #9579, #118538, .T. ) ;
#84901 = EDGE_LOOP ( 'NONE', ( #40042, #46209, #86502, #5249 ) ) ;
#84902 = CARTESIAN_POINT ( 'NONE',  ( -4.150000000000024336, 12.50000000000000000, 1.472243186433545459 ) ) ;
#84903 = FACE_OUTER_BOUND ( 'NONE', #102206, .T. ) ;
#84904 = VERTEX_POINT ( 'NONE', #8571 ) ;
#84905 = DIRECTION ( 'NONE',  ( -0.000000000000000000, -1.000000000000000000, -0.000000000000000000 ) ) ;
#84906 = EDGE_CURVE ( 'NONE', #45052, #9793, #49889, .T. ) ;
#84907 = LINE ( 'NONE', #113738, #29525 ) ;
#84908 = DIRECTION ( 'NONE',  ( 0.000000000000000000, 0.000000000000000000, -1.000000000000000000 ) ) ;
#84909 = DIRECTION ( 'NONE',  ( 0.000000000000000000, 0.000000000000000000, 1.000000000000000000 ) ) ;
#84910 = ORIENTED_EDGE ( 'NONE', *, *, #33975, .T. ) ;
#84911 = ADVANCED_FACE ( 'NONE', ( #106780 ), #64439, .T. ) ;
#84912 = DIRECTION ( 'NONE',  ( 0.000000000000000000, -0.000000000000000000, 1.000000000000000000 ) ) ;
#84913 = ADVANCED_FACE ( 'NONE', ( #68148 ), #14259, .T. ) ;
#84914 = CIRCLE ( 'NONE', #86965, 0.06509327318403745899 ) ;
#84915 = AXIS2_PLACEMENT_3D ( 'NONE', #41338, #31499, #42629 ) ;
#84916 = CARTESIAN_POINT ( 'NONE',  ( 14.54999999999989591, 2.500000000000000000, 2.165063509461097713 ) ) ;
#84917 = EDGE_LOOP ( 'NONE', ( #19809, #44680, #98007, #107709 ) ) ;
#84918 = EDGE_LOOP ( 'NONE', ( #46865, #83954 ) ) ;
#84919 = CARTESIAN_POINT ( 'NONE',  ( 184.0052083336747160, -6.551208109652278289, 3.782341765624995134 ) ) ;
#84920 = DIRECTION ( 'NONE',  ( 0.000000000000000000, -0.9999939076577903929, 0.003490651415223739937 ) ) ;
#84921 = DIRECTION ( 'NONE',  ( 0.000000000000000000, 0.000000000000000000, 1.000000000000000000 ) ) ;
#84922 = DIRECTION ( 'NONE',  ( 0.000000000000000000, -0.9999939076577903929, 0.003490651415223739937 ) ) ;
#84925 = CIRCLE ( 'NONE', #74467, 0.09999999999999999167 ) ;
#84924 = CARTESIAN_POINT ( 'NONE',  ( -0.2000000000000347888, 2.500000000000000000, 0.3464101615137758494 ) ) ;
#84923 = AXIS2_PLACEMENT_3D ( 'NONE', #102350, #79490, #51965 ) ;
#84926 = LINE ( 'NONE', #113757, #126138 ) ;
#84927 = DIRECTION ( 'NONE',  ( -0.000000000000000000, -1.000000000000000000, -0.000000000000000000 ) ) ;
#84928 = DIRECTION ( 'NONE',  ( -0.000000000000000000, 1.000000000000000000, -0.000000000000000000 ) ) ;
#84929 = DIRECTION ( 'NONE',  ( 0.000000000000000000, -0.9999939076577903929, 0.003490651415223739937 ) ) ;
#84930 = DIRECTION ( 'NONE',  ( 0.000000000000000000, 0.000000000000000000, 1.000000000000000000 ) ) ;
#84932 = CONICAL_SURFACE ( 'NONE', #47384, 0.1000000000000002554, 0.003490658503988666988 ) ;
#84931 = AXIS2_PLACEMENT_3D ( 'NONE', #114712, #53872, #74804 ) ;
#84933 = VERTEX_POINT ( 'NONE', #87142 ) ;
#84934 = VERTEX_POINT ( 'NONE', #7938 ) ;
#84935 = ORIENTED_EDGE ( 'NONE', *, *, #56283, .T. ) ;
#84936 = ORIENTED_EDGE ( 'NONE', *, *, #91953, .F. ) ;
#84937 = FACE_OUTER_BOUND ( 'NONE', #82027, .T. ) ;
#84938 = CARTESIAN_POINT ( 'NONE',  ( 9.199999999999915801, 2.500000000000000000, 4.330127018922196314 ) ) ;
#84939 = FACE_OUTER_BOUND ( 'NONE', #78154, .T. ) ;
#84940 = ORIENTED_EDGE ( 'NONE', *, *, #63545, .T. ) ;
#84941 = LINE ( 'NONE', #125507, #107273 ) ;
#84942 = DIRECTION ( 'NONE',  ( 0.000000000000000000, 0.000000000000000000, -1.000000000000000000 ) ) ;
#84944 = ORIENTED_EDGE ( 'NONE', *, *, #116754, .T. ) ;
#84943 = DIRECTION ( 'NONE',  ( 0.000000000000000000, 1.000000000000000000, 0.000000000000000000 ) ) ;
#84945 = CARTESIAN_POINT ( 'NONE',  ( 7.099999999999928590, 12.50000000000000000, -5.022947341949754119 ) ) ;
#84946 = ORIENTED_EDGE ( 'NONE', *, *, #2702, .T. ) ;
#84947 = ADVANCED_FACE ( 'NONE', ( #67487 ), #47890, .T. ) ;
#84948 = VECTOR ( 'NONE', #69684, 1000.000000000000000 ) ;
#84949 = AXIS2_PLACEMENT_3D ( 'NONE', #106956, #115479, #65749 ) ;
#84950 = ORIENTED_EDGE ( 'NONE', *, *, #15380, .T. ) ;
#84951 = VERTEX_POINT ( 'NONE', #18413 ) ;
#84952 = VERTEX_POINT ( 'NONE', #78645 ) ;
#84953 = CARTESIAN_POINT ( 'NONE',  ( 1.249999999999952038, 2.500000000000000000, 5.902370205355745192 ) ) ;
#84954 = AXIS2_PLACEMENT_3D ( 'NONE', #16264, #98698, #7749 ) ;
#84955 = AXIS2_PLACEMENT_3D ( 'NONE', #63605, #93702, #83870 ) ;
#84956 = DIRECTION ( 'NONE',  ( 0.000000000000000000, 0.000000000000000000, 1.000000000000000000 ) ) ;
#84957 = FACE_OUTER_BOUND ( 'NONE', #84820, .T. ) ;
#84958 = CIRCLE ( 'NONE', #28537, 0.06509327318403745899 ) ;
#84959 = CARTESIAN_POINT ( 'NONE',  ( -5.650000000000023448, 2.500000000000000000, -1.818653347947326138 ) ) ;
#84960 = ORIENTED_EDGE ( 'NONE', *, *, #73839, .F. ) ;
#84961 = VECTOR ( 'NONE', #34641, 1000.000000000000000 ) ;
#84962 = DIRECTION ( 'NONE',  ( -0.000000000000000000, -1.000000000000000000, -0.000000000000000000 ) ) ;
#84963 = EDGE_LOOP ( 'NONE', ( #13794, #9381 ) ) ;
#84964 = CARTESIAN_POINT ( 'NONE',  ( 26.61818291011036308, -2.722754637270933475, -4.358315985290887262 ) ) ;
#84965 = CARTESIAN_POINT ( 'NONE',  ( 3.710216157338390275, -1.500000000001404432, -9.999999999999998224 ) ) ;
#84966 = PLANE ( 'NONE',  #8781 ) ;
#84967 = CARTESIAN_POINT ( 'NONE',  ( -3.150000000000030553, 2.500000000000000000, 6.148780366869520009 ) ) ;
#84968 = CIRCLE ( 'NONE', #45274, 0.1000000000000002554 ) ;
#84969 = EDGE_LOOP ( 'NONE', ( #121387, #72197, #1506, #29689 ) ) ;
#84970 = CIRCLE ( 'NONE', #80793, 0.1000000000000002554 ) ;
#84971 = ORIENTED_EDGE ( 'NONE', *, *, #8066, .F. ) ;
#84972 = ORIENTED_EDGE ( 'NONE', *, *, #118086, .T. ) ;
#84973 = DIRECTION ( 'NONE',  ( -0.000000000000000000, -1.000000000000000000, -0.000000000000000000 ) ) ;
#84974 = CARTESIAN_POINT ( 'NONE',  ( -9.600000000000006750, 2.500000000000000000, 0.7928203230275495672 ) ) ;
#84975 = DIRECTION ( 'NONE',  ( 0.000000000000000000, 0.000000000000000000, -1.000000000000000000 ) ) ;
#84976 = FACE_BOUND ( 'NONE', #82472, .T. ) ;
#84977 = LINE ( 'NONE', #16850, #76572 ) ;
#84978 = DIRECTION ( 'NONE',  ( 0.000000000000000000, 0.000000000000000000, -1.000000000000000000 ) ) ;
#84979 = DIRECTION ( 'NONE',  ( 1.000000000000000000, 0.000000000000000000, 0.000000000000000000 ) ) ;
#84980 = CARTESIAN_POINT ( 'NONE',  ( -1.050000000000038680, 12.50000000000000000, 2.576566944158910744 ) ) ;
#84981 = CARTESIAN_POINT ( 'NONE',  ( -6.050000000000017586, 2.500000000000000000, 1.818653347947321475 ) ) ;
#84982 = FACE_OUTER_BOUND ( 'NONE', #2819, .T. ) ;
#84983 = EDGE_LOOP ( 'NONE', ( #59103, #22017 ) ) ;
#84984 = EDGE_CURVE ( 'NONE', #94668, #23121, #48523, .T. ) ;
#84985 = FACE_OUTER_BOUND ( 'NONE', #74589, .T. ) ;
#84986 = ORIENTED_EDGE ( 'NONE', *, *, #19223, .F. ) ;
#84987 = ORIENTED_EDGE ( 'NONE', *, *, #103963, .F. ) ;
#84988 = EDGE_LOOP ( 'NONE', ( #34473, #38393, #65481, #106456 ) ) ;
#84989 = ORIENTED_EDGE ( 'NONE', *, *, #42682, .F. ) ;
#84990 = EDGE_CURVE ( 'NONE', #6208, #24462, #16386, .T. ) ;
#84991 = CARTESIAN_POINT ( 'NONE',  ( -11.24999999999999822, 2.500000000000000000, 5.802370205355744659 ) ) ;
#84992 = FACE_BOUND ( 'NONE', #63641, .T. ) ;
#84993 = ADVANCED_FACE ( 'NONE', ( #19709 ), #53985, .T. ) ;
#84994 = DIRECTION ( 'NONE',  ( 0.000000000000000000, 0.000000000000000000, -1.000000000000000000 ) ) ;
#84995 = CIRCLE ( 'NONE', #80810, 0.06509327318403741736 ) ;
#84996 = CIRCLE ( 'NONE', #59899, 5.000000000000000000 ) ;
#84997 = EDGE_CURVE ( 'NONE', #61622, #23744, #43626, .T. ) ;
#84998 = ADVANCED_FACE ( 'NONE', ( #116605 ), #26950, .T. ) ;
#84999 = EDGE_LOOP ( 'NONE', ( #100111, #86647 ) ) ;
#85000 = FACE_OUTER_BOUND ( 'NONE', #106156, .T. ) ;
#85001 = EDGE_CURVE ( 'NONE', #115300, #91287, #97888, .T. ) ;
#85002 = LINE ( 'NONE', #44442, #41660 ) ;
#85003 = ADVANCED_FACE ( 'NONE', ( #111964 ), #110028, .T. ) ;
#85004 = VERTEX_POINT ( 'NONE', #32774 ) ;
#85005 = CARTESIAN_POINT ( 'NONE',  ( -8.100000000000013856, 12.50000000000000000, -3.983716857408426293 ) ) ;
#85006 = CARTESIAN_POINT ( 'NONE',  ( -4.350000000000027178, 12.50000000000000000, -6.906693963081115051 ) ) ;
#85007 = VECTOR ( 'NONE', #102195, 1000.000000000000000 ) ;
#85008 = ORIENTED_EDGE ( 'NONE', *, *, #95210, .T. ) ;
#85009 = CARTESIAN_POINT ( 'NONE',  ( 3.549999999999944755, 2.500000000000000000, -6.841600689897077814 ) ) ;
#85012 = EDGE_CURVE ( 'NONE', #36022, #49975, #40661, .T. ) ;
#85011 = AXIS2_PLACEMENT_3D ( 'NONE', #54438, #66192, #75363 ) ;
#85010 = DIRECTION ( 'NONE',  ( -0.000000000000000000, -1.000000000000000000, -0.000000000000000000 ) ) ;
#85014 = AXIS2_PLACEMENT_3D ( 'NONE', #75323, #83227, #103508 ) ;
#85013 = CIRCLE ( 'NONE', #116309, 0.06509327318403745899 ) ;
#85015 = ORIENTED_EDGE ( 'NONE', *, *, #99401, .T. ) ;
#85016 = AXIS2_PLACEMENT_3D ( 'NONE', #25121, #26425, #66963 ) ;
#85017 = CARTESIAN_POINT ( 'NONE',  ( -13.14999999999999147, 2.500000000000000000, -2.411473670974875638 ) ) ;
#85018 = DIRECTION ( 'NONE',  ( -0.000000000000000000, 1.000000000000000000, -0.000000000000000000 ) ) ;
#85019 = DIRECTION ( 'NONE',  ( 0.000000000000000000, 0.000000000000000000, 1.000000000000000000 ) ) ;
#85020 = ORIENTED_EDGE ( 'NONE', *, *, #61233, .T. ) ;
#85021 = VERTEX_POINT ( 'NONE', #101495 ) ;
#85022 = DIRECTION ( 'NONE',  ( 0.000000000000000000, 0.000000000000000000, 1.000000000000000000 ) ) ;
#85023 = VERTEX_POINT ( 'NONE', #62851 ) ;
#85024 = DIRECTION ( 'NONE',  ( 0.000000000000000000, 0.000000000000000000, 1.000000000000000000 ) ) ;
#85025 = DIRECTION ( 'NONE',  ( 0.000000000000000000, 0.000000000000000000, 1.000000000000000000 ) ) ;
#85026 = VERTEX_POINT ( 'NONE', #102761 ) ;
#85027 = FACE_OUTER_BOUND ( 'NONE', #34096, .T. ) ;
#85028 = DIRECTION ( 'NONE',  ( 0.000000000000000000, 0.000000000000000000, 1.000000000000000000 ) ) ;
#85029 = DIRECTION ( 'NONE',  ( -0.000000000000000000, 1.000000000000000000, -0.000000000000000000 ) ) ;
#85030 = DIRECTION ( 'NONE',  ( 0.000000000000000000, 1.000000000000000000, 0.000000000000000000 ) ) ;
#85031 = EDGE_CURVE ( 'NONE', #107528, #34472, #72861, .T. ) ;
#85032 = CIRCLE ( 'NONE', #83007, 0.06509327318403745899 ) ;
#85034 = VECTOR ( 'NONE', #67458, 1000.000000000000000 ) ;
#85033 = DIRECTION ( 'NONE',  ( 0.000000000000000000, 0.000000000000000000, 1.000000000000000000 ) ) ;
#85035 = CONICAL_SURFACE ( 'NONE', #20212, 0.1000000000000002554, 0.003490658503988666988 ) ;
#85036 = ORIENTED_EDGE ( 'NONE', *, *, #86293, .T. ) ;
#85037 = VERTEX_POINT ( 'NONE', #2622 ) ;
#85038 = DIRECTION ( 'NONE',  ( -0.000000000000000000, 1.000000000000000000, -0.000000000000000000 ) ) ;
#85039 = AXIS2_PLACEMENT_3D ( 'NONE', #78728, #108794, #38140 ) ;
#85040 = CARTESIAN_POINT ( 'NONE',  ( 17.19804440726969474, -0.4677972980984264617, 5.492654682185391657 ) ) ;
#85041 = CARTESIAN_POINT ( 'NONE',  ( -7.300000000000018474, 12.50000000000000000, -3.983716857408426293 ) ) ;
#85043 = ORIENTED_EDGE ( 'NONE', *, *, #113728, .F. ) ;
#85042 = ORIENTED_EDGE ( 'NONE', *, *, #2682, .F. ) ;
#85044 = EDGE_LOOP ( 'NONE', ( #7726, #6377 ) ) ;
#85045 = ADVANCED_FACE ( 'NONE', ( #11809 ), #5927, .T. ) ;
#85046 = CARTESIAN_POINT ( 'NONE',  ( 1.899999999999949507, 12.50000000000000000, 3.983716857408420964 ) ) ;
#85047 = AXIS2_PLACEMENT_3D ( 'NONE', #14790, #63282, #94669 ) ;
#85048 = ADVANCED_FACE ( 'NONE', ( #54 ), #89583, .T. ) ;
#85049 = CONICAL_SURFACE ( 'NONE', #18146, 0.09999999999999999167, 0.003490658503988666988 ) ;
#85050 = DIRECTION ( 'NONE',  ( -0.6795087154616696878, -6.363550617825450602E-16, 0.7336674352945151689 ) ) ;
#85051 = DIRECTION ( 'NONE',  ( -0.000000000000000000, 1.000000000000000000, -0.000000000000000000 ) ) ;
#85052 = VECTOR ( 'NONE', #122481, 1000.000000000000000 ) ;
#85053 = EDGE_CURVE ( 'NONE', #122997, #51911, #70100, .T. ) ;
#85054 = CARTESIAN_POINT ( 'NONE',  ( 0.000000000000000000, 0.000000000000000000, 0.000000000000000000 ) ) ;
#85055 = DIRECTION ( 'NONE',  ( 0.000000000000000000, 0.000000000000000000, -1.000000000000000000 ) ) ;
#85056 = CARTESIAN_POINT ( 'NONE',  ( -4.800000000000022915, 12.50000000000000000, -0.4115034346978157509 ) ) ;
#85057 = CARTESIAN_POINT ( 'NONE',  ( -3.350000000000028511, 2.500000000000000000, -1.572243186433550211 ) ) ;
#85058 = DIRECTION ( 'NONE',  ( 0.000000000000000000, 0.000000000000000000, -1.000000000000000000 ) ) ;
#85059 = DIRECTION ( 'NONE',  ( 0.000000000000000000, 0.000000000000000000, 1.000000000000000000 ) ) ;
#85060 = AXIS2_PLACEMENT_3D ( 'NONE', #63480, #92948, #103406 ) ;
#85061 = EDGE_CURVE ( 'NONE', #16079, #48393, #112605, .T. ) ;
#85062 = DIRECTION ( 'NONE',  ( 0.000000000000000000, 1.000000000000000000, 0.000000000000000000 ) ) ;
#85063 = AXIS2_PLACEMENT_3D ( 'NONE', #13171, #62936, #3372 ) ;
#85064 = EDGE_CURVE ( 'NONE', #108831, #8397, #22937, .T. ) ;
#85066 = ORIENTED_EDGE ( 'NONE', *, *, #41477, .T. ) ;
#85065 = EDGE_CURVE ( 'NONE', #92765, #90185, #62222, .T. ) ;
#85069 = ADVANCED_FACE ( 'NONE', ( #121125 ), #41494, .T. ) ;
#85068 = CIRCLE ( 'NONE', #26499, 0.06509327318403745899 ) ;
#85067 = AXIS2_PLACEMENT_3D ( 'NONE', #22624, #63164, #112283 ) ;
#85070 = CARTESIAN_POINT ( 'NONE',  ( 12.69999999999989804, 2.500000000000000000, 0.4464101615137735513 ) ) ;
#85071 = ORIENTED_EDGE ( 'NONE', *, *, #30060, .F. ) ;
#85072 = ORIENTED_EDGE ( 'NONE', *, *, #98026, .T. ) ;
#85073 = DIRECTION ( 'NONE',  ( -0.000000000000000000, 1.000000000000000000, -0.000000000000000000 ) ) ;
#85074 = DIRECTION ( 'NONE',  ( 0.000000000000000000, 0.000000000000000000, 1.000000000000000000 ) ) ;
#85075 = DIRECTION ( 'NONE',  ( 0.000000000000000000, 0.000000000000000000, -1.000000000000000000 ) ) ;
#85076 = ADVANCED_FACE ( 'NONE', ( #72038 ), #102137, .T. ) ;
#85077 = CARTESIAN_POINT ( 'NONE',  ( -0.2000000000000412836, 2.500000000000000000, 4.776537180435972196 ) ) ;
#85078 = CARTESIAN_POINT ( 'NONE',  ( -1.850000000000033840, 2.500000000000000000, 6.841600689897072485 ) ) ;
#85079 = CARTESIAN_POINT ( 'NONE',  ( 2.049999999999948308, 12.50000000000000000, 6.495190528383297135 ) ) ;
#85080 = DIRECTION ( 'NONE',  ( -0.000000000000000000, -1.000000000000000000, -0.000000000000000000 ) ) ;
#85081 = ORIENTED_EDGE ( 'NONE', *, *, #38638, .F. ) ;
#85082 = DIRECTION ( 'NONE',  ( 0.000000000000000000, 0.000000000000000000, -1.000000000000000000 ) ) ;
#85083 = AXIS2_PLACEMENT_3D ( 'NONE', #78302, #28545, #36448 ) ;
#85084 = CARTESIAN_POINT ( 'NONE',  ( 1.849999999999949019, 2.500000000000000000, 6.741600689897071952 ) ) ;
#85085 = ORIENTED_EDGE ( 'NONE', *, *, #93874, .F. ) ;
#85086 = ORIENTED_EDGE ( 'NONE', *, *, #64650, .T. ) ;
#85087 = ORIENTED_EDGE ( 'NONE', *, *, #54244, .T. ) ;
#85088 = ORIENTED_EDGE ( 'NONE', *, *, #23768, .T. ) ;
#85089 = DIRECTION ( 'NONE',  ( 0.000000000000000000, -0.000000000000000000, 1.000000000000000000 ) ) ;
#85090 = DIRECTION ( 'NONE',  ( -0.000000000000000000, 1.000000000000000000, -0.000000000000000000 ) ) ;
#85091 = CONICAL_SURFACE ( 'NONE', #116478, 0.1000000000000002554, 0.003490658503988666988 ) ;
#85092 = DIRECTION ( 'NONE',  ( -0.000000000000000000, 1.000000000000000000, -0.000000000000000000 ) ) ;
#85094 = CARTESIAN_POINT ( 'NONE',  ( -5.850000000000018296, 2.500000000000000000, 2.957883832488649389 ) ) ;
#85093 = CONICAL_SURFACE ( 'NONE', #87149, 0.09999999999999982514, 0.003490658503988666988 ) ;
#85095 = LINE ( 'NONE', #15037, #11593 ) ;
#85096 = EDGE_LOOP ( 'NONE', ( #115202, #63136 ) ) ;
#85097 = CARTESIAN_POINT ( 'NONE',  ( -12.04999999999999538, 2.500000000000000000, 6.495190528383297135 ) ) ;
#85098 = CARTESIAN_POINT ( 'NONE',  ( 6.649999999999927525, 2.500000000000000000, 2.165063509461097713 ) ) ;
#85100 = CIRCLE ( 'NONE', #1475, 0.06509327318403745899 ) ;
#85099 = CIRCLE ( 'NONE', #9801, 0.06509327318403745899 ) ;
#85101 = DIRECTION ( 'NONE',  ( 0.000000000000000000, 0.000000000000000000, 1.000000000000000000 ) ) ;
#85102 = EDGE_LOOP ( 'NONE', ( #100052, #103301, #2705, #105003 ) ) ;
#85103 = ADVANCED_FACE ( 'NONE', ( #20989 ), #700, .T. ) ;
#85104 = EDGE_LOOP ( 'NONE', ( #31707, #63367 ) ) ;
#85105 = ORIENTED_EDGE ( 'NONE', *, *, #9898, .T. ) ;
#85106 = DIRECTION ( 'NONE',  ( 0.000000000000000000, 0.000000000000000000, 1.000000000000000000 ) ) ;
#85107 = CONICAL_SURFACE ( 'NONE', #45417, 0.1000000000000000056, 0.003490658503988666988 ) ;
#85108 = DIRECTION ( 'NONE',  ( 0.000000000000000000, 1.000000000000000000, 0.000000000000000000 ) ) ;
#85109 = DIRECTION ( 'NONE',  ( -0.000000000000000000, -1.000000000000000000, -0.000000000000000000 ) ) ;
#85110 = CONICAL_SURFACE ( 'NONE', #68481, 0.1000000000000002554, 0.003490658503988666988 ) ;
#85111 = ORIENTED_EDGE ( 'NONE', *, *, #79504, .T. ) ;
#85112 = FACE_OUTER_BOUND ( 'NONE', #78044, .T. ) ;
#85113 = DIRECTION ( 'NONE',  ( -4.274815082592931898E-19, -0.9999939076577903929, -0.003490651415223739937 ) ) ;
#85114 = ADVANCED_FACE ( 'NONE', ( #50448 ), #120483, .T. ) ;
#85115 = DIRECTION ( 'NONE',  ( -0.000000000000000000, -1.000000000000000000, -0.000000000000000000 ) ) ;
#85116 = CARTESIAN_POINT ( 'NONE',  ( -6.249999999999984901, 12.50000000000000000, -6.495190528383302464 ) ) ;
#85117 = DIRECTION ( 'NONE',  ( 0.000000000000000000, 0.000000000000000000, -1.000000000000000000 ) ) ;
#85118 = ORIENTED_EDGE ( 'NONE', *, *, #19014, .F. ) ;
#85119 = CARTESIAN_POINT ( 'NONE',  ( 175.5000000000000000, 0.000000000000000000, -5.000000000000000000 ) ) ;
#85120 = ORIENTED_EDGE ( 'NONE', *, *, #71655, .F. ) ;
#85121 = ORIENTED_EDGE ( 'NONE', *, *, #73497, .F. ) ;
#85122 = VERTEX_POINT ( 'NONE', #60914 ) ;
#85123 = CARTESIAN_POINT ( 'NONE',  ( 8.749999999999921840, 2.500000000000000000, 2.857883832488649301 ) ) ;
#85124 = FACE_BOUND ( 'NONE', #41914, .T. ) ;
#85125 = AXIS2_PLACEMENT_3D ( 'NONE', #30806, #38703, #109341 ) ;
#85126 = CARTESIAN_POINT ( 'NONE',  ( 10.64999999999991331, 12.50000000000000000, -1.753560074763288457 ) ) ;
#85127 = CARTESIAN_POINT ( 'NONE',  ( 11.24999999999990763, 12.50000000000000000, 1.537336459617582918 ) ) ;
#85128 = CONICAL_SURFACE ( 'NONE', #37028, 0.09999999999999982514, 0.003490658503988666988 ) ;
#85129 = DIRECTION ( 'NONE',  ( 0.000000000000000000, 0.000000000000000000, -1.000000000000000000 ) ) ;
#85130 = VECTOR ( 'NONE', #112176, 1000.000000000000000 ) ;
#85131 = VERTEX_POINT ( 'NONE', #11161 ) ;
#85132 = CARTESIAN_POINT ( 'NONE',  ( 6.899999999999926636, 12.50000000000000000, -0.3464101615137782364 ) ) ;
#85133 = DIRECTION ( 'NONE',  ( -0.000000000000000000, 1.000000000000000000, -0.000000000000000000 ) ) ;
#85135 = FACE_OUTER_BOUND ( 'NONE', #5869, .T. ) ;
#85134 = CIRCLE ( 'NONE', #114382, 0.06509327318403745899 ) ;
#85137 = DIRECTION ( 'NONE',  ( -4.274815082592931898E-19, -0.9999939076577903929, -0.003490651415223739937 ) ) ;
#85136 = VECTOR ( 'NONE', #107060, 1000.000000000000000 ) ;
#85138 = EDGE_LOOP ( 'NONE', ( #121054, #90168 ) ) ;
#85139 = LINE ( 'NONE', #14453, #19691 ) ;
#85140 = CONICAL_SURFACE ( 'NONE', #62180, 0.1000000000000002554, 0.003490658503988666988 ) ;
#85141 = AXIS2_PLACEMENT_3D ( 'NONE', #67372, #75936, #5891 ) ;
#85142 = EDGE_CURVE ( 'NONE', #104830, #31947, #91632, .T. ) ;
#85143 = FACE_OUTER_BOUND ( 'NONE', #60633, .T. ) ;
#85144 = ORIENTED_EDGE ( 'NONE', *, *, #47825, .F. ) ;
#85145 = CARTESIAN_POINT ( 'NONE',  ( 3.299999999999944755, 2.500000000000000000, -4.430127018922202176 ) ) ;
#85146 = AXIS2_PLACEMENT_3D ( 'NONE', #33241, #102591, #50938 ) ;
#85147 = VERTEX_POINT ( 'NONE', #41936 ) ;
#85148 = FACE_BOUND ( 'NONE', #22183, .T. ) ;
#85149 = ADVANCED_FACE ( 'NONE', ( #95540 ), #85703, .T. ) ;
#85150 = FACE_OUTER_BOUND ( 'NONE', #125112, .T. ) ;
#85152 = CONICAL_SURFACE ( 'NONE', #89374, 0.09999999999999982514, 0.003490658503988666988 ) ;
#85151 = CONICAL_SURFACE ( 'NONE', #87204, 0.1000000000000000472, 0.003490658503988666988 ) ;
#85153 = ORIENTED_EDGE ( 'NONE', *, *, #49751, .T. ) ;
#85154 = DIRECTION ( 'NONE',  ( -4.274815082592931898E-19, -0.9999939076577903929, -0.003490651415223739937 ) ) ;
#85155 = DIRECTION ( 'NONE',  ( 0.000000000000000000, 1.000000000000000000, 0.000000000000000000 ) ) ;
#85156 = ADVANCED_FACE ( 'NONE', ( #73961 ), #1734, .T. ) ;
#85157 = VERTEX_POINT ( 'NONE', #93598 ) ;
#85158 = ADVANCED_FACE ( 'NONE', ( #105999 ), #33411, .T. ) ;
#85159 = EDGE_LOOP ( 'NONE', ( #57117, #16910 ) ) ;
#85160 = EDGE_CURVE ( 'NONE', #33313, #112742, #54321, .T. ) ;
#85161 = ADVANCED_FACE ( 'NONE', ( #66064 ), #53039, .T. ) ;
#85162 = CARTESIAN_POINT ( 'NONE',  ( 185.3802083336747160, 4.367472073101515306, 7.564683531250000925 ) ) ;
#85163 = ORIENTED_EDGE ( 'NONE', *, *, #19555, .F. ) ;
#85164 = CARTESIAN_POINT ( 'NONE',  ( 185.1718750003414016, 9.264065473108010111E-16, -7.564683531250000925 ) ) ;
#85165 = DIRECTION ( 'NONE',  ( -0.000000000000000000, -1.000000000000000000, -0.000000000000000000 ) ) ;
#85166 = CARTESIAN_POINT ( 'NONE',  ( -0.8500000000000386136, 2.500000000000000000, 2.857883832488649301 ) ) ;
#85167 = CARTESIAN_POINT ( 'NONE',  ( 1.899999999999949507, 2.500000000000000000, 3.983716857408420964 ) ) ;
#85168 = FACE_OUTER_BOUND ( 'NONE', #12183, .T. ) ;
#85169 = CARTESIAN_POINT ( 'NONE',  ( 11.24999999999990763, 2.500000000000000000, 1.572243186433545548 ) ) ;
#85171 = EDGE_CURVE ( 'NONE', #74962, #85395, #83336, .T. ) ;
#85170 = CIRCLE ( 'NONE', #122832, 0.1000000000000000472 ) ;
#85172 = EDGE_CURVE ( 'NONE', #110704, #46732, #85372, .T. ) ;
#85173 = ADVANCED_FACE ( 'NONE', ( #105355 ), #125082, .T. ) ;
#85174 = ORIENTED_EDGE ( 'NONE', *, *, #102084, .F. ) ;
#85175 = ORIENTED_EDGE ( 'NONE', *, *, #84847, .T. ) ;
#85176 = CARTESIAN_POINT ( 'NONE',  ( 9.149999999999920419, 2.500000000000000000, -5.802370205355749988 ) ) ;
#85177 = DIRECTION ( 'NONE',  ( -4.274815082592931898E-19, -0.9999939076577903929, -0.003490651415223739937 ) ) ;
#85178 = DIRECTION ( 'NONE',  ( 0.000000000000000000, 1.000000000000000000, 0.000000000000000000 ) ) ;
#85179 = CARTESIAN_POINT ( 'NONE',  ( -2.300000000000033129, 12.50000000000000000, 3.983716857408420076 ) ) ;
#85181 = EDGE_LOOP ( 'NONE', ( #87088, #9532 ) ) ;
#85180 = ORIENTED_EDGE ( 'NONE', *, *, #79725, .F. ) ;
#85182 = FACE_BOUND ( 'NONE', #80004, .T. ) ;
#85183 = EDGE_LOOP ( 'NONE', ( #48306, #61862, #124225, #111979 ) ) ;
#85184 = DIRECTION ( 'NONE',  ( -0.000000000000000000, -1.000000000000000000, -0.000000000000000000 ) ) ;
#85185 = FACE_OUTER_BOUND ( 'NONE', #111314, .T. ) ;
#85186 = EDGE_LOOP ( 'NONE', ( #99572, #14184, #50876, #12514 ) ) ;
#85187 = DIRECTION ( 'NONE',  ( -0.000000000000000000, 1.000000000000000000, -0.000000000000000000 ) ) ;
#85188 = CARTESIAN_POINT ( 'NONE',  ( -2.700000000000030820, 2.500000000000000000, -3.983716857408426293 ) ) ;
#85189 = CIRCLE ( 'NONE', #66403, 0.1000000000000002554 ) ;
#85190 = CARTESIAN_POINT ( 'NONE',  ( 11.64999999999990266, 12.50000000000000000, -6.495190528383302464 ) ) ;
#85191 = CONICAL_SURFACE ( 'NONE', #51753, 0.1000000000000002554, 0.003490658503988666988 ) ;
#85192 = PLANE ( 'NONE',  #602 ) ;
#85193 = CARTESIAN_POINT ( 'NONE',  ( -14.19999999999998685, 2.500000000000000000, 0.09999999999999989453 ) ) ;
#85194 = CARTESIAN_POINT ( 'NONE',  ( 13.94999999999989448, 2.500000000000000000, -2.611473670974877592 ) ) ;
#85195 = DIRECTION ( 'NONE',  ( 0.000000000000000000, 0.000000000000000000, 1.000000000000000000 ) ) ;
#85196 = DIRECTION ( 'NONE',  ( 0.000000000000000000, 1.000000000000000000, 0.000000000000000000 ) ) ;
#85197 = VECTOR ( 'NONE', #112507, 1000.000000000000000 ) ;
#85198 = ORIENTED_EDGE ( 'NONE', *, *, #45661, .F. ) ;
#85199 = CIRCLE ( 'NONE', #28782, 0.06509327318403741736 ) ;
#85200 = EDGE_LOOP ( 'NONE', ( #45091, #51415, #91617, #114160 ) ) ;
#85201 = DIRECTION ( 'NONE',  ( -4.274815082592931898E-19, -0.9999939076577903929, -0.003490651415223739937 ) ) ;
#85202 = ORIENTED_EDGE ( 'NONE', *, *, #64235, .T. ) ;
#85203 = DIRECTION ( 'NONE',  ( -0.000000000000000000, 1.000000000000000000, -0.000000000000000000 ) ) ;
#85205 = ORIENTED_EDGE ( 'NONE', *, *, #65212, .T. ) ;
#85204 = VERTEX_POINT ( 'NONE', #124992 ) ;
#85206 = ORIENTED_EDGE ( 'NONE', *, *, #103206, .F. ) ;
#85207 = CARTESIAN_POINT ( 'NONE',  ( -3.550000000000027356, 12.50000000000000000, -2.446380397790840266 ) ) ;
#85208 = AXIS2_PLACEMENT_3D ( 'NONE', #61693, #10613, #101611 ) ;
#85209 = DIRECTION ( 'NONE',  ( 0.000000000000000000, 0.000000000000000000, -1.000000000000000000 ) ) ;
#85210 = SURFACE_STYLE_FILL_AREA ( #35483 ) ;
#85211 = DIRECTION ( 'NONE',  ( 0.000000000000000000, -0.000000000000000000, 1.000000000000000000 ) ) ;
#85212 = DIRECTION ( 'NONE',  ( 0.000000000000000000, -0.9999939076577903929, 0.003490651415223739937 ) ) ;
#85213 = DIRECTION ( 'NONE',  ( 0.000000000000000000, 0.000000000000000000, 1.000000000000000000 ) ) ;
#85214 = VECTOR ( 'NONE', #78986, 1000.000000000000000 ) ;
#85215 = EDGE_LOOP ( 'NONE', ( #86022, #128826 ) ) ;
#85216 = ADVANCED_FACE ( 'NONE', ( #103424 ), #13734, .T. ) ;
#85217 = DIRECTION ( 'NONE',  ( 0.000000000000000000, 0.000000000000000000, 1.000000000000000000 ) ) ;
#85218 = VERTEX_POINT ( 'NONE', #114514 ) ;
#85219 = ADVANCED_FACE ( 'NONE', ( #24861 ), #64133, .T. ) ;
#85220 = CIRCLE ( 'NONE', #51778, 0.1000000000000000472 ) ;
#85221 = ORIENTED_EDGE ( 'NONE', *, *, #110569, .F. ) ;
#85222 = ORIENTED_EDGE ( 'NONE', *, *, #29533, .F. ) ;
#85223 = EDGE_CURVE ( 'NONE', #27204, #37524, #79132, .T. ) ;
#85224 = CIRCLE ( 'NONE', #45527, 0.09999999999999982514 ) ;
#85225 = PLANE ( 'NONE',  #107034 ) ;
#85226 = EDGE_LOOP ( 'NONE', ( #35788, #25545 ) ) ;
#85227 = ORIENTED_EDGE ( 'NONE', *, *, #5232, .T. ) ;
#85228 = ORIENTED_EDGE ( 'NONE', *, *, #72619, .T. ) ;
#85229 = CIRCLE ( 'NONE', #60120, 0.1000000000000000472 ) ;
#85231 = DIRECTION ( 'NONE',  ( 0.000000000000000000, 0.000000000000000000, -1.000000000000000000 ) ) ;
#85230 = AXIS2_PLACEMENT_3D ( 'NONE', #12423, #52358, #92271 ) ;
#85232 = EDGE_CURVE ( 'NONE', #106006, #73789, #34038, .T. ) ;
#85233 = CARTESIAN_POINT ( 'NONE',  ( 1.249999999999953815, 12.50000000000000000, 1.472243186433545459 ) ) ;
#85235 = CIRCLE ( 'NONE', #24694, 0.06509327318403745899 ) ;
#85234 = DIRECTION ( 'NONE',  ( 0.000000000000000000, 0.000000000000000000, 1.000000000000000000 ) ) ;
#85236 = CARTESIAN_POINT ( 'NONE',  ( -9.800000000000007816, 12.50000000000000000, -3.983716857408421852 ) ) ;
#85237 = CARTESIAN_POINT ( 'NONE',  ( -5.850000000000019185, 2.500000000000000000, 6.395190528383296602 ) ) ;
#85238 = DIRECTION ( 'NONE',  ( 0.000000000000000000, -0.000000000000000000, 1.000000000000000000 ) ) ;
#85239 = EDGE_LOOP ( 'NONE', ( #111768, #8681, #30313, #11540 ) ) ;
#85240 = AXIS2_PLACEMENT_3D ( 'NONE', #99038, #21113, #110780 ) ;
#85242 = AXIS2_PLACEMENT_3D ( 'NONE', #121405, #101777, #52038 ) ;
#85241 = CARTESIAN_POINT ( 'NONE',  ( 11.44999999999991047, 12.50000000000000000, -2.511473670974877948 ) ) ;
#85243 = ORIENTED_EDGE ( 'NONE', *, *, #48750, .T. ) ;
#85244 = AXIS2_PLACEMENT_3D ( 'NONE', #70967, #22536, #110878 ) ;
#85245 = DIRECTION ( 'NONE',  ( 0.000000000000000000, -0.000000000000000000, 1.000000000000000000 ) ) ;
#85246 = ORIENTED_EDGE ( 'NONE', *, *, #64738, .F. ) ;
#85247 = CARTESIAN_POINT ( 'NONE',  ( 7.099999999999928590, 2.500000000000000000, -5.122947341949753763 ) ) ;
#85248 = ORIENTED_EDGE ( 'NONE', *, *, #61075, .F. ) ;
#85249 = AXIS2_PLACEMENT_3D ( 'NONE', #36461, #76373, #94073 ) ;
#85250 = EDGE_CURVE ( 'NONE', #101710, #63288, #85458, .T. ) ;
#85251 = ORIENTED_EDGE ( 'NONE', *, *, #20288, .F. ) ;
#85252 = PLANE ( 'NONE',  #9376 ) ;
#85253 = CARTESIAN_POINT ( 'NONE',  ( 14.59999999999989484, 2.500000000000000000, -0.5928203230275541635 ) ) ;
#85255 = VECTOR ( 'NONE', #47306, 1000.000000000000000 ) ;
#85254 = AXIS2_PLACEMENT_3D ( 'NONE', #4087, #45968, #45325 ) ;
#85256 = CARTESIAN_POINT ( 'NONE',  ( -6.050000000000020250, 2.500000000000000000, -2.511473670974877948 ) ) ;
#85257 = LINE ( 'NONE', #36169, #26179 ) ;
#85258 = ORIENTED_EDGE ( 'NONE', *, *, #66760, .F. ) ;
#85259 = DIRECTION ( 'NONE',  ( 0.000000000000000000, 1.000000000000000000, 0.000000000000000000 ) ) ;
#85260 = DIRECTION ( 'NONE',  ( -0.000000000000000000, -1.000000000000000000, -0.000000000000000000 ) ) ;
#85261 = PLANE ( 'NONE',  #106638 ) ;
#85262 = DIRECTION ( 'NONE',  ( 0.000000000000000000, 0.000000000000000000, -1.000000000000000000 ) ) ;
#85263 = DIRECTION ( 'NONE',  ( 0.000000000000000000, 0.000000000000000000, -1.000000000000000000 ) ) ;
#85264 = EDGE_LOOP ( 'NONE', ( #2802, #98190, #48148, #42304 ) ) ;
#85265 = EDGE_CURVE ( 'NONE', #71725, #126533, #35970, .T. ) ;
#85266 = ORIENTED_EDGE ( 'NONE', *, *, #47238, .T. ) ;
#85267 = ORIENTED_EDGE ( 'NONE', *, *, #29345, .T. ) ;
#85268 = DIRECTION ( 'NONE',  ( 0.000000000000000000, 0.000000000000000000, 1.000000000000000000 ) ) ;
#85269 = DIRECTION ( 'NONE',  ( 0.000000000000000000, 0.000000000000000000, 1.000000000000000000 ) ) ;
#85270 = CIRCLE ( 'NONE', #35125, 0.1000000000000002554 ) ;
#85271 = CARTESIAN_POINT ( 'NONE',  ( 183.9218750003414016, 0.000000000000000000, 7.564683531250000925 ) ) ;
#85272 = FACE_OUTER_BOUND ( 'NONE', #126962, .T. ) ;
#85273 = DIRECTION ( 'NONE',  ( -0.000000000000000000, -1.000000000000000000, -0.000000000000000000 ) ) ;
#85274 = EDGE_CURVE ( 'NONE', #112496, #26891, #70795, .T. ) ;
#85275 = CARTESIAN_POINT ( 'NONE',  ( -4.250072516143177381E-14, 2.500000000000000000, -3.637306695894650055 ) ) ;
#85276 = CARTESIAN_POINT ( 'NONE',  ( 11.84999999999990372, 2.500000000000000000, -6.741600689897078169 ) ) ;
#85277 = ORIENTED_EDGE ( 'NONE', *, *, #75378, .T. ) ;
#85278 = AXIS2_PLACEMENT_3D ( 'NONE', #55121, #53827, #93757 ) ;
#85279 = AXIS2_PLACEMENT_3D ( 'NONE', #26372, #116667, #115355 ) ;
#85280 = CARTESIAN_POINT ( 'NONE',  ( 0.8499999999999545697, 2.500000000000000000, -1.472243186433550122 ) ) ;
#85281 = CARTESIAN_POINT ( 'NONE',  ( -12.04999999999999538, 12.50000000000000000, 6.560283801567334372 ) ) ;
#85282 = ORIENTED_EDGE ( 'NONE', *, *, #6961, .F. ) ;
#85283 = EDGE_CURVE ( 'NONE', #62002, #95428, #70897, .T. ) ;
#85284 = DIRECTION ( 'NONE',  ( 0.000000000000000000, 1.000000000000000000, 0.000000000000000000 ) ) ;
#85285 = CARTESIAN_POINT ( 'NONE',  ( 10.44999999999991047, 12.50000000000000000, 2.165063509461097713 ) ) ;
#85286 = CONICAL_SURFACE ( 'NONE', #49716, 0.1000000000000002554, 0.003490658503988666988 ) ;
#85287 = DIRECTION ( 'NONE',  ( 0.000000000000000000, 0.000000000000000000, -1.000000000000000000 ) ) ;
#85288 = CONICAL_SURFACE ( 'NONE', #116678, 0.1000000000000000472, 0.003490658503988666988 ) ;
#85289 = ORIENTED_EDGE ( 'NONE', *, *, #45463, .F. ) ;
#85290 = DIRECTION ( 'NONE',  ( 0.000000000000000000, -0.9999939076577903929, 0.003490651415223739937 ) ) ;
#85291 = ORIENTED_EDGE ( 'NONE', *, *, #125096, .T. ) ;
#85292 = FACE_OUTER_BOUND ( 'NONE', #44323, .T. ) ;
#85293 = FACE_OUTER_BOUND ( 'NONE', #47229, .T. ) ;
#85294 = ORIENTED_EDGE ( 'NONE', *, *, #107796, .F. ) ;
#85295 = DIRECTION ( 'NONE',  ( 0.000000000000000000, 1.000000000000000000, 0.000000000000000000 ) ) ;
#85296 = ADVANCED_FACE ( 'NONE', ( #115811 ), #87505, .T. ) ;
#85297 = CARTESIAN_POINT ( 'NONE',  ( -1.900000000000034106, 2.500000000000000000, 0.3464101615137735735 ) ) ;
#85298 = AXIS2_PLACEMENT_3D ( 'NONE', #36967, #38260, #19231 ) ;
#85299 = ORIENTED_EDGE ( 'NONE', *, *, #66115, .F. ) ;
#85300 = DIRECTION ( 'NONE',  ( 0.000000000000000000, 0.000000000000000000, -1.000000000000000000 ) ) ;
#85301 = EDGE_CURVE ( 'NONE', #87786, #94540, #117085, .T. ) ;
#85302 = AXIS2_PLACEMENT_3D ( 'NONE', #62298, #121196, #79360 ) ;
#85303 = ORIENTED_EDGE ( 'NONE', *, *, #10020, .T. ) ;
#85304 = VERTEX_POINT ( 'NONE', #58833 ) ;
#85305 = AXIS2_PLACEMENT_3D ( 'NONE', #19181, #62370, #100986 ) ;
#85306 = PLANE ( 'NONE',  #27517 ) ;
#85307 = CARTESIAN_POINT ( 'NONE',  ( -1.250000000000036193, 12.50000000000000000, 5.802370205355744659 ) ) ;
#85308 = EDGE_CURVE ( 'NONE', #117873, #89637, #14433, .T. ) ;
#85309 = EDGE_CURVE ( 'NONE', #124116, #47422, #58290, .T. ) ;
#85310 = ORIENTED_EDGE ( 'NONE', *, *, #985, .T. ) ;
#85311 = EDGE_CURVE ( 'NONE', #24620, #124866, #100145, .T. ) ;
#85312 = AXIS2_PLACEMENT_3D ( 'NONE', #72193, #72827, #4070 ) ;
#85313 = EDGE_CURVE ( 'NONE', #29034, #126026, #9081, .T. ) ;
#85314 = CARTESIAN_POINT ( 'NONE',  ( -15.39999999999997904, 12.50000000000000000, -0.6928203230275519209 ) ) ;
#85315 = DIRECTION ( 'NONE',  ( -0.000000000000000000, 1.000000000000000000, -0.000000000000000000 ) ) ;
#85316 = AXIS2_PLACEMENT_3D ( 'NONE', #102754, #72671, #43223 ) ;
#85317 = EDGE_LOOP ( 'NONE', ( #19077, #81602, #127193, #72661 ) ) ;
#85318 = CARTESIAN_POINT ( 'NONE',  ( -12.89999999999999147, 12.50000000000000000, -0.6928203230275500335 ) ) ;
#85319 = DIRECTION ( 'NONE',  ( -0.000000000000000000, -1.000000000000000000, -0.000000000000000000 ) ) ;
#85320 = EDGE_CURVE ( 'NONE', #45027, #6696, #16303, .T. ) ;
#85321 = DIRECTION ( 'NONE',  ( -0.000000000000000000, -1.000000000000000000, -0.000000000000000000 ) ) ;
#85322 = DIRECTION ( 'NONE',  ( 0.000000000000000000, 0.000000000000000000, -1.000000000000000000 ) ) ;
#85323 = EDGE_CURVE ( 'NONE', #66996, #1899, #114704, .T. ) ;
#85324 = DIRECTION ( 'NONE',  ( 0.000000000000000000, 1.000000000000000000, 0.000000000000000000 ) ) ;
#85325 = CONICAL_SURFACE ( 'NONE', #1411, 0.09999999999999982514, 0.003490658503988666988 ) ;
#85326 = DIRECTION ( 'NONE',  ( 0.000000000000000000, -0.9999939076577903929, 0.003490651415223739937 ) ) ;
#85327 = EDGE_CURVE ( 'NONE', #25449, #95824, #60455, .T. ) ;
#85328 = ADVANCED_FACE ( 'NONE', ( #88939 ), #8425, .T. ) ;
#85329 = EDGE_CURVE ( 'NONE', #78151, #16115, #128889, .T. ) ;
#85330 = EDGE_LOOP ( 'NONE', ( #110083, #101526, #1497, #94453 ) ) ;
#85331 = VERTEX_POINT ( 'NONE', #16929 ) ;
#85332 = VERTEX_POINT ( 'NONE', #47092 ) ;
#85333 = ORIENTED_EDGE ( 'NONE', *, *, #102502, .T. ) ;
#85334 = DIRECTION ( 'NONE',  ( 0.000000000000000000, 1.000000000000000000, 0.000000000000000000 ) ) ;
#85335 = DIRECTION ( 'NONE',  ( 1.000000000000000000, -0.000000000000000000, -0.000000000000000000 ) ) ;
#85336 = CARTESIAN_POINT ( 'NONE',  ( -6.650000000000018119, 2.500000000000000000, -6.595190528383302109 ) ) ;
#85337 = VECTOR ( 'NONE', #51212, 1000.000000000000000 ) ;
#85338 = VERTEX_POINT ( 'NONE', #106636 ) ;
#85339 = FACE_BOUND ( 'NONE', #59619, .T. ) ;
#85340 = ADVANCED_FACE ( 'NONE', ( #79129 ), #1835, .T. ) ;
#85341 = DIRECTION ( 'NONE',  ( 0.000000000000000000, 0.000000000000000000, 1.000000000000000000 ) ) ;
#85342 = DIRECTION ( 'NONE',  ( 0.000000000000000000, -0.9999939076577903929, 0.003490651415223739937 ) ) ;
#85343 = DIRECTION ( 'NONE',  ( 0.000000000000000000, 0.000000000000000000, -1.000000000000000000 ) ) ;
#85345 = AXIS2_PLACEMENT_3D ( 'NONE', #24282, #2049, #21711 ) ;
#85344 = CONICAL_SURFACE ( 'NONE', #110380, 0.1000000000000002554, 0.003490658503988666988 ) ;
#85346 = DIRECTION ( 'NONE',  ( 0.000000000000000000, 0.000000000000000000, 1.000000000000000000 ) ) ;
#85347 = DIRECTION ( 'NONE',  ( -0.000000000000000000, 1.000000000000000000, -0.000000000000000000 ) ) ;
#85348 = LINE ( 'NONE', #104965, #1602 ) ;
#85349 = LINE ( 'NONE', #15943, #55877 ) ;
#85350 = DIRECTION ( 'NONE',  ( -0.000000000000000000, -1.000000000000000000, -0.000000000000000000 ) ) ;
#85351 = DIRECTION ( 'NONE',  ( 0.000000000000000000, 0.000000000000000000, -1.000000000000000000 ) ) ;
#85352 = CARTESIAN_POINT ( 'NONE',  ( -13.34999999999999076, 2.500000000000000000, 1.372243186433549367 ) ) ;
#85353 = ORIENTED_EDGE ( 'NONE', *, *, #31418, .T. ) ;
#85354 = ORIENTED_EDGE ( 'NONE', *, *, #55480, .F. ) ;
#85355 = ORIENTED_EDGE ( 'NONE', *, *, #98914, .F. ) ;
#85356 = ORIENTED_EDGE ( 'NONE', *, *, #72157, .T. ) ;
#85357 = DIRECTION ( 'NONE',  ( 0.000000000000000000, 1.000000000000000000, 0.000000000000000000 ) ) ;
#85358 = ORIENTED_EDGE ( 'NONE', *, *, #119914, .T. ) ;
#85359 = CIRCLE ( 'NONE', #8079, 0.06509327318403745899 ) ;
#85360 = FACE_OUTER_BOUND ( 'NONE', #85639, .T. ) ;
#85361 = ORIENTED_EDGE ( 'NONE', *, *, #68774, .F. ) ;
#85362 = ORIENTED_EDGE ( 'NONE', *, *, #30343, .T. ) ;
#85363 = DIRECTION ( 'NONE',  ( -1.000000000000000000, -0.000000000000000000, -0.000000000000000000 ) ) ;
#85364 = VECTOR ( 'NONE', #95579, 1000.000000000000000 ) ;
#85365 = AXIS2_PLACEMENT_3D ( 'NONE', #64466, #4244, #23917 ) ;
#85366 = CARTESIAN_POINT ( 'NONE',  ( -0.8500000000000386136, 2.500000000000000000, 5.902370205355745192 ) ) ;
#85368 = CARTESIAN_POINT ( 'NONE',  ( 9.599999999999917932, 12.50000000000000000, 0.6928203230275494784 ) ) ;
#85367 = CIRCLE ( 'NONE', #20538, 0.06509327318403745899 ) ;
#85369 = CARTESIAN_POINT ( 'NONE',  ( 12.49999999999993960, 2.500000000000000000, -4.230127018922201998 ) ) ;
#85370 = ORIENTED_EDGE ( 'NONE', *, *, #3434, .T. ) ;
#85371 = CIRCLE ( 'NONE', #28955, 0.1000000000000000056 ) ;
#85372 = CIRCLE ( 'NONE', #93793, 0.06509327318403741736 ) ;
#85373 = ORIENTED_EDGE ( 'NONE', *, *, #73494, .F. ) ;
#85374 = ADVANCED_FACE ( 'NONE', ( #107281 ), #118388, .T. ) ;
#85375 = CIRCLE ( 'NONE', #41495, 0.1000000000000002554 ) ;
#85376 = EDGE_LOOP ( 'NONE', ( #71930, #121320 ) ) ;
#85378 = EDGE_LOOP ( 'NONE', ( #22773, #101718 ) ) ;
#85377 = DIRECTION ( 'NONE',  ( 0.000000000000000000, 0.000000000000000000, 1.000000000000000000 ) ) ;
#85379 = EDGE_CURVE ( 'NONE', #120770, #82540, #73491, .T. ) ;
#85380 = CARTESIAN_POINT ( 'NONE',  ( 13.34999999999990017, 2.500000000000000000, 2.957883832488649389 ) ) ;
#85381 = EDGE_LOOP ( 'NONE', ( #129154, #82342, #18729, #83577 ) ) ;
#85382 = ORIENTED_EDGE ( 'NONE', *, *, #87733, .T. ) ;
#85383 = AXIS2_PLACEMENT_3D ( 'NONE', #118305, #98013, #109109 ) ;
#85384 = DIRECTION ( 'NONE',  ( 0.000000000000000000, 0.000000000000000000, -1.000000000000000000 ) ) ;
#85385 = EDGE_CURVE ( 'NONE', #29210, #112782, #108442, .T. ) ;
#85386 = CIRCLE ( 'NONE', #74927, 0.06509327318403745899 ) ;
#85387 = CARTESIAN_POINT ( 'NONE',  ( -13.74999999999998757, 2.500000000000000000, -2.957883832488651610 ) ) ;
#85388 = DIRECTION ( 'NONE',  ( -0.000000000000000000, -1.000000000000000000, -0.000000000000000000 ) ) ;
#85389 = DIRECTION ( 'NONE',  ( -1.000000000000000000, 0.000000000000000000, 0.000000000000000000 ) ) ;
#85390 = DIRECTION ( 'NONE',  ( 0.000000000000000000, -0.000000000000000000, 1.000000000000000000 ) ) ;
#85391 = CARTESIAN_POINT ( 'NONE',  ( 7.099999999999928590, 2.500000000000000000, 4.330127018922196314 ) ) ;
#85392 = EDGE_LOOP ( 'NONE', ( #92455, #28149 ) ) ;
#85393 = FACE_OUTER_BOUND ( 'NONE', #94867, .T. ) ;
#85394 = CIRCLE ( 'NONE', #41511, 0.1000000000000002554 ) ;
#85395 = VERTEX_POINT ( 'NONE', #119045 ) ;
#85396 = CARTESIAN_POINT ( 'NONE',  ( 7.899999999999923084, 2.500000000000000000, 0.6928203230275494784 ) ) ;
#85397 = ORIENTED_EDGE ( 'NONE', *, *, #30711, .T. ) ;
#85398 = PLANE ( 'NONE',  #84949 ) ;
#85399 = PLANE ( 'NONE',  #53262 ) ;
#85400 = AXIS2_PLACEMENT_3D ( 'NONE', #126571, #29025, #68926 ) ;
#85401 = AXIS2_PLACEMENT_3D ( 'NONE', #6658, #96349, #127760 ) ;
#85402 = EDGE_LOOP ( 'NONE', ( #155, #16, #1308, #13250 ) ) ;
#85403 = DIRECTION ( 'NONE',  ( 0.000000000000000000, 0.000000000000000000, 1.000000000000000000 ) ) ;
#85404 = DIRECTION ( 'NONE',  ( 0.000000000000000000, 0.000000000000000000, 1.000000000000000000 ) ) ;
#85405 = ORIENTED_EDGE ( 'NONE', *, *, #57837, .T. ) ;
#85407 = VECTOR ( 'NONE', #18273, 1000.000000000000000 ) ;
#85406 = CARTESIAN_POINT ( 'NONE',  ( 2.899999999999943956, 12.50000000000000000, 4.395220292106234439 ) ) ;
#85408 = DIRECTION ( 'NONE',  ( 0.000000000000000000, 0.000000000000000000, 1.000000000000000000 ) ) ;
#85409 = EDGE_LOOP ( 'NONE', ( #51773, #26253 ) ) ;
#85410 = ORIENTED_EDGE ( 'NONE', *, *, #56479, .T. ) ;
#85411 = DIRECTION ( 'NONE',  ( -0.000000000000000000, 1.000000000000000000, -0.000000000000000000 ) ) ;
#85412 = CARTESIAN_POINT ( 'NONE',  ( -12.09999999999999432, 2.500000000000000000, 5.022947341949748790 ) ) ;
#85413 = CARTESIAN_POINT ( 'NONE',  ( 185.3385416670080872, 6.551208109652274736, 3.782341765625001351 ) ) ;
#85415 = VECTOR ( 'NONE', #1027, 1000.000000000000000 ) ;
#85414 = DIRECTION ( 'NONE',  ( -0.000000000000000000, 1.000000000000000000, -0.000000000000000000 ) ) ;
#85416 = EDGE_CURVE ( 'NONE', #15482, #84687, #96166, .T. ) ;
#85417 = AXIS2_PLACEMENT_3D ( 'NONE', #27017, #79347, #108141 ) ;
#85418 = CARTESIAN_POINT ( 'NONE',  ( 13.09999999999990195, 12.50000000000000000, -4.741630453620016006 ) ) ;
#85419 = DIRECTION ( 'NONE',  ( 0.000000000000000000, 0.000000000000000000, -1.000000000000000000 ) ) ;
#85420 = AXIS2_PLACEMENT_3D ( 'NONE', #103553, #83888, #74080 ) ;
#85421 = VERTEX_POINT ( 'NONE', #26792 ) ;
#85422 = CARTESIAN_POINT ( 'NONE',  ( 26.76179944288227475, 1.073660921396622614, -4.445808334545023222 ) ) ;
#85423 = ORIENTED_EDGE ( 'NONE', *, *, #23125, .T. ) ;
#85424 = AXIS2_PLACEMENT_3D ( 'NONE', #69352, #41857, #101414 ) ;
#85425 = EDGE_CURVE ( 'NONE', #12748, #90660, #89674, .T. ) ;
#85426 = CONICAL_SURFACE ( 'NONE', #106356, 0.1000000000000002554, 0.003490658503988666988 ) ;
#85427 = DIRECTION ( 'NONE',  ( 0.000000000000000000, 0.000000000000000000, 1.000000000000000000 ) ) ;
#85428 = DIRECTION ( 'NONE',  ( 0.000000000000000000, -0.9999939076577903929, 0.003490651415223739937 ) ) ;
#85429 = EDGE_CURVE ( 'NONE', #118375, #88991, #52241, .T. ) ;
#85430 = DIRECTION ( 'NONE',  ( -0.000000000000000000, 1.000000000000000000, -0.000000000000000000 ) ) ;
#85431 = VERTEX_POINT ( 'NONE', #92149 ) ;
#85433 = CIRCLE ( 'NONE', #6002, 0.06509327318403745899 ) ;
#85432 = CIRCLE ( 'NONE', #58260, 0.1000000000000002554 ) ;
#85434 = DIRECTION ( 'NONE',  ( 0.000000000000000000, 0.000000000000000000, 1.000000000000000000 ) ) ;
#85435 = DIRECTION ( 'NONE',  ( 0.000000000000000000, -0.000000000000000000, 1.000000000000000000 ) ) ;
#85436 = EDGE_CURVE ( 'NONE', #116432, #22907, #60769, .T. ) ;
#85437 = EDGE_LOOP ( 'NONE', ( #6027, #75369, #17532, #33349 ) ) ;
#85438 = CARTESIAN_POINT ( 'NONE',  ( 3.749999999999976907, 2.500000000000000000, 2.165063509461097713 ) ) ;
#85439 = EDGE_LOOP ( 'NONE', ( #11755, #38574, #38681, #41277 ) ) ;
#85440 = ORIENTED_EDGE ( 'NONE', *, *, #100239, .T. ) ;
#85441 = CARTESIAN_POINT ( 'NONE',  ( -2.500000000000032863, 2.500000000000000000, 5.022947341949748790 ) ) ;
#85442 = AXIS2_PLACEMENT_3D ( 'NONE', #66646, #16872, #96746 ) ;
#85443 = ORIENTED_EDGE ( 'NONE', *, *, #8951, .T. ) ;
#85444 = DIRECTION ( 'NONE',  ( 0.000000000000000000, -0.9999939076577903929, 0.003490651415223739937 ) ) ;
#85445 = CARTESIAN_POINT ( 'NONE',  ( -12.49999999999995737, 2.500000000000000000, 4.330127018922196314 ) ) ;
#85446 = DIRECTION ( 'NONE',  ( 0.000000000000000000, 0.000000000000000000, 1.000000000000000000 ) ) ;
#85447 = ORIENTED_EDGE ( 'NONE', *, *, #101532, .T. ) ;
#85448 = AXIS2_PLACEMENT_3D ( 'NONE', #37943, #107972, #20239 ) ;
#85449 = FACE_BOUND ( 'NONE', #116713, .T. ) ;
#85450 = AXIS2_PLACEMENT_3D ( 'NONE', #86024, #51304, #80754 ) ;
#85451 = AXIS2_PLACEMENT_3D ( 'NONE', #43715, #52869, #2453 ) ;
#85453 = ORIENTED_EDGE ( 'NONE', *, *, #90171, .F. ) ;
#85452 = CARTESIAN_POINT ( 'NONE',  ( -6.700000000000019718, 2.500000000000000000, -4.330127018922201643 ) ) ;
#85454 = DIRECTION ( 'NONE',  ( 0.000000000000000000, -0.000000000000000000, 1.000000000000000000 ) ) ;
#85455 = DIRECTION ( 'NONE',  ( 0.000000000000000000, 0.000000000000000000, 1.000000000000000000 ) ) ;
#85456 = AXIS2_PLACEMENT_3D ( 'NONE', #83502, #33739, #86707 ) ;
#85457 = ORIENTED_EDGE ( 'NONE', *, *, #115973, .T. ) ;
#85458 = CIRCLE ( 'NONE', #79221, 0.1000000000000000472 ) ;
#85459 = ADVANCED_FACE ( 'NONE', ( #69943 ), #90201, .T. ) ;
#85460 = CONICAL_SURFACE ( 'NONE', #43729, 0.1000000000000002554, 0.003490658503988666988 ) ;
#85461 = VERTEX_POINT ( 'NONE', #120334 ) ;
#85462 = ORIENTED_EDGE ( 'NONE', *, *, #81361, .F. ) ;
#85463 = LINE ( 'NONE', #75010, #60810 ) ;
#85464 = CARTESIAN_POINT ( 'NONE',  ( 2.500000000000002220, 1.499999999999999556, 10.00000000000000533 ) ) ;
#85465 = CARTESIAN_POINT ( 'NONE',  ( -10.65000000000000213, 2.500000000000000000, 1.718653347947321386 ) ) ;
#85466 = ADVANCED_FACE ( 'NONE', ( #2465 ), #16490, .T. ) ;
#85467 = FACE_BOUND ( 'NONE', #115580, .T. ) ;
#85468 = ORIENTED_EDGE ( 'NONE', *, *, #20282, .T. ) ;
#85469 = CARTESIAN_POINT ( 'NONE',  ( 184.9010416670080588, -4.367472073101519747, 7.564683531249999149 ) ) ;
#85471 = EDGE_CURVE ( 'NONE', #60027, #91650, #52030, .T. ) ;
#85470 = VECTOR ( 'NONE', #124099, 1000.000000000000000 ) ;
#85472 = CARTESIAN_POINT ( 'NONE',  ( -10.85000000000000142, 2.500000000000000000, 6.395190528383296602 ) ) ;
#85473 = DIRECTION ( 'NONE',  ( 0.000000000000000000, -0.000000000000000000, 1.000000000000000000 ) ) ;
#85474 = CONICAL_SURFACE ( 'NONE', #33274, 0.1000000000000002554, 0.003490658503988666988 ) ;
#85475 = CARTESIAN_POINT ( 'NONE',  ( 184.9166666666666856, 6.668395609140176816, 3.850000000000000977 ) ) ;
#85476 = ADVANCED_FACE ( 'NONE', ( #101341 ), #110504, .T. ) ;
#85477 = CARTESIAN_POINT ( 'NONE',  ( 0.6499999999999543920, 12.50000000000000000, 6.841600689897072485 ) ) ;
#85478 = ADVANCED_FACE ( 'NONE', ( #1832 ), #122274, .T. ) ;
#85479 = CARTESIAN_POINT ( 'NONE',  ( -9.999999999999969802, 12.50000000000000000, 4.330127018922196314 ) ) ;
#85480 = EDGE_CURVE ( 'NONE', #9421, #55696, #123124, .T. ) ;
#85481 = DIRECTION ( 'NONE',  ( 0.000000000000000000, -0.000000000000000000, 1.000000000000000000 ) ) ;
#85482 = CARTESIAN_POINT ( 'NONE',  ( 1.049999999999953637, 12.50000000000000000, 2.446380397790835826 ) ) ;
#85483 = CIRCLE ( 'NONE', #70811, 0.06509327318403745899 ) ;
#85484 = DIRECTION ( 'NONE',  ( 0.000000000000000000, 1.000000000000000000, 0.000000000000000000 ) ) ;
#85485 = ADVANCED_FACE ( 'NONE', ( #109204 ), #66670, .T. ) ;
#85486 = EDGE_LOOP ( 'NONE', ( #46105, #12742 ) ) ;
#85487 = ORIENTED_EDGE ( 'NONE', *, *, #37254, .F. ) ;
#85488 = ORIENTED_EDGE ( 'NONE', *, *, #35223, .F. ) ;
#85489 = ORIENTED_EDGE ( 'NONE', *, *, #1260, .F. ) ;
#85490 = ORIENTED_EDGE ( 'NONE', *, *, #67434, .T. ) ;
#85491 = AXIS2_PLACEMENT_3D ( 'NONE', #89766, #93, #7003 ) ;
#85492 = FACE_OUTER_BOUND ( 'NONE', #8445, .T. ) ;
#85493 = DIRECTION ( 'NONE',  ( 0.000000000000000000, 0.000000000000000000, -1.000000000000000000 ) ) ;
#85494 = EDGE_LOOP ( 'NONE', ( #105237, #48865 ) ) ;
#85495 = FACE_BOUND ( 'NONE', #123349, .T. ) ;
#85496 = EDGE_CURVE ( 'NONE', #76941, #82898, #10253, .T. ) ;
#85497 = DIRECTION ( 'NONE',  ( 0.000000000000000000, 1.000000000000000000, 0.000000000000000000 ) ) ;
#85498 = AXIS2_PLACEMENT_3D ( 'NONE', #72390, #112941, #41007 ) ;
#85499 = CARTESIAN_POINT ( 'NONE',  ( -9.150000000000009237, 12.50000000000000000, -7.188010851410848723 ) ) ;
#85500 = ORIENTED_EDGE ( 'NONE', *, *, #71387, .T. ) ;
#85501 = DIRECTION ( 'NONE',  ( -0.000000000000000000, 1.000000000000000000, -0.000000000000000000 ) ) ;
#85502 = CARTESIAN_POINT ( 'NONE',  ( 2.699999999999947331, 12.50000000000000000, -0.3464101615137783474 ) ) ;
#85503 = CARTESIAN_POINT ( 'NONE',  ( -8.750000000000010658, 12.50000000000000000, -7.188010851410848723 ) ) ;
#85504 = ORIENTED_EDGE ( 'NONE', *, *, #98313, .T. ) ;
#85505 = DIRECTION ( 'NONE',  ( 0.000000000000000000, 1.000000000000000000, 0.000000000000000000 ) ) ;
#85507 = VERTEX_POINT ( 'NONE', #89580 ) ;
#85506 = AXIS2_PLACEMENT_3D ( 'NONE', #88326, #28797, #18947 ) ;
#85508 = ORIENTED_EDGE ( 'NONE', *, *, #71396, .F. ) ;
#85509 = EDGE_LOOP ( 'NONE', ( #91835, #79292, #41917, #30587 ) ) ;
#85510 = CARTESIAN_POINT ( 'NONE',  ( -2.950000000000030376, 12.50000000000000000, 6.560283801567334372 ) ) ;
#85511 = DIRECTION ( 'NONE',  ( 0.000000000000000000, 0.000000000000000000, 1.000000000000000000 ) ) ;
#85512 = FACE_OUTER_BOUND ( 'NONE', #13392, .T. ) ;
#85513 = VECTOR ( 'NONE', #114190, 1000.000000000000000 ) ;
#85514 = VERTEX_POINT ( 'NONE', #10374 ) ;
#85515 = CARTESIAN_POINT ( 'NONE',  ( 14.38463633427375576, 1.500000000000064171, -7.683002070836549180 ) ) ;
#85516 = CARTESIAN_POINT ( 'NONE',  ( -8.100000000000010303, 2.500000000000000000, 4.676537180435972552 ) ) ;
#85519 = AXIS2_PLACEMENT_3D ( 'NONE', #55538, #73238, #123607 ) ;
#85518 = FACE_OUTER_BOUND ( 'NONE', #128559, .T. ) ;
#85517 = AXIS2_PLACEMENT_3D ( 'NONE', #93005, #3960, #42627 ) ;
#85520 = CARTESIAN_POINT ( 'NONE',  ( 184.8229166673494603, -4.445597072760122614, 7.699999999999998401 ) ) ;
#85521 = DIRECTION ( 'NONE',  ( 0.000000000000000000, 0.000000000000000000, 1.000000000000000000 ) ) ;
#85522 = CIRCLE ( 'NONE', #45824, 0.1000000000000002554 ) ;
#85523 = PLANE ( 'NONE',  #68353 ) ;
#85524 = ORIENTED_EDGE ( 'NONE', *, *, #114808, .F. ) ;
#85525 = CARTESIAN_POINT ( 'NONE',  ( 1.449999999999951328, 12.50000000000000000, 2.446380397790835826 ) ) ;
#85527 = AXIS2_PLACEMENT_3D ( 'NONE', #68536, #1724, #119564 ) ;
#85526 = CIRCLE ( 'NONE', #62561, 0.1000000000000002554 ) ;
#85528 = VERTEX_POINT ( 'NONE', #1196 ) ;
#85529 = EDGE_CURVE ( 'NONE', #81382, #26297, #68737, .T. ) ;
#85530 = ORIENTED_EDGE ( 'NONE', *, *, #24573, .F. ) ;
#85531 = FACE_OUTER_BOUND ( 'NONE', #64372, .T. ) ;
#85532 = CARTESIAN_POINT ( 'NONE',  ( -4.200000000000029488, 2.500000000000000000, -4.330127018922201643 ) ) ;
#85533 = DIRECTION ( 'NONE',  ( -4.274815082592931898E-19, -0.9999939076577903929, -0.003490651415223739937 ) ) ;
#85534 = ORIENTED_EDGE ( 'NONE', *, *, #66760, .T. ) ;
#85535 = VERTEX_POINT ( 'NONE', #99414 ) ;
#85536 = EDGE_CURVE ( 'NONE', #107774, #118072, #104251, .T. ) ;
#85537 = DIRECTION ( 'NONE',  ( 0.000000000000000000, 0.000000000000000000, 1.000000000000000000 ) ) ;
#85538 = DIRECTION ( 'NONE',  ( 0.000000000000000000, 0.000000000000000000, -1.000000000000000000 ) ) ;
#85539 = DIRECTION ( 'NONE',  ( -0.000000000000000000, -1.000000000000000000, -0.000000000000000000 ) ) ;
#85541 = EDGE_LOOP ( 'NONE', ( #93566, #48316 ) ) ;
#85540 = CONICAL_SURFACE ( 'NONE', #31271, 0.1000000000000002554, 0.003490658503988666988 ) ;
#85542 = EDGE_LOOP ( 'NONE', ( #74480, #128774 ) ) ;
#85543 = DIRECTION ( 'NONE',  ( 0.000000000000000000, 0.000000000000000000, 1.000000000000000000 ) ) ;
#85544 = ORIENTED_EDGE ( 'NONE', *, *, #28022, .F. ) ;
#85545 = CARTESIAN_POINT ( 'NONE',  ( -8.100000000000010303, 12.50000000000000000, 4.676537180435972552 ) ) ;
#85547 = PLANE ( 'NONE',  #67920 ) ;
#85546 = VECTOR ( 'NONE', #82375, 1000.000000000000000 ) ;
#85548 = ORIENTED_EDGE ( 'NONE', *, *, #76389, .T. ) ;
#85549 = DIRECTION ( 'NONE',  ( 0.000000000000000000, 0.000000000000000000, 1.000000000000000000 ) ) ;
#85550 = LINE ( 'NONE', #63341, #104797 ) ;
#85551 = CARTESIAN_POINT ( 'NONE',  ( -9.350000000000006750, 2.500000000000000000, -2.411473670974877859 ) ) ;
#85552 = DIRECTION ( 'NONE',  ( -0.000000000000000000, 1.000000000000000000, -0.000000000000000000 ) ) ;
#85553 = AXIS2_PLACEMENT_3D ( 'NONE', #102336, #2838, #42797 ) ;
#85554 = ORIENTED_EDGE ( 'NONE', *, *, #73250, .F. ) ;
#85555 = AXIS2_PLACEMENT_3D ( 'NONE', #104553, #114365, #73167 ) ;
#85557 = DIRECTION ( 'NONE',  ( 0.000000000000000000, 0.000000000000000000, 1.000000000000000000 ) ) ;
#85556 = VECTOR ( 'NONE', #93590, 1000.000000000000000 ) ;
#85558 = CARTESIAN_POINT ( 'NONE',  ( 194.5000000000000000, 0.000000000000000000, -4.000000000000000000 ) ) ;
#85559 = VERTEX_POINT ( 'NONE', #49677 ) ;
#85560 = ORIENTED_EDGE ( 'NONE', *, *, #52533, .T. ) ;
#85561 = CARTESIAN_POINT ( 'NONE',  ( -0.8500000000000395017, 2.500000000000000000, 6.595190528383296780 ) ) ;
#85562 = DIRECTION ( 'NONE',  ( 0.000000000000000000, 0.000000000000000000, -1.000000000000000000 ) ) ;
#85563 = DIRECTION ( 'NONE',  ( 0.000000000000000000, 1.000000000000000000, 0.000000000000000000 ) ) ;
#85564 = DIRECTION ( 'NONE',  ( 0.000000000000000000, 0.000000000000000000, -1.000000000000000000 ) ) ;
#85565 = CONICAL_SURFACE ( 'NONE', #26998, 0.09999999999999982514, 0.003490658503988666988 ) ;
#85566 = CARTESIAN_POINT ( 'NONE',  ( 4.599999999999936584, 2.500000000000000000, 3.737306695894644371 ) ) ;
#85567 = CARTESIAN_POINT ( 'NONE',  ( 9.999999999999916511, 2.500000000000000000, -0.6928203230275541413 ) ) ;
#85569 = ADVANCED_FACE ( 'NONE', ( #111125 ), #77151, .T. ) ;
#85568 = AXIS2_PLACEMENT_3D ( 'NONE', #40868, #38939, #80780 ) ;
#85570 = AXIS2_PLACEMENT_3D ( 'NONE', #57781, #39451, #97687 ) ;
#85571 = DIRECTION ( 'NONE',  ( 0.000000000000000000, 0.000000000000000000, 1.000000000000000000 ) ) ;
#85572 = CARTESIAN_POINT ( 'NONE',  ( -1.050000000000038680, 2.500000000000000000, 6.941600689897073018 ) ) ;
#85573 = FACE_OUTER_BOUND ( 'NONE', #98567, .T. ) ;
#85574 = DIRECTION ( 'NONE',  ( -0.000000000000000000, 1.000000000000000000, -0.000000000000000000 ) ) ;
#85575 = CARTESIAN_POINT ( 'NONE',  ( -1.650000000000034328, 12.50000000000000000, -2.099970236277064473 ) ) ;
#85576 = EDGE_CURVE ( 'NONE', #30501, #54077, #47828, .T. ) ;
#85577 = VERTEX_POINT ( 'NONE', #538 ) ;
#85578 = ORIENTED_EDGE ( 'NONE', *, *, #39634, .T. ) ;
#85579 = AXIS2_PLACEMENT_3D ( 'NONE', #119540, #107802, #29888 ) ;
#85580 = EDGE_CURVE ( 'NONE', #115716, #33086, #40506, .T. ) ;
#85581 = ORIENTED_EDGE ( 'NONE', *, *, #112053, .F. ) ;
#85582 = DIRECTION ( 'NONE',  ( 0.000000000000000000, 0.000000000000000000, 1.000000000000000000 ) ) ;
#85583 = EDGE_CURVE ( 'NONE', #117286, #54541, #22795, .T. ) ;
#85584 = LINE ( 'NONE', #107146, #23390 ) ;
#85585 = ORIENTED_EDGE ( 'NONE', *, *, #13761, .F. ) ;
#85586 = CARTESIAN_POINT ( 'NONE',  ( 21.23528140090950700, -2.699413673072311948, -2.293764360948876480 ) ) ;
#85587 = ADVANCED_FACE ( 'NONE', ( #65251 ), #98071, .T. ) ;
#85588 = DIRECTION ( 'NONE',  ( 0.000000000000000000, 0.000000000000000000, -1.000000000000000000 ) ) ;
#85590 = VERTEX_POINT ( 'NONE', #12926 ) ;
#85589 = DIRECTION ( 'NONE',  ( 0.000000000000000000, 0.000000000000000000, 1.000000000000000000 ) ) ;
#85591 = EDGE_CURVE ( 'NONE', #95448, #98294, #47920, .T. ) ;
#85592 = CIRCLE ( 'NONE', #89708, 0.06509327318403745899 ) ;
#85593 = CARTESIAN_POINT ( 'NONE',  ( -2.050000000000032685, 12.50000000000000000, -2.165063509461101710 ) ) ;
#85594 = ORIENTED_EDGE ( 'NONE', *, *, #81033, .T. ) ;
#85595 = ORIENTED_EDGE ( 'NONE', *, *, #115306, .F. ) ;
#85596 = ORIENTED_EDGE ( 'NONE', *, *, #76870, .T. ) ;
#85597 = VERTEX_POINT ( 'NONE', #43087 ) ;
#85598 = DIRECTION ( 'NONE',  ( 0.000000000000000000, 0.000000000000000000, 1.000000000000000000 ) ) ;
#85599 = AXIS2_PLACEMENT_3D ( 'NONE', #2139, #109529, #91172 ) ;
#85600 = CARTESIAN_POINT ( 'NONE',  ( 8.349999999999919709, 2.500000000000000000, 5.702370205355745014 ) ) ;
#85601 = CARTESIAN_POINT ( 'NONE',  ( -12.09999999999999609, 2.500000000000000000, 0.6928203230275535862 ) ) ;
#85602 = DIRECTION ( 'NONE',  ( 0.000000000000000000, 0.000000000000000000, 1.000000000000000000 ) ) ;
#85603 = VERTEX_POINT ( 'NONE', #24711 ) ;
#85605 = AXIS2_PLACEMENT_3D ( 'NONE', #111717, #79674, #121515 ) ;
#85604 = AXIS2_PLACEMENT_3D ( 'NONE', #37145, #106513, #97978 ) ;
#85606 = CARTESIAN_POINT ( 'NONE',  ( -4.600000000000028066, 12.50000000000000000, -5.022947341949754119 ) ) ;
#85607 = ORIENTED_EDGE ( 'NONE', *, *, #67271, .T. ) ;
#85608 = DIRECTION ( 'NONE',  ( 0.000000000000000000, -0.9999939076577903929, 0.003490651415223739937 ) ) ;
#85610 = CIRCLE ( 'NONE', #31253, 0.1000000000000000472 ) ;
#85609 = CARTESIAN_POINT ( 'NONE',  ( 14.69205215096692818, -2.499999999999999112, -6.336420066640019222 ) ) ;
#85611 = DIRECTION ( 'NONE',  ( 0.000000000000000000, 0.000000000000000000, 1.000000000000000000 ) ) ;
#85612 = CARTESIAN_POINT ( 'NONE',  ( 15.86953761860680068, -2.463355995079608451, 3.896699429476443211 ) ) ;
#85613 = ORIENTED_EDGE ( 'NONE', *, *, #30809, .T. ) ;
#85615 = AXIS2_PLACEMENT_3D ( 'NONE', #5582, #57286, #77554 ) ;
#85614 = VECTOR ( 'NONE', #16154, 1000.000000000000000 ) ;
#85616 = EDGE_CURVE ( 'NONE', #54196, #106953, #31199, .T. ) ;
#85617 = VERTEX_POINT ( 'NONE', #45000 ) ;
#85618 = EDGE_LOOP ( 'NONE', ( #79889, #21626, #118031, #108476 ) ) ;
#85619 = LINE ( 'NONE', #125540, #33544 ) ;
#85620 = CARTESIAN_POINT ( 'NONE',  ( -2.100000000000034284, 2.500000000000000000, -4.330127018922201643 ) ) ;
#85621 = CARTESIAN_POINT ( 'NONE',  ( -1.700000000000034817, 2.500000000000000000, -0.1000000000000023925 ) ) ;
#85622 = FACE_BOUND ( 'NONE', #16174, .T. ) ;
#85623 = CARTESIAN_POINT ( 'NONE',  ( 4.199999999999938005, 2.500000000000000000, 4.430127018922196847 ) ) ;
#85624 = CARTESIAN_POINT ( 'NONE',  ( 6.249999999999930722, 12.50000000000000000, 1.472243186433545459 ) ) ;
#85625 = EDGE_CURVE ( 'NONE', #11699, #32199, #50075, .T. ) ;
#85626 = CARTESIAN_POINT ( 'NONE',  ( 12.69999999999990159, 2.500000000000000000, 4.776537180435972196 ) ) ;
#85627 = DIRECTION ( 'NONE',  ( 0.000000000000000000, 0.000000000000000000, 1.000000000000000000 ) ) ;
#85628 = VECTOR ( 'NONE', #118661, 1000.000000000000000 ) ;
#85629 = EDGE_CURVE ( 'NONE', #8254, #30750, #27074, .T. ) ;
#85630 = CARTESIAN_POINT ( 'NONE',  ( 185.2135416670080588, 4.367472073101518859, -7.564683531249999149 ) ) ;
#85631 = LINE ( 'NONE', #106554, #92646 ) ;
#85632 = EDGE_CURVE ( 'NONE', #28676, #121748, #125270, .T. ) ;
#85633 = DIRECTION ( 'NONE',  ( 0.000000000000000000, 1.000000000000000000, 0.000000000000000000 ) ) ;
#85634 = ADVANCED_FACE ( 'NONE', ( #82998 ), #62710, .T. ) ;
#85635 = VECTOR ( 'NONE', #119830, 1000.000000000000000 ) ;
#85636 = VECTOR ( 'NONE', #104571, 1000.000000000000000 ) ;
#85637 = CARTESIAN_POINT ( 'NONE',  ( 2.099999999999948574, 12.50000000000000000, 3.637306695894644726 ) ) ;
#85638 = ADVANCED_FACE ( 'NONE', ( #43725 ), #104341, .T. ) ;
#85639 = EDGE_LOOP ( 'NONE', ( #110105, #28039, #122308, #7740 ) ) ;
#85640 = EDGE_LOOP ( 'NONE', ( #106560, #122092, #82892, #115272 ) ) ;
#85641 = ORIENTED_EDGE ( 'NONE', *, *, #98895, .F. ) ;
#85642 = EDGE_LOOP ( 'NONE', ( #13645, #20180, #12115, #11789 ) ) ;
#85643 = DIRECTION ( 'NONE',  ( 0.000000000000000000, 1.000000000000000000, 0.000000000000000000 ) ) ;
#85644 = FACE_BOUND ( 'NONE', #81039, .T. ) ;
#85645 = DIRECTION ( 'NONE',  ( 0.000000000000000000, 0.000000000000000000, 1.000000000000000000 ) ) ;
#85646 = AXIS2_PLACEMENT_3D ( 'NONE', #34084, #32163, #71404 ) ;
#85649 = EDGE_CURVE ( 'NONE', #33086, #109058, #129504, .T. ) ;
#85648 = CIRCLE ( 'NONE', #43901, 0.06509327318403745899 ) ;
#85647 = VECTOR ( 'NONE', #25843, 1000.000000000000000 ) ;
#85650 = ADVANCED_FACE ( 'NONE', ( #54172 ), #35187, .F. ) ;
#85651 = ORIENTED_EDGE ( 'NONE', *, *, #99515, .T. ) ;
#85652 = CARTESIAN_POINT ( 'NONE',  ( 3.149999999999946176, 2.500000000000000000, -2.411473670974877859 ) ) ;
#85653 = CARTESIAN_POINT ( 'NONE',  ( -0.6500000000000398792, 2.500000000000000000, -6.941600689897078347 ) ) ;
#85654 = VERTEX_POINT ( 'NONE', #73794 ) ;
#85655 = DIRECTION ( 'NONE',  ( 0.000000000000000000, 1.000000000000000000, 0.000000000000000000 ) ) ;
#85656 = CARTESIAN_POINT ( 'NONE',  ( 9.799999999999913669, 12.50000000000000000, 4.741630453620009789 ) ) ;
#85657 = AXIS2_PLACEMENT_3D ( 'NONE', #77389, #45365, #27005 ) ;
#85658 = AXIS2_PLACEMENT_3D ( 'NONE', #91740, #11231, #81283 ) ;
#85659 = EDGE_LOOP ( 'NONE', ( #115244, #77342, #13064, #65066 ) ) ;
#85660 = CARTESIAN_POINT ( 'NONE',  ( 6.699999999999930012, 2.500000000000000000, 4.230127018922196669 ) ) ;
#85661 = DIRECTION ( 'NONE',  ( 0.000000000000000000, 0.000000000000000000, 1.000000000000000000 ) ) ;
#85662 = AXIS2_PLACEMENT_3D ( 'NONE', #12515, #42657, #104133 ) ;
#85663 = ORIENTED_EDGE ( 'NONE', *, *, #20081, .F. ) ;
#85664 = PLANE ( 'NONE',  #103247 ) ;
#85665 = CARTESIAN_POINT ( 'NONE',  ( 13.74999999999993427, 2.500000000000000000, 2.165063509461097713 ) ) ;
#85666 = EDGE_LOOP ( 'NONE', ( #85595, #84771, #14128, #36757 ) ) ;
#85667 = FACE_OUTER_BOUND ( 'NONE', #113765, .T. ) ;
#85668 = CIRCLE ( 'NONE', #119126, 0.1000000000000000472 ) ;
#85669 = ORIENTED_EDGE ( 'NONE', *, *, #124056, .F. ) ;
#85670 = ORIENTED_EDGE ( 'NONE', *, *, #80465, .T. ) ;
#85671 = CARTESIAN_POINT ( 'NONE',  ( 10.84999999999990905, 12.50000000000000000, 1.472243186433545459 ) ) ;
#85672 = VERTEX_POINT ( 'NONE', #102611 ) ;
#85673 = DIRECTION ( 'NONE',  ( 0.000000000000000000, 0.000000000000000000, 1.000000000000000000 ) ) ;
#85674 = CARTESIAN_POINT ( 'NONE',  ( -10.65000000000000213, 2.500000000000000000, 6.741600689897071952 ) ) ;
#85675 = VERTEX_POINT ( 'NONE', #74452 ) ;
#85676 = DIRECTION ( 'NONE',  ( -0.000000000000000000, 1.000000000000000000, -0.000000000000000000 ) ) ;
#85677 = DIRECTION ( 'NONE',  ( -0.000000000000000000, 1.000000000000000000, -0.000000000000000000 ) ) ;
#85678 = CARTESIAN_POINT ( 'NONE',  ( -1.050000000000037792, 12.50000000000000000, 1.818653347947321475 ) ) ;
#85679 = CARTESIAN_POINT ( 'NONE',  ( 1.249999999999952038, 12.50000000000000000, 5.737276932171707422 ) ) ;
#85680 = CARTESIAN_POINT ( 'NONE',  ( -11.24999999999996270, 2.500000000000000000, 6.595190528383296780 ) ) ;
#85681 = CARTESIAN_POINT ( 'NONE',  ( 17.50011966276722220, 2.224296756944650344, -4.070989939659154011 ) ) ;
#85682 = ORIENTED_EDGE ( 'NONE', *, *, #87652, .T. ) ;
#85683 = ADVANCED_FACE ( 'NONE', ( #52881 ), #55454, .T. ) ;
#85684 = VERTEX_POINT ( 'NONE', #53532 ) ;
#85685 = DIRECTION ( 'NONE',  ( 0.000000000000000000, 0.000000000000000000, 1.000000000000000000 ) ) ;
#85686 = CARTESIAN_POINT ( 'NONE',  ( 16.55874544816229132, -0.4845305829427751232, 6.091953208798936537 ) ) ;
#85687 = CARTESIAN_POINT ( 'NONE',  ( 13.14999999999989733, 2.500000000000000000, -1.818653347947325916 ) ) ;
#85689 = ORIENTED_EDGE ( 'NONE', *, *, #68880, .F. ) ;
#85688 = ORIENTED_EDGE ( 'NONE', *, *, #63493, .T. ) ;
#85690 = ORIENTED_EDGE ( 'NONE', *, *, #66007, .F. ) ;
#85691 = AXIS2_PLACEMENT_3D ( 'NONE', #69927, #7769, #58189 ) ;
#85692 = DIRECTION ( 'NONE',  ( 0.000000000000000000, 0.000000000000000000, 1.000000000000000000 ) ) ;
#85693 = CARTESIAN_POINT ( 'NONE',  ( -8.100000000000013856, 2.500000000000000000, 0.2464101615137736789 ) ) ;
#85694 = DIRECTION ( 'NONE',  ( 1.000000000000000000, 0.000000000000000000, 0.000000000000000000 ) ) ;
#85695 = SURFACE_SIDE_STYLE ('',( #43866 ) ) ;
#85697 = CIRCLE ( 'NONE', #20864, 0.1000000000000002554 ) ;
#85696 = CIRCLE ( 'NONE', #102434, 0.06509327318403745899 ) ;
#85698 = DIRECTION ( 'NONE',  ( -0.000000000000000000, -1.000000000000000000, -0.000000000000000000 ) ) ;
#85699 = CARTESIAN_POINT ( 'NONE',  ( 7.049999999999928768, 12.50000000000000000, 6.560283801567334372 ) ) ;
#85700 = DIRECTION ( 'NONE',  ( -0.000000000000000000, 1.000000000000000000, -0.000000000000000000 ) ) ;
#85701 = DIRECTION ( 'NONE',  ( 0.000000000000000000, 1.000000000000000000, 0.000000000000000000 ) ) ;
#85702 = DIRECTION ( 'NONE',  ( 0.000000000000000000, 1.000000000000000000, 0.000000000000000000 ) ) ;
#85703 = PLANE ( 'NONE',  #28956 ) ;
#85705 = AXIS2_PLACEMENT_3D ( 'NONE', #77882, #126356, #128301 ) ;
#85704 = VECTOR ( 'NONE', #82030, 1000.000000000000000 ) ;
#85706 = ORIENTED_EDGE ( 'NONE', *, *, #61415, .T. ) ;
#85707 = DIRECTION ( 'NONE',  ( 0.000000000000000000, 1.000000000000000000, 0.000000000000000000 ) ) ;
#85708 = ORIENTED_EDGE ( 'NONE', *, *, #64896, .T. ) ;
#85709 = ORIENTED_EDGE ( 'NONE', *, *, #101403, .T. ) ;
#85710 = PLANE ( 'NONE',  #60927 ) ;
#85711 = DIRECTION ( 'NONE',  ( 0.000000000000000000, -0.000000000000000000, 1.000000000000000000 ) ) ;
#85712 = DIRECTION ( 'NONE',  ( 0.000000000000000000, 0.000000000000000000, -1.000000000000000000 ) ) ;
#85713 = CARTESIAN_POINT ( 'NONE',  ( 4.599999999999938360, 2.500000000000000000, 0.09999999999999772959 ) ) ;
#85714 = DIRECTION ( 'NONE',  ( 0.000000000000000000, 1.000000000000000000, 0.000000000000000000 ) ) ;
#85715 = CARTESIAN_POINT ( 'NONE',  ( 1.049999999999953637, 2.500000000000000000, 2.511473670974873507 ) ) ;
#85716 = LINE ( 'NONE', #67338, #99158 ) ;
#85717 = ORIENTED_EDGE ( 'NONE', *, *, #116327, .T. ) ;
#85718 = PLANE ( 'NONE',  #59860 ) ;
#85719 = CARTESIAN_POINT ( 'NONE',  ( 5.849999999999933920, 2.500000000000000000, -2.165063509461101710 ) ) ;
#85720 = ORIENTED_EDGE ( 'NONE', *, *, #28157, .T. ) ;
#85721 = CONICAL_SURFACE ( 'NONE', #102461, 0.09999999999999982514, 0.003490658503988666988 ) ;
#85722 = EDGE_CURVE ( 'NONE', #29766, #113276, #8181, .T. ) ;
#85724 = VERTEX_POINT ( 'NONE', #103275 ) ;
#85723 = CIRCLE ( 'NONE', #125442, 0.09999999999999999167 ) ;
#85725 = VERTEX_POINT ( 'NONE', #13580 ) ;
#85726 = ADVANCED_FACE ( 'NONE', ( #113741 ), #24066, .T. ) ;
#85727 = ORIENTED_EDGE ( 'NONE', *, *, #50090, .T. ) ;
#85728 = EDGE_CURVE ( 'NONE', #105930, #14509, #123223, .T. ) ;
#85729 = DIRECTION ( 'NONE',  ( -4.274815082592931898E-19, -0.9999939076577903929, -0.003490651415223739937 ) ) ;
#85730 = DIRECTION ( 'NONE',  ( 0.000000000000000000, 1.000000000000000000, 0.000000000000000000 ) ) ;
#85731 = AXIS2_PLACEMENT_3D ( 'NONE', #72581, #81113, #11712 ) ;
#85732 = CARTESIAN_POINT ( 'NONE',  ( 1.049999999999952971, 2.500000000000000000, 6.148780366869520897 ) ) ;
#85733 = FACE_OUTER_BOUND ( 'NONE', #96339, .T. ) ;
#85734 = ADVANCED_FACE ( 'NONE', ( #18744 ), #112759, .T. ) ;
#85735 = FACE_OUTER_BOUND ( 'NONE', #92286, .T. ) ;
#85737 = EDGE_LOOP ( 'NONE', ( #99076, #75301, #91960, #97803 ) ) ;
#85736 = EDGE_CURVE ( 'NONE', #33390, #102762, #46270, .T. ) ;
#85738 = ADVANCED_FACE ( 'NONE', ( #96021 ), #56298, .T. ) ;
#85739 = DIRECTION ( 'NONE',  ( 0.000000000000000000, -0.000000000000000000, 1.000000000000000000 ) ) ;
#85740 = CONICAL_SURFACE ( 'NONE', #81552, 0.09999999999999999167, 0.003490658503988666988 ) ;
#85741 = CARTESIAN_POINT ( 'NONE',  ( 13.09999999999990195, 2.500000000000000000, 4.776537180435972196 ) ) ;
#85742 = AXIS2_PLACEMENT_3D ( 'NONE', #123730, #81876, #53084 ) ;
#85743 = ORIENTED_EDGE ( 'NONE', *, *, #50674, .T. ) ;
#85744 = CONICAL_SURFACE ( 'NONE', #62786, 0.1000000000000000472, 0.003490658503988666988 ) ;
#85745 = ORIENTED_EDGE ( 'NONE', *, *, #91458, .T. ) ;
#85746 = ORIENTED_EDGE ( 'NONE', *, *, #1535, .F. ) ;
#85747 = DIRECTION ( 'NONE',  ( -0.000000000000000000, 1.000000000000000000, -0.000000000000000000 ) ) ;
#85748 = CIRCLE ( 'NONE', #117129, 0.06509327318403745899 ) ;
#85749 = CARTESIAN_POINT ( 'NONE',  ( -11.89999999999999680, 2.500000000000000000, -3.883716857408423984 ) ) ;
#85750 = CARTESIAN_POINT ( 'NONE',  ( -3.150000000000029221, 12.50000000000000000, -1.818653347947326138 ) ) ;
#85751 = AXIS2_PLACEMENT_3D ( 'NONE', #78579, #67412, #17689 ) ;
#85752 = VERTEX_POINT ( 'NONE', #47577 ) ;
#85753 = DIRECTION ( 'NONE',  ( 0.000000000000000000, 0.000000000000000000, 1.000000000000000000 ) ) ;
#85754 = PLANE ( 'NONE',  #80955 ) ;
#85755 = CARTESIAN_POINT ( 'NONE',  ( 13.29999999999989946, 2.500000000000000000, 0.09999999999999761857 ) ) ;
#85756 = FACE_OUTER_BOUND ( 'NONE', #31902, .T. ) ;
#85757 = FACE_OUTER_BOUND ( 'NONE', #83341, .T. ) ;
#85758 = ORIENTED_EDGE ( 'NONE', *, *, #45918, .F. ) ;
#85759 = DIRECTION ( 'NONE',  ( -1.000000000000000000, -0.000000000000000000, -0.000000000000000000 ) ) ;
#85760 = EDGE_LOOP ( 'NONE', ( #87763, #52777 ) ) ;
#85761 = EDGE_LOOP ( 'NONE', ( #44038, #99185, #61968, #93761 ) ) ;
#85762 = VERTEX_POINT ( 'NONE', #27924 ) ;
#85763 = CARTESIAN_POINT ( 'NONE',  ( -2.500000000000032419, 2.500000000000000000, -3.637306695894650055 ) ) ;
#85764 = FACE_BOUND ( 'NONE', #52390, .T. ) ;
#85765 = FACE_OUTER_BOUND ( 'NONE', #29166, .T. ) ;
#85766 = DIRECTION ( 'NONE',  ( -4.274815082592931898E-19, -0.9999939076577903929, -0.003490651415223739937 ) ) ;
#85767 = CARTESIAN_POINT ( 'NONE',  ( 4.599999999999940137, 12.50000000000000000, -5.022947341949754119 ) ) ;
#85769 = EDGE_CURVE ( 'NONE', #39292, #78915, #14528, .T. ) ;
#85768 = VECTOR ( 'NONE', #23237, 1000.000000000000000 ) ;
#85770 = ORIENTED_EDGE ( 'NONE', *, *, #16692, .T. ) ;
#85771 = EDGE_CURVE ( 'NONE', #33523, #3854, #35814, .T. ) ;
#85773 = AXIS2_PLACEMENT_3D ( 'NONE', #74441, #64608, #104537 ) ;
#85772 = FACE_OUTER_BOUND ( 'NONE', #64070, .T. ) ;
#85774 = CARTESIAN_POINT ( 'NONE',  ( -3.350000000000028511, 2.500000000000000000, -2.957883832488653830 ) ) ;
#85775 = CARTESIAN_POINT ( 'NONE',  ( -6.650000000000018119, 12.50000000000000000, -6.560283801567339701 ) ) ;
#85776 = EDGE_CURVE ( 'NONE', #4707, #3076, #116289, .T. ) ;
#85777 = DIRECTION ( 'NONE',  ( 0.000000000000000000, 0.000000000000000000, 1.000000000000000000 ) ) ;
#85778 = EDGE_LOOP ( 'NONE', ( #35646, #57685, #3736, #92459 ) ) ;
#85779 = CARTESIAN_POINT ( 'NONE',  ( 3.099999999999943245, 2.500000000000000000, 3.983716857408420076 ) ) ;
#85781 = VECTOR ( 'NONE', #60553, 1000.000000000000000 ) ;
#85780 = AXIS2_PLACEMENT_3D ( 'NONE', #52593, #24426, #74175 ) ;
#85782 = CARTESIAN_POINT ( 'NONE',  ( 3.549999999999942091, 12.50000000000000000, 2.511473670974873507 ) ) ;
#85783 = ADVANCED_FACE ( 'NONE', ( #65908 ), #77239, .T. ) ;
#85784 = ORIENTED_EDGE ( 'NONE', *, *, #105746, .F. ) ;
#85785 = DIRECTION ( 'NONE',  ( 0.000000000000000000, 1.000000000000000000, 0.000000000000000000 ) ) ;
#85786 = EDGE_CURVE ( 'NONE', #67840, #58977, #16580, .T. ) ;
#85787 = FACE_BOUND ( 'NONE', #103299, .T. ) ;
#85788 = DIRECTION ( 'NONE',  ( -0.000000000000000000, -1.000000000000000000, -0.000000000000000000 ) ) ;
#85789 = ADVANCED_FACE ( 'NONE', ( #67846 ), #115646, .T. ) ;
#85790 = EDGE_CURVE ( 'NONE', #84307, #16039, #18650, .T. ) ;
#85791 = ADVANCED_FACE ( 'NONE', ( #68487 ), #87602, .T. ) ;
#85792 = ORIENTED_EDGE ( 'NONE', *, *, #105572, .F. ) ;
#85793 = FACE_OUTER_BOUND ( 'NONE', #82942, .T. ) ;
#85794 = DIRECTION ( 'NONE',  ( -0.000000000000000000, -1.000000000000000000, -0.000000000000000000 ) ) ;
#85795 = ORIENTED_EDGE ( 'NONE', *, *, #122133, .T. ) ;
#85796 = ORIENTED_EDGE ( 'NONE', *, *, #12480, .F. ) ;
#85797 = CARTESIAN_POINT ( 'NONE',  ( 186.7135416670080872, 4.367472073101518859, -7.564683531249999149 ) ) ;
#85798 = EDGE_CURVE ( 'NONE', #27457, #99444, #77659, .T. ) ;
#85799 = ORIENTED_EDGE ( 'NONE', *, *, #110620, .T. ) ;
#85800 = CARTESIAN_POINT ( 'NONE',  ( 184.8802083336747444, 4.367472073101515306, 7.564683531250000925 ) ) ;
#85801 = DIRECTION ( 'NONE',  ( 0.000000000000000000, 0.000000000000000000, -1.000000000000000000 ) ) ;
#85802 = DIRECTION ( 'NONE',  ( -0.000000000000000000, 1.000000000000000000, -0.000000000000000000 ) ) ;
#85803 = CARTESIAN_POINT ( 'NONE',  ( 4.149999999999936406, 12.50000000000000000, 6.495190528383297135 ) ) ;
#85804 = DIRECTION ( 'NONE',  ( 0.000000000000000000, 0.000000000000000000, -1.000000000000000000 ) ) ;
#85805 = VECTOR ( 'NONE', #101519, 1000.000000000000000 ) ;
#85806 = CONICAL_SURFACE ( 'NONE', #46115, 0.09999999999999982514, 0.003490658503988666988 ) ;
#85807 = ORIENTED_EDGE ( 'NONE', *, *, #108774, .F. ) ;
#85808 = EDGE_LOOP ( 'NONE', ( #50058, #104917 ) ) ;
#85809 = LINE ( 'NONE', #17037, #15155 ) ;
#85810 = DIRECTION ( 'NONE',  ( 0.000000000000000000, 0.000000000000000000, -1.000000000000000000 ) ) ;
#85811 = CARTESIAN_POINT ( 'NONE',  ( 5.449999999999937117, 2.500000000000000000, -6.395190528383301931 ) ) ;
#85812 = DIRECTION ( 'NONE',  ( 0.000000000000000000, 0.000000000000000000, -1.000000000000000000 ) ) ;
#85814 = VERTEX_POINT ( 'NONE', #117560 ) ;
#85813 = ORIENTED_EDGE ( 'NONE', *, *, #114609, .F. ) ;
#85815 = CARTESIAN_POINT ( 'NONE',  ( -11.25000000000000000, 2.500000000000000000, -2.757883832488650100 ) ) ;
#85816 = VERTEX_POINT ( 'NONE', #8911 ) ;
#85817 = DIRECTION ( 'NONE',  ( 0.000000000000000000, 1.000000000000000000, 0.000000000000000000 ) ) ;
#85818 = DIRECTION ( 'NONE',  ( 0.000000000000000000, 0.000000000000000000, 1.000000000000000000 ) ) ;
#85819 = AXIS2_PLACEMENT_3D ( 'NONE', #54065, #72426, #112346 ) ;
#85820 = EDGE_LOOP ( 'NONE', ( #70274, #27026 ) ) ;
#85821 = DIRECTION ( 'NONE',  ( 0.000000000000000000, -0.000000000000000000, 1.000000000000000000 ) ) ;
#85822 = CARTESIAN_POINT ( 'NONE',  ( -4.150000000000025224, 2.500000000000000000, 5.802370205355744659 ) ) ;
#85823 = CARTESIAN_POINT ( 'NONE',  ( 4.999999999999933387, 12.50000000000000000, 5.088040615133786027 ) ) ;
#85824 = CARTESIAN_POINT ( 'NONE',  ( -3.350000000000028511, 12.50000000000000000, 2.857883832488649301 ) ) ;
#85825 = CARTESIAN_POINT ( 'NONE',  ( -6.250000000000015987, 2.500000000000000000, 1.372243186433545370 ) ) ;
#85826 = DIRECTION ( 'NONE',  ( -1.000000000000000000, -0.000000000000000000, -0.000000000000000000 ) ) ;
#85827 = CARTESIAN_POINT ( 'NONE',  ( 186.4843750003414016, -8.734944146203032389, -1.604583208406767949E-15 ) ) ;
#85828 = CARTESIAN_POINT ( 'NONE',  ( -5.200000000000020606, 2.500000000000000000, -0.4464101615137782142 ) ) ;
#85829 = DIRECTION ( 'NONE',  ( -4.274815082592931898E-19, -0.9999939076577903929, -0.003490651415223739937 ) ) ;
#85830 = AXIS2_PLACEMENT_3D ( 'NONE', #7833, #127619, #18937 ) ;
#85831 = EDGE_LOOP ( 'NONE', ( #63689, #59998, #60527, #75479 ) ) ;
#85832 = AXIS2_PLACEMENT_3D ( 'NONE', #80966, #120878, #31230 ) ;
#85833 = ADVANCED_FACE ( 'NONE', ( #86172 ), #118238, .T. ) ;
#85834 = VERTEX_POINT ( 'NONE', #7626 ) ;
#85835 = CARTESIAN_POINT ( 'NONE',  ( -13.14999999999999147, 2.500000000000000000, 1.918653347947325338 ) ) ;
#85836 = EDGE_LOOP ( 'NONE', ( #22101, #61458 ) ) ;
#85837 = DIRECTION ( 'NONE',  ( 0.000000000000000000, -0.000000000000000000, 1.000000000000000000 ) ) ;
#85839 = EDGE_LOOP ( 'NONE', ( #120679, #27893, #17148, #60564 ) ) ;
#85838 = EDGE_LOOP ( 'NONE', ( #67310, #16194, #125926, #103772 ) ) ;
#85840 = VERTEX_POINT ( 'NONE', #48873 ) ;
#85841 = CARTESIAN_POINT ( 'NONE',  ( 13.09999999999990195, 2.500000000000000000, -3.983716857408426293 ) ) ;
#85842 = VECTOR ( 'NONE', #29297, 1000.000000000000000 ) ;
#85843 = CARTESIAN_POINT ( 'NONE',  ( -13.34999999999999076, 12.50000000000000000, 2.165063509461101265 ) ) ;
#85844 = DIRECTION ( 'NONE',  ( -0.000000000000000000, -1.000000000000000000, -0.000000000000000000 ) ) ;
#85845 = AXIS2_PLACEMENT_3D ( 'NONE', #100140, #10456, #79839 ) ;
#85846 = CARTESIAN_POINT ( 'NONE',  ( 12.09999999999990195, 2.500000000000000000, -0.7928203230275542301 ) ) ;
#85847 = CARTESIAN_POINT ( 'NONE',  ( 5.849999999999931255, 12.50000000000000000, 2.857883832488649301 ) ) ;
#85848 = EDGE_CURVE ( 'NONE', #100949, #75943, #119005, .T. ) ;
#85849 = EDGE_LOOP ( 'NONE', ( #1608, #13269 ) ) ;
#85850 = LINE ( 'NONE', #95696, #26794 ) ;
#85851 = ORIENTED_EDGE ( 'NONE', *, *, #111840, .F. ) ;
#85852 = ORIENTED_EDGE ( 'NONE', *, *, #50333, .T. ) ;
#85853 = ORIENTED_EDGE ( 'NONE', *, *, #83461, .F. ) ;
#85854 = ORIENTED_EDGE ( 'NONE', *, *, #122559, .F. ) ;
#85855 = DIRECTION ( 'NONE',  ( 0.000000000000000000, 0.000000000000000000, 1.000000000000000000 ) ) ;
#85856 = VERTEX_POINT ( 'NONE', #16144 ) ;
#85857 = VERTEX_POINT ( 'NONE', #56085 ) ;
#85858 = CARTESIAN_POINT ( 'NONE',  ( 0.4499999999999552136, 2.500000000000000000, 6.495190528383297135 ) ) ;
#85859 = DIRECTION ( 'NONE',  ( 0.000000000000000000, 0.000000000000000000, -1.000000000000000000 ) ) ;
#85860 = DIRECTION ( 'NONE',  ( 0.000000000000000000, 0.000000000000000000, 1.000000000000000000 ) ) ;
#85861 = DIRECTION ( 'NONE',  ( -0.000000000000000000, -1.000000000000000000, -0.000000000000000000 ) ) ;
#85862 = DIRECTION ( 'NONE',  ( -4.274815082592931898E-19, -0.9999939076577903929, -0.003490651415223739937 ) ) ;
#85863 = ORIENTED_EDGE ( 'NONE', *, *, #11586, .F. ) ;
#85864 = AXIS2_PLACEMENT_3D ( 'NONE', #68980, #87953, #127907 ) ;
#85865 = CARTESIAN_POINT ( 'NONE',  ( -4.800000000000024691, 12.50000000000000000, 0.3464101615137735735 ) ) ;
#85866 = ORIENTED_EDGE ( 'NONE', *, *, #116127, .T. ) ;
#85867 = PLANE ( 'NONE',  #44328 ) ;
#85868 = EDGE_CURVE ( 'NONE', #110466, #38646, #6321, .T. ) ;
#85869 = STYLED_ITEM ( 'NONE', ( #8628 ), #102059 ) ;
#85870 = VERTEX_POINT ( 'NONE', #46941 ) ;
#85871 = DIRECTION ( 'NONE',  ( 0.000000000000000000, 1.000000000000000000, 0.000000000000000000 ) ) ;
#85872 = EDGE_LOOP ( 'NONE', ( #83398, #81383 ) ) ;
#85873 = AXIS2_PLACEMENT_3D ( 'NONE', #39688, #37730, #88080 ) ;
#85874 = ORIENTED_EDGE ( 'NONE', *, *, #124485, .T. ) ;
#85875 = ADVANCED_FACE ( 'NONE', ( #31803 ), #35389, .T. ) ;
#85876 = CARTESIAN_POINT ( 'NONE',  ( -8.300000000000011369, 12.50000000000000000, -4.330127018922201643 ) ) ;
#85877 = DIRECTION ( 'NONE',  ( 0.000000000000000000, -0.000000000000000000, 1.000000000000000000 ) ) ;
#85878 = CARTESIAN_POINT ( 'NONE',  ( -11.05000000000000249, 2.500000000000000000, -6.148780366869522673 ) ) ;
#85879 = CARTESIAN_POINT ( 'NONE',  ( -10.20000000000000639, 12.50000000000000000, -3.918623584224384615 ) ) ;
#85880 = EDGE_CURVE ( 'NONE', #82140, #122576, #6124, .T. ) ;
#85881 = CARTESIAN_POINT ( 'NONE',  ( 11.24999999999990941, 2.500000000000000000, 7.088010851410848190 ) ) ;
#85883 = EDGE_LOOP ( 'NONE', ( #119392, #55546 ) ) ;
#85882 = ADVANCED_FACE ( 'NONE', ( #41642 ), #96023, .T. ) ;
#85884 = DIRECTION ( 'NONE',  ( -0.000000000000000000, 1.000000000000000000, -0.000000000000000000 ) ) ;
#85885 = CARTESIAN_POINT ( 'NONE',  ( 12.89999999999990266, 2.500000000000000000, 4.922947341949748257 ) ) ;
#85886 = EDGE_CURVE ( 'NONE', #26403, #13366, #39617, .T. ) ;
#85887 = DIRECTION ( 'NONE',  ( -0.000000000000000000, -1.000000000000000000, -0.000000000000000000 ) ) ;
#85888 = EDGE_CURVE ( 'NONE', #106311, #113123, #81540, .T. ) ;
#85889 = EDGE_CURVE ( 'NONE', #67958, #47787, #129306, .T. ) ;
#85890 = FACE_OUTER_BOUND ( 'NONE', #75607, .T. ) ;
#85891 = FACE_OUTER_BOUND ( 'NONE', #35552, .T. ) ;
#85892 = ORIENTED_EDGE ( 'NONE', *, *, #44284, .T. ) ;
#85893 = VECTOR ( 'NONE', #7757, 1000.000000000000000 ) ;
#85894 = ORIENTED_EDGE ( 'NONE', *, *, #128504, .T. ) ;
#85895 = CARTESIAN_POINT ( 'NONE',  ( -11.89999999999999503, 12.50000000000000000, 4.676537180435972552 ) ) ;
#85896 = EDGE_CURVE ( 'NONE', #91980, #93976, #33149, .T. ) ;
#85897 = VERTEX_POINT ( 'NONE', #90713 ) ;
#85898 = DIRECTION ( 'NONE',  ( -0.000000000000000000, -1.000000000000000000, -0.000000000000000000 ) ) ;
#85899 = VECTOR ( 'NONE', #10397, 1000.000000000000000 ) ;
#85900 = CARTESIAN_POINT ( 'NONE',  ( 1.449999999999951328, 2.500000000000000000, -1.718653347947326049 ) ) ;
#85901 = EDGE_CURVE ( 'NONE', #90888, #22290, #68920, .T. ) ;
#85902 = ORIENTED_EDGE ( 'NONE', *, *, #2262, .F. ) ;
#85903 = CARTESIAN_POINT ( 'NONE',  ( 185.4166666666666856, 6.668395609140176816, 3.850000000000000977 ) ) ;
#85904 = CARTESIAN_POINT ( 'NONE',  ( 1.449999999999952216, 2.500000000000000000, -2.611473670974877592 ) ) ;
#85905 = DIRECTION ( 'NONE',  ( 0.000000000000000000, -0.000000000000000000, 1.000000000000000000 ) ) ;
#85906 = CARTESIAN_POINT ( 'NONE',  ( -8.550000000000009592, 2.500000000000000000, 6.841600689897072485 ) ) ;
#85907 = EDGE_LOOP ( 'NONE', ( #36408, #5368, #60892, #24223 ) ) ;
#85908 = AXIS2_PLACEMENT_3D ( 'NONE', #16354, #56296, #36686 ) ;
#85909 = AXIS2_PLACEMENT_3D ( 'NONE', #91679, #81222, #43245 ) ;
#85910 = DIRECTION ( 'NONE',  ( 0.000000000000000000, 0.000000000000000000, 1.000000000000000000 ) ) ;
#85911 = FACE_OUTER_BOUND ( 'NONE', #11461, .T. ) ;
#85912 = ORIENTED_EDGE ( 'NONE', *, *, #48385, .T. ) ;
#85913 = LINE ( 'NONE', #40723, #56886 ) ;
#85914 = FACE_OUTER_BOUND ( 'NONE', #112780, .T. ) ;
#85915 = DIRECTION ( 'NONE',  ( 0.000000000000000000, 1.000000000000000000, 0.000000000000000000 ) ) ;
#85916 = AXIS2_PLACEMENT_3D ( 'NONE', #120386, #50350, #128282 ) ;
#85917 = ORIENTED_EDGE ( 'NONE', *, *, #110731, .T. ) ;
#85918 = PRODUCT_DEFINITION_SHAPE ( 'NONE', 'NONE',  #129618 ) ;
#85919 = DIRECTION ( 'NONE',  ( 0.000000000000000000, 1.000000000000000000, 0.000000000000000000 ) ) ;
#85920 = EDGE_LOOP ( 'NONE', ( #33685, #128640 ) ) ;
#85921 = DIRECTION ( 'NONE',  ( 0.000000000000000000, 0.000000000000000000, 1.000000000000000000 ) ) ;
#85922 = DIRECTION ( 'NONE',  ( -0.000000000000000000, 1.000000000000000000, -0.000000000000000000 ) ) ;
#85923 = CIRCLE ( 'NONE', #48386, 0.1000000000000002554 ) ;
#85924 = CARTESIAN_POINT ( 'NONE',  ( -14.59999999999998366, 2.500000000000000000, 0.09999999999999989453 ) ) ;
#85925 = EDGE_CURVE ( 'NONE', #24108, #60798, #16667, .T. ) ;
#85926 = VERTEX_POINT ( 'NONE', #377 ) ;
#85927 = FACE_OUTER_BOUND ( 'NONE', #84590, .T. ) ;
#85928 = ADVANCED_FACE ( 'NONE', ( #78976 ), #89847, .T. ) ;
#85929 = CARTESIAN_POINT ( 'NONE',  ( -0.4000000000000331624, 2.500000000000000000, 0.000000000000000000 ) ) ;
#85930 = AXIS2_PLACEMENT_3D ( 'NONE', #34547, #84254, #4383 ) ;
#85931 = ORIENTED_EDGE ( 'NONE', *, *, #69863, .F. ) ;
#85932 = EDGE_CURVE ( 'NONE', #120284, #99983, #81451, .T. ) ;
#85933 = EDGE_LOOP ( 'NONE', ( #59974, #30279 ) ) ;
#85934 = CARTESIAN_POINT ( 'NONE',  ( 1.649999999999949729, 2.500000000000000000, 7.288010851410849256 ) ) ;
#85935 = ADVANCED_FACE ( 'NONE', ( #1041 ), #12484, .T. ) ;
#85936 = EDGE_CURVE ( 'NONE', #45123, #5118, #109040, .T. ) ;
#85937 = ORIENTED_EDGE ( 'NONE', *, *, #85936, .T. ) ;
#85938 = DIRECTION ( 'NONE',  ( -0.000000000000000000, -1.000000000000000000, -0.000000000000000000 ) ) ;
#85939 = CARTESIAN_POINT ( 'NONE',  ( -15.59999999999998010, 2.500000000000000000, 0.3464101615137759604 ) ) ;
#85940 = VERTEX_POINT ( 'NONE', #61262 ) ;
#85941 = DIRECTION ( 'NONE',  ( -0.000000000000000000, -1.000000000000000000, -0.000000000000000000 ) ) ;
#85942 = DIRECTION ( 'NONE',  ( 0.000000000000000000, 0.000000000000000000, -1.000000000000000000 ) ) ;
#85943 = EDGE_LOOP ( 'NONE', ( #62536, #1817 ) ) ;
#85944 = ADVANCED_FACE ( 'NONE', ( #39064 ), #39713, .T. ) ;
#85945 = DIRECTION ( 'NONE',  ( -0.000000000000000000, 1.000000000000000000, -0.000000000000000000 ) ) ;
#85946 = DIRECTION ( 'NONE',  ( 0.000000000000000000, 0.000000000000000000, 1.000000000000000000 ) ) ;
#85947 = CIRCLE ( 'NONE', #125659, 0.06509327318403745899 ) ;
#85948 = DIRECTION ( 'NONE',  ( 0.000000000000000000, -0.000000000000000000, 1.000000000000000000 ) ) ;
#85949 = DIRECTION ( 'NONE',  ( -0.000000000000000000, -1.000000000000000000, -0.000000000000000000 ) ) ;
#85950 = AXIS2_PLACEMENT_3D ( 'NONE', #19206, #27116, #97144 ) ;
#85951 = FACE_OUTER_BOUND ( 'NONE', #16792, .T. ) ;
#85952 = CARTESIAN_POINT ( 'NONE',  ( -7.050000000000013145, 2.500000000000000000, 2.165063509461097713 ) ) ;
#85953 = AXIS2_PLACEMENT_3D ( 'NONE', #104124, #102198, #74655 ) ;
#85954 = ORIENTED_EDGE ( 'NONE', *, *, #120735, .F. ) ;
#85956 = EDGE_LOOP ( 'NONE', ( #89464, #90266 ) ) ;
#85955 = AXIS2_PLACEMENT_3D ( 'NONE', #125448, #126084, #35787 ) ;
#85957 = EDGE_LOOP ( 'NONE', ( #89196, #107237 ) ) ;
#85958 = EDGE_LOOP ( 'NONE', ( #65748, #107492, #59475, #40365 ) ) ;
#85959 = DIRECTION ( 'NONE',  ( 0.000000000000000000, 0.000000000000000000, 1.000000000000000000 ) ) ;
#85960 = CARTESIAN_POINT ( 'NONE',  ( -0.2000000000000339284, 12.50000000000000000, -0.4115034346978133639 ) ) ;
#85961 = CIRCLE ( 'NONE', #54660, 7.700000000000000178 ) ;
#85962 = CARTESIAN_POINT ( 'NONE',  ( -8.350000000000008527, 2.500000000000000000, 5.802370205355744659 ) ) ;
#85963 = VERTEX_POINT ( 'NONE', #80901 ) ;
#85964 = FACE_BOUND ( 'NONE', #91314, .T. ) ;
#85965 = ADVANCED_FACE ( 'NONE', ( #29861 ), #51452, .T. ) ;
#85966 = CARTESIAN_POINT ( 'NONE',  ( -5.850000000000022737, 2.500000000000000000, -6.395190528383301931 ) ) ;
#85967 = FACE_OUTER_BOUND ( 'NONE', #112999, .T. ) ;
#85968 = CARTESIAN_POINT ( 'NONE',  ( -2.050000000000032685, 12.50000000000000000, -2.165063509461101710 ) ) ;
#85969 = DIRECTION ( 'NONE',  ( -0.000000000000000000, -1.000000000000000000, -0.000000000000000000 ) ) ;
#85970 = CARTESIAN_POINT ( 'NONE',  ( 16.87640210516338968, -2.500000000000000000, 4.436424697255031191 ) ) ;
#85971 = CARTESIAN_POINT ( 'NONE',  ( -0.6000000000000383915, 2.500000000000000000, -4.576537180435977348 ) ) ;
#85972 = CARTESIAN_POINT ( 'NONE',  ( -4.550000000000022915, 2.500000000000000000, 6.495190528383297135 ) ) ;
#85973 = DIRECTION ( 'NONE',  ( 0.000000000000000000, 0.000000000000000000, 1.000000000000000000 ) ) ;
#85974 = DIRECTION ( 'NONE',  ( -4.274815082592931898E-19, -0.9999939076577903929, -0.003490651415223739937 ) ) ;
#85975 = CARTESIAN_POINT ( 'NONE',  ( 1.249999999999988454, 12.50000000000000000, -2.099970236277064473 ) ) ;
#85976 = ORIENTED_EDGE ( 'NONE', *, *, #98746, .F. ) ;
#85977 = ORIENTED_EDGE ( 'NONE', *, *, #41313, .F. ) ;
#85978 = EDGE_CURVE ( 'NONE', #82935, #28339, #39716, .T. ) ;
#85979 = VERTEX_POINT ( 'NONE', #99897 ) ;
#85980 = ORIENTED_EDGE ( 'NONE', *, *, #63725, .T. ) ;
#85981 = DIRECTION ( 'NONE',  ( -4.274815082592931898E-19, -0.9999939076577903929, -0.003490651415223739937 ) ) ;
#85982 = ORIENTED_EDGE ( 'NONE', *, *, #44210, .F. ) ;
#85983 = DIRECTION ( 'NONE',  ( 0.000000000000000000, -0.000000000000000000, 1.000000000000000000 ) ) ;
#85984 = ORIENTED_EDGE ( 'NONE', *, *, #5457, .T. ) ;
#85985 = EDGE_LOOP ( 'NONE', ( #113233, #94433, #41416, #6112 ) ) ;
#85986 = DIRECTION ( 'NONE',  ( 0.000000000000000000, 0.000000000000000000, 1.000000000000000000 ) ) ;
#85988 = LINE ( 'NONE', #125922, #124933 ) ;
#85987 = PRODUCT_DEFINITION_CONTEXT ( 'detailed design', #16189, 'design' ) ;
#85989 = CARTESIAN_POINT ( 'NONE',  ( -3.950000000000025491, 12.50000000000000000, 6.083687093685483660 ) ) ;
#85990 = CARTESIAN_POINT ( 'NONE',  ( 8.099999999999923261, 12.50000000000000000, 3.983716857408420076 ) ) ;
#85991 = CARTESIAN_POINT ( 'NONE',  ( -7.700000000000016165, 12.50000000000000000, 0.4115034346978109769 ) ) ;
#85992 = EDGE_CURVE ( 'NONE', #104335, #92609, #10223, .T. ) ;
#85993 = EDGE_LOOP ( 'NONE', ( #55262, #85443, #1668, #121441 ) ) ;
#85994 = CONICAL_SURFACE ( 'NONE', #102719, 0.1000000000000002554, 0.003490658503988666988 ) ;
#85995 = CIRCLE ( 'NONE', #63039, 0.09999999999999999167 ) ;
#85996 = ORIENTED_EDGE ( 'NONE', *, *, #21313, .T. ) ;
#85997 = ORIENTED_EDGE ( 'NONE', *, *, #13973, .T. ) ;
#85998 = ORIENTED_EDGE ( 'NONE', *, *, #92290, .T. ) ;
#85999 = FACE_OUTER_BOUND ( 'NONE', #96582, .T. ) ;
#86000 = ORIENTED_EDGE ( 'NONE', *, *, #106322, .T. ) ;
#86001 = VERTEX_POINT ( 'NONE', #112930 ) ;
#86002 = AXIS2_PLACEMENT_3D ( 'NONE', #114414, #76435, #37167 ) ;
#86003 = DIRECTION ( 'NONE',  ( 0.000000000000000000, 1.000000000000000000, 0.000000000000000000 ) ) ;
#86004 = FACE_OUTER_BOUND ( 'NONE', #72649, .T. ) ;
#86005 = AXIS2_PLACEMENT_3D ( 'NONE', #119420, #29768, #80159 ) ;
#86006 = DIRECTION ( 'NONE',  ( 0.000000000000000000, 0.000000000000000000, 1.000000000000000000 ) ) ;
#86007 = CARTESIAN_POINT ( 'NONE',  ( -11.44999999999999751, 2.500000000000000000, 1.918653347947321564 ) ) ;
#86008 = DIRECTION ( 'NONE',  ( 0.000000000000000000, 0.000000000000000000, 1.000000000000000000 ) ) ;
#86009 = VECTOR ( 'NONE', #97346, 1000.000000000000000 ) ;
#86010 = DIRECTION ( 'NONE',  ( 0.000000000000000000, 1.000000000000000000, 0.000000000000000000 ) ) ;
#86011 = CARTESIAN_POINT ( 'NONE',  ( -3.100000000000028511, 12.50000000000000000, -4.741630453620015118 ) ) ;
#86012 = ORIENTED_EDGE ( 'NONE', *, *, #23827, .F. ) ;
#86013 = CARTESIAN_POINT ( 'NONE',  ( -13.09999999999999076, 2.500000000000000000, 4.083716857408421497 ) ) ;
#86014 = EDGE_LOOP ( 'NONE', ( #72046, #19488, #112074, #78740 ) ) ;
#86015 = DIRECTION ( 'NONE',  ( -0.000000000000000000, -1.000000000000000000, -0.000000000000000000 ) ) ;
#86016 = ADVANCED_FACE ( 'NONE', ( #13427 ), #12777, .T. ) ;
#86017 = ORIENTED_EDGE ( 'NONE', *, *, #121970, .T. ) ;
#86018 = DIRECTION ( 'NONE',  ( -4.274815082592931898E-19, -0.9999939076577903929, -0.003490651415223739937 ) ) ;
#86019 = CONICAL_SURFACE ( 'NONE', #73510, 0.1000000000000002554, 0.003490658503988666988 ) ;
#86020 = CIRCLE ( 'NONE', #44263, 0.09999999999999982514 ) ;
#86021 = FACE_OUTER_BOUND ( 'NONE', #109155, .T. ) ;
#86022 = ORIENTED_EDGE ( 'NONE', *, *, #105688, .F. ) ;
#86023 = CARTESIAN_POINT ( 'NONE',  ( -5.650000000000023448, 12.50000000000000000, -6.776507416713040577 ) ) ;
#86024 = CARTESIAN_POINT ( 'NONE',  ( -11.44999999999999751, 2.500000000000000000, -2.511473670974873951 ) ) ;
#86025 = VERTEX_POINT ( 'NONE', #84104 ) ;
#86026 = EDGE_CURVE ( 'NONE', #91737, #8978, #44847, .T. ) ;
#86027 = DIRECTION ( 'NONE',  ( -0.000000000000000000, 1.000000000000000000, -0.000000000000000000 ) ) ;
#86028 = ORIENTED_EDGE ( 'NONE', *, *, #32919, .F. ) ;
#86029 = EDGE_CURVE ( 'NONE', #45024, #8842, #39426, .T. ) ;
#86031 = ORIENTED_EDGE ( 'NONE', *, *, #10650, .F. ) ;
#86030 = ADVANCED_FACE ( 'NONE', ( #93941 ), #34394, .T. ) ;
#86032 = PLANE ( 'NONE',  #79254 ) ;
#86033 = DIRECTION ( 'NONE',  ( -0.000000000000000000, -1.000000000000000000, -0.000000000000000000 ) ) ;
#86034 = EDGE_CURVE ( 'NONE', #96832, #104331, #124034, .T. ) ;
#86035 = CARTESIAN_POINT ( 'NONE',  ( 186.4218750003414016, 0.000000000000000000, 7.564683531250000925 ) ) ;
#86036 = ADVANCED_FACE ( 'NONE', ( #74304 ), #95836, .T. ) ;
#86037 = CARTESIAN_POINT ( 'NONE',  ( -6.249999999999984901, 12.50000000000000000, -6.430097255199264339 ) ) ;
#86038 = FACE_OUTER_BOUND ( 'NONE', #19167, .T. ) ;
#86039 = EDGE_CURVE ( 'NONE', #98143, #52604, #15350, .T. ) ;
#86040 = DIRECTION ( 'NONE',  ( 0.000000000000000000, 0.000000000000000000, 1.000000000000000000 ) ) ;
#86041 = EDGE_CURVE ( 'NONE', #86648, #110490, #92645, .T. ) ;
#86042 = AXIS2_PLACEMENT_3D ( 'NONE', #43161, #102685, #25404 ) ;
#86043 = AXIS2_PLACEMENT_3D ( 'NONE', #97632, #58372, #36797 ) ;
#86044 = ADVANCED_FACE ( 'NONE', ( #2310 ), #75187, .T. ) ;
#86045 = EDGE_CURVE ( 'NONE', #69532, #87361, #22688, .T. ) ;
#86046 = ORIENTED_EDGE ( 'NONE', *, *, #103334, .T. ) ;
#86047 = EDGE_CURVE ( 'NONE', #100718, #15933, #62680, .T. ) ;
#86048 = CARTESIAN_POINT ( 'NONE',  ( 2.049999999999950084, 2.500000000000000000, -2.165063509461101710 ) ) ;
#86050 = ADVANCED_FACE ( 'NONE', ( #82185 ), #122752, .T. ) ;
#86049 = AXIS2_PLACEMENT_3D ( 'NONE', #21542, #112509, #3832 ) ;
#86051 = VECTOR ( 'NONE', #21291, 1000.000000000000000 ) ;
#86052 = ORIENTED_EDGE ( 'NONE', *, *, #37293, .T. ) ;
#86053 = VECTOR ( 'NONE', #104285, 1000.000000000000000 ) ;
#86054 = DIRECTION ( 'NONE',  ( -0.000000000000000000, 1.000000000000000000, -0.000000000000000000 ) ) ;
#86055 = CARTESIAN_POINT ( 'NONE',  ( 0.8499999999999553468, 2.500000000000000000, 1.472243186433545459 ) ) ;
#86056 = DIRECTION ( 'NONE',  ( 0.000000000000000000, -0.9999939076577903929, 0.003490651415223739937 ) ) ;
#86057 = EDGE_CURVE ( 'NONE', #16616, #65580, #33439, .T. ) ;
#86058 = VERTEX_POINT ( 'NONE', #73008 ) ;
#86059 = DIRECTION ( 'NONE',  ( -0.000000000000000000, -1.000000000000000000, -0.000000000000000000 ) ) ;
#86060 = DIRECTION ( 'NONE',  ( -0.000000000000000000, 1.000000000000000000, -0.000000000000000000 ) ) ;
#86061 = ORIENTED_EDGE ( 'NONE', *, *, #78889, .T. ) ;
#86062 = DIRECTION ( 'NONE',  ( 0.000000000000000000, 0.000000000000000000, 1.000000000000000000 ) ) ;
#86063 = ORIENTED_EDGE ( 'NONE', *, *, #12305, .T. ) ;
#86064 = VERTEX_POINT ( 'NONE', #25184 ) ;
#86065 = PLANE ( 'NONE',  #113716 ) ;
#86066 = VERTEX_POINT ( 'NONE', #22636 ) ;
#86067 = CARTESIAN_POINT ( 'NONE',  ( -5.200000000000025935, 2.500000000000000000, -3.883716857408426648 ) ) ;
#86068 = LINE ( 'NONE', #14116, #42218 ) ;
#86069 = LINE ( 'NONE', #126672, #35460 ) ;
#86070 = AXIS2_PLACEMENT_3D ( 'NONE', #23279, #14097, #104423 ) ;
#86071 = VERTEX_POINT ( 'NONE', #32473 ) ;
#86072 = CIRCLE ( 'NONE', #98597, 0.09999999999999982514 ) ;
#86073 = FACE_BOUND ( 'NONE', #10185, .T. ) ;
#86075 = EDGE_LOOP ( 'NONE', ( #77445, #23410, #115348, #51935 ) ) ;
#86074 = CARTESIAN_POINT ( 'NONE',  ( 13.34999999999990017, 2.500000000000000000, 1.472243186433545459 ) ) ;
#86076 = DIRECTION ( 'NONE',  ( -0.000000000000000000, 1.000000000000000000, -0.000000000000000000 ) ) ;
#86077 = CARTESIAN_POINT ( 'NONE',  ( -10.45000000000000462, 2.500000000000000000, -6.495190528383298911 ) ) ;
#86078 = VERTEX_POINT ( 'NONE', #112295 ) ;
#86079 = VECTOR ( 'NONE', #29063, 1000.000000000000000 ) ;
#86080 = EDGE_CURVE ( 'NONE', #22999, #356, #102091, .T. ) ;
#86081 = AXIS2_PLACEMENT_3D ( 'NONE', #101680, #83949, #36164 ) ;
#86082 = AXIS2_PLACEMENT_3D ( 'NONE', #13451, #74322, #14726 ) ;
#86083 = ORIENTED_EDGE ( 'NONE', *, *, #122241, .F. ) ;
#86084 = EDGE_CURVE ( 'NONE', #97627, #5867, #103107, .T. ) ;
#86085 = EDGE_LOOP ( 'NONE', ( #65546, #99856 ) ) ;
#86086 = CARTESIAN_POINT ( 'NONE',  ( -0.6000000000000323963, 2.500000000000000000, -0.3464101615137759604 ) ) ;
#86087 = DIRECTION ( 'NONE',  ( -0.000000000000000000, -1.000000000000000000, -0.000000000000000000 ) ) ;
#86088 =( BOUNDED_CURVE ( )  B_SPLINE_CURVE ( 2, ( #30182, #695, #118533, #8566, #68799, #19706, #40001 ),
 .UNSPECIFIED., .F., .F. ) 
 B_SPLINE_CURVE_WITH_KNOTS ( ( 3, 2, 2, 3 ),
 ( 0.4285714285714289362, 0.4523809523809527722, 0.4761904761904766081, 0.5000000000000004441 ),
 .UNSPECIFIED. ) 
 CURVE ( )  GEOMETRIC_REPRESENTATION_ITEM ( )  RATIONAL_B_SPLINE_CURVE ( ( 0.9999999999999977796, 0.8660254037844409281, 1.000000000000000000, 0.8660254037844387076, 1.000000000000000000, 0.8660254037844361541, 1.000000000000002442 ) ) 
 REPRESENTATION_ITEM ( '' )  );
#86089 = DIRECTION ( 'NONE',  ( 0.000000000000000000, 0.000000000000000000, 1.000000000000000000 ) ) ;
#86090 = FACE_BOUND ( 'NONE', #38502, .T. ) ;
#86091 = ORIENTED_EDGE ( 'NONE', *, *, #88900, .T. ) ;
#86092 = CARTESIAN_POINT ( 'NONE',  ( 186.3177083336747160, 4.367472073101515306, 7.564683531250000925 ) ) ;
#86093 = LINE ( 'NONE', #25917, #74067 ) ;
#86094 = DIRECTION ( 'NONE',  ( 0.000000000000000000, 1.000000000000000000, 0.000000000000000000 ) ) ;
#86095 = AXIS2_PLACEMENT_3D ( 'NONE', #76922, #107674, #28475 ) ;
#86096 = EDGE_CURVE ( 'NONE', #106091, #67575, #106568, .T. ) ;
#86097 = CIRCLE ( 'NONE', #29691, 0.06509327318403745899 ) ;
#86098 = CIRCLE ( 'NONE', #58942, 0.1000000000000002554 ) ;
#86099 = AXIS2_PLACEMENT_3D ( 'NONE', #6918, #127378, #18046 ) ;
#86100 = DIRECTION ( 'NONE',  ( -4.274815082592931898E-19, -0.9999939076577903929, -0.003490651415223739937 ) ) ;
#86101 = DIRECTION ( 'NONE',  ( 0.000000000000000000, 1.000000000000000000, 0.000000000000000000 ) ) ;
#86102 = DIRECTION ( 'NONE',  ( 0.000000000000000000, 0.000000000000000000, 1.000000000000000000 ) ) ;
#86103 = VECTOR ( 'NONE', #107372, 1000.000000000000000 ) ;
#86104 = CARTESIAN_POINT ( 'NONE',  ( -6.249999999999984901, 2.500000000000000000, -2.165063509461101710 ) ) ;
#86105 = DIRECTION ( 'NONE',  ( 0.000000000000000000, 0.000000000000000000, 1.000000000000000000 ) ) ;
#86106 = ORIENTED_EDGE ( 'NONE', *, *, #124437, .T. ) ;
#86107 = AXIS2_PLACEMENT_3D ( 'NONE', #18992, #127045, #48473 ) ;
#86108 = ORIENTED_EDGE ( 'NONE', *, *, #67709, .F. ) ;
#86109 = ORIENTED_EDGE ( 'NONE', *, *, #109830, .T. ) ;
#86110 = ORIENTED_EDGE ( 'NONE', *, *, #32658, .T. ) ;
#86111 = ORIENTED_EDGE ( 'NONE', *, *, #69291, .T. ) ;
#86112 = DIRECTION ( 'NONE',  ( -4.274815082592931898E-19, -0.9999939076577903929, -0.003490651415223739937 ) ) ;
#86113 = CARTESIAN_POINT ( 'NONE',  ( 9.999999999999952038, 2.500000000000000000, -2.276824562219559311E-15 ) ) ;
#86114 = ORIENTED_EDGE ( 'NONE', *, *, #19094, .F. ) ;
#86115 = FACE_BOUND ( 'NONE', #41479, .T. ) ;
#86116 = DIRECTION ( 'NONE',  ( 0.000000000000000000, -0.9999939076577903929, 0.003490651415223739937 ) ) ;
#86117 = DIRECTION ( 'NONE',  ( 0.000000000000000000, 1.000000000000000000, 0.000000000000000000 ) ) ;
#86118 = FACE_OUTER_BOUND ( 'NONE', #66045, .T. ) ;
#86119 = DIRECTION ( 'NONE',  ( 0.000000000000000000, -0.000000000000000000, 1.000000000000000000 ) ) ;
#86120 = CARTESIAN_POINT ( 'NONE',  ( 108.0000000000000142, 8.500000000000000000, 0.000000000000000000 ) ) ;
#86121 = VERTEX_POINT ( 'NONE', #113578 ) ;
#86122 = DIRECTION ( 'NONE',  ( 0.000000000000000000, 0.000000000000000000, -1.000000000000000000 ) ) ;
#86123 = ORIENTED_EDGE ( 'NONE', *, *, #6971, .F. ) ;
#86124 = ORIENTED_EDGE ( 'NONE', *, *, #54550, .F. ) ;
#86125 = AXIS2_PLACEMENT_3D ( 'NONE', #81607, #24632, #101901 ) ;
#86126 = VERTEX_POINT ( 'NONE', #8124 ) ;
#86127 = CIRCLE ( 'NONE', #111261, 0.1000000000000002554 ) ;
#86128 = DIRECTION ( 'NONE',  ( 0.000000000000000000, 1.000000000000000000, 0.000000000000000000 ) ) ;
#86129 = CONICAL_SURFACE ( 'NONE', #104912, 0.09999999999999999167, 0.003490658503988666988 ) ;
#86130 = CARTESIAN_POINT ( 'NONE',  ( -7.500000000000016875, 12.50000000000000000, 0.6928203230275494784 ) ) ;
#86131 = FACE_OUTER_BOUND ( 'NONE', #11261, .T. ) ;
#86132 = ORIENTED_EDGE ( 'NONE', *, *, #6989, .F. ) ;
#86133 = CARTESIAN_POINT ( 'NONE',  ( 15.62920359459757336, 2.499999999999999556, -5.623946225393742004 ) ) ;
#86134 = CARTESIAN_POINT ( 'NONE',  ( -5.850000000000018296, 12.50000000000000000, 7.188010851410848723 ) ) ;
#86135 = AXIS2_PLACEMENT_3D ( 'NONE', #75785, #17501, #104604 ) ;
#86136 = VECTOR ( 'NONE', #95569, 1000.000000000000000 ) ;
#86137 = CIRCLE ( 'NONE', #35999, 0.09999999999999999167 ) ;
#86138 = CARTESIAN_POINT ( 'NONE',  ( -4.200000000000029488, 2.500000000000000000, -4.430127018922202176 ) ) ;
#86139 = CARTESIAN_POINT ( 'NONE',  ( 184.3645833340161175, -6.668395609140180369, 3.849999999999994760 ) ) ;
#86140 = CARTESIAN_POINT ( 'NONE',  ( 11.04999999999991012, 12.50000000000000000, -1.883746621131363597 ) ) ;
#86142 = EDGE_CURVE ( 'NONE', #41595, #55841, #56571, .T. ) ;
#86141 = CONICAL_SURFACE ( 'NONE', #464, 0.1000000000000000472, 0.003490658503988666988 ) ;
#86143 = CONICAL_SURFACE ( 'NONE', #100823, 0.09999999999999999167, 0.003490658503988666988 ) ;
#86144 = CARTESIAN_POINT ( 'NONE',  ( -11.89999999999999503, 2.500000000000000000, 4.576537180435972019 ) ) ;
#86145 = EDGE_CURVE ( 'NONE', #46062, #122449, #112564, .T. ) ;
#86146 = ORIENTED_EDGE ( 'NONE', *, *, #114868, .F. ) ;
#86147 = CARTESIAN_POINT ( 'NONE',  ( -5.850000000000018296, 2.500000000000000000, 7.188010851410848723 ) ) ;
#86148 = AXIS2_PLACEMENT_3D ( 'NONE', #102622, #12943, #60782 ) ;
#86149 = ORIENTED_EDGE ( 'NONE', *, *, #73607, .F. ) ;
#86150 = ORIENTED_EDGE ( 'NONE', *, *, #48870, .T. ) ;
#86151 = FACE_OUTER_BOUND ( 'NONE', #44175, .T. ) ;
#86152 = DIRECTION ( 'NONE',  ( 0.000000000000000000, -0.000000000000000000, 1.000000000000000000 ) ) ;
#86154 = EDGE_CURVE ( 'NONE', #79643, #27571, #6811, .T. ) ;
#86153 = DIRECTION ( 'NONE',  ( 0.000000000000000000, 0.000000000000000000, 1.000000000000000000 ) ) ;
#86155 = ORIENTED_EDGE ( 'NONE', *, *, #15547, .F. ) ;
#86156 = VERTEX_POINT ( 'NONE', #68339 ) ;
#86157 = DIRECTION ( 'NONE',  ( 0.000000000000000000, 0.000000000000000000, 1.000000000000000000 ) ) ;
#86158 = CARTESIAN_POINT ( 'NONE',  ( 43.29532267389756583, 3.510960536759776485, -3.940524368371014052 ) ) ;
#86159 = FACE_OUTER_BOUND ( 'NONE', #32756, .T. ) ;
#86160 = ORIENTED_EDGE ( 'NONE', *, *, #3647, .F. ) ;
#86161 = ORIENTED_EDGE ( 'NONE', *, *, #92500, .F. ) ;
#86162 = DIRECTION ( 'NONE',  ( 0.000000000000000000, 0.000000000000000000, 1.000000000000000000 ) ) ;
#86164 = EDGE_LOOP ( 'NONE', ( #118341, #85708, #2547, #54781 ) ) ;
#86163 = AXIS2_PLACEMENT_3D ( 'NONE', #916, #79492, #108289 ) ;
#86165 = LINE ( 'NONE', #67161, #58292 ) ;
#86166 = CARTESIAN_POINT ( 'NONE',  ( -11.84999999999999609, 12.50000000000000000, 6.906693963081109722 ) ) ;
#86167 = ORIENTED_EDGE ( 'NONE', *, *, #8514, .T. ) ;
#86168 = DIRECTION ( 'NONE',  ( -0.000000000000000000, 1.000000000000000000, -0.000000000000000000 ) ) ;
#86169 = ADVANCED_FACE ( 'NONE', ( #108263 ), #56107, .T. ) ;
#86170 = DIRECTION ( 'NONE',  ( 0.000000000000000000, 0.000000000000000000, 1.000000000000000000 ) ) ;
#86171 = DIRECTION ( 'NONE',  ( -0.000000000000000000, -1.000000000000000000, -0.000000000000000000 ) ) ;
#86173 = CONICAL_SURFACE ( 'NONE', #69461, 0.1000000000000000472, 0.003490658503988666988 ) ;
#86172 = FACE_OUTER_BOUND ( 'NONE', #66468, .T. ) ;
#86174 = VERTEX_POINT ( 'NONE', #95874 ) ;
#86175 = VECTOR ( 'NONE', #118060, 1000.000000000000000 ) ;
#86177 = EDGE_CURVE ( 'NONE', #49853, #92039, #116785, .T. ) ;
#86176 = AXIS2_PLACEMENT_3D ( 'NONE', #30220, #10540, #30861 ) ;
#86178 = CARTESIAN_POINT ( 'NONE',  ( 7.099999999999927702, 2.500000000000000000, 5.022947341949748790 ) ) ;
#86179 = FACE_OUTER_BOUND ( 'NONE', #4377, .T. ) ;
#86180 = EDGE_LOOP ( 'NONE', ( #3797, #122709, #29793, #89476 ) ) ;
#86181 = ORIENTED_EDGE ( 'NONE', *, *, #94951, .F. ) ;
#86182 = EDGE_CURVE ( 'NONE', #103260, #59034, #127277, .T. ) ;
#86183 = EDGE_CURVE ( 'NONE', #65479, #93927, #121154, .T. ) ;
#86184 = CARTESIAN_POINT ( 'NONE',  ( 185.2552083336747444, 6.551208109652275624, -3.782341765624998686 ) ) ;
#86185 = FACE_OUTER_BOUND ( 'NONE', #105673, .T. ) ;
#86186 = DIRECTION ( 'NONE',  ( -0.000000000000000000, 1.000000000000000000, -0.000000000000000000 ) ) ;
#86187 = EDGE_CURVE ( 'NONE', #85617, #14892, #107624, .T. ) ;
#86188 = FACE_OUTER_BOUND ( 'NONE', #27950, .T. ) ;
#86189 = EDGE_CURVE ( 'NONE', #45669, #73196, #76239, .T. ) ;
#86190 = CARTESIAN_POINT ( 'NONE',  ( -5.000000000000022204, 12.50000000000000000, -0.6928203230275541413 ) ) ;
#86191 = LINE ( 'NONE', #46954, #92429 ) ;
#86192 = VECTOR ( 'NONE', #85154, 1000.000000000000000 ) ;
#86193 = CARTESIAN_POINT ( 'NONE',  ( 16.98713586915519969, 1.503435535904362075, -5.629434499184647223 ) ) ;
#86194 = AXIS2_PLACEMENT_3D ( 'NONE', #47728, #69272, #68641 ) ;
#86195 = CARTESIAN_POINT ( 'NONE',  ( 9.399999999999915090, 12.50000000000000000, -3.983716857408426293 ) ) ;
#86196 = AXIS2_PLACEMENT_3D ( 'NONE', #120489, #61585, #101499 ) ;
#86197 = CONICAL_SURFACE ( 'NONE', #46493, 0.09999999999999999167, 0.003490658503988666988 ) ;
#86198 = CARTESIAN_POINT ( 'NONE',  ( 9.799999999999915445, 12.50000000000000000, -4.676537180435977881 ) ) ;
#86199 = EDGE_CURVE ( 'NONE', #3943, #13317, #125358, .T. ) ;
#86200 = EDGE_CURVE ( 'NONE', #35689, #87216, #16642, .T. ) ;
#86201 = AXIS2_PLACEMENT_3D ( 'NONE', #52323, #43810, #42524 ) ;
#86202 = PLANE ( 'NONE',  #29226 ) ;
#86203 = ORIENTED_EDGE ( 'NONE', *, *, #5208, .F. ) ;
#86204 = EDGE_CURVE ( 'NONE', #29164, #20699, #16482, .T. ) ;
#86205 = AXIS2_PLACEMENT_3D ( 'NONE', #100773, #102087, #13032 ) ;
#86206 = ORIENTED_EDGE ( 'NONE', *, *, #40080, .T. ) ;
#86207 = CARTESIAN_POINT ( 'NONE',  ( 14.59999999999989484, 12.50000000000000000, -0.06509327318403970719 ) ) ;
#86208 = ORIENTED_EDGE ( 'NONE', *, *, #44201, .F. ) ;
#86209 = EDGE_CURVE ( 'NONE', #53658, #11186, #60346, .T. ) ;
#86210 = CARTESIAN_POINT ( 'NONE',  ( -11.84999999999999609, 2.500000000000000000, 1.818653347947321475 ) ) ;
#86211 = CARTESIAN_POINT ( 'NONE',  ( -0.8500000000000390576, 2.500000000000000000, -6.495190528383302464 ) ) ;
#86212 = DIRECTION ( 'NONE',  ( 0.000000000000000000, 1.000000000000000000, 0.000000000000000000 ) ) ;
#86213 = ADVANCED_FACE ( 'NONE', ( #126631 ), #115486, .T. ) ;
#86214 = VERTEX_POINT ( 'NONE', #118080 ) ;
#86215 = LINE ( 'NONE', #26033, #105113 ) ;
#86216 = FACE_OUTER_BOUND ( 'NONE', #33562, .T. ) ;
#86218 = ORIENTED_EDGE ( 'NONE', *, *, #113412, .T. ) ;
#86217 = DIRECTION ( 'NONE',  ( -0.000000000000000000, -1.000000000000000000, -0.000000000000000000 ) ) ;
#86219 = AXIS2_PLACEMENT_3D ( 'NONE', #40032, #2017, #72707 ) ;
#86220 = DIRECTION ( 'NONE',  ( 0.000000000000000000, 0.000000000000000000, 1.000000000000000000 ) ) ;
#86221 = ORIENTED_EDGE ( 'NONE', *, *, #87247, .T. ) ;
#86222 = ORIENTED_EDGE ( 'NONE', *, *, #121200, .T. ) ;
#86223 = ORIENTED_EDGE ( 'NONE', *, *, #97607, .F. ) ;
#86224 = AXIS2_PLACEMENT_3D ( 'NONE', #107703, #86759, #8197 ) ;
#86225 = ORIENTED_EDGE ( 'NONE', *, *, #13929, .F. ) ;
#86226 = DIRECTION ( 'NONE',  ( 0.000000000000000000, 1.000000000000000000, 0.000000000000000000 ) ) ;
#86227 = CIRCLE ( 'NONE', #65300, 0.06509327318403745899 ) ;
#86228 = DIRECTION ( 'NONE',  ( 0.000000000000000000, -0.9999939076577903929, 0.003490651415223739937 ) ) ;
#86229 = DIRECTION ( 'NONE',  ( 0.000000000000000000, 0.000000000000000000, 1.000000000000000000 ) ) ;
#86230 = CARTESIAN_POINT ( 'NONE',  ( -4.150000000000025224, 12.50000000000000000, 6.560283801567334372 ) ) ;
#86232 = ORIENTED_EDGE ( 'NONE', *, *, #95683, .T. ) ;
#86231 = CIRCLE ( 'NONE', #77835, 0.1000000000000002554 ) ;
#86233 = VECTOR ( 'NONE', #8452, 1000.000000000000000 ) ;
#86234 = CONICAL_SURFACE ( 'NONE', #107170, 0.1000000000000002554, 0.003490658503988666988 ) ;
#86235 = LINE ( 'NONE', #126180, #46127 ) ;
#86237 = ORIENTED_EDGE ( 'NONE', *, *, #69188, .T. ) ;
#86236 = AXIS2_PLACEMENT_3D ( 'NONE', #71514, #69583, #109518 ) ;
#86238 = CARTESIAN_POINT ( 'NONE',  ( 59.88087687688727812, -3.776023963367705516, -4.996435080130480877 ) ) ;
#86239 = CARTESIAN_POINT ( 'NONE',  ( 15.23091471310473999, -2.500000000000513367, -7.179421168902700323 ) ) ;
#86240 = CIRCLE ( 'NONE', #6710, 0.06509327318403745899 ) ;
#86241 = CARTESIAN_POINT ( 'NONE',  ( 2.099999999999950351, 2.500000000000000000, -4.430127018922202176 ) ) ;
#86242 = CARTESIAN_POINT ( 'NONE',  ( 18.27284318114671180, -0.4998542452747786746, 4.791717918553223932 ) ) ;
#86243 = CIRCLE ( 'NONE', #57000, 0.06509327318403745899 ) ;
#86244 = EDGE_LOOP ( 'NONE', ( #54199, #37808, #64665, #37045 ) ) ;
#86245 = EDGE_CURVE ( 'NONE', #63643, #68589, #116748, .T. ) ;
#86246 = ORIENTED_EDGE ( 'NONE', *, *, #2981, .T. ) ;
#86247 = ADVANCED_FACE ( 'NONE', ( #95234 ), #66572, .T. ) ;
#86248 = EDGE_LOOP ( 'NONE', ( #100946, #116907, #69725, #66451 ) ) ;
#86249 = PLANE ( 'NONE',  #48193 ) ;
#86250 = CARTESIAN_POINT ( 'NONE',  ( 9.549999999999915445, 12.50000000000000000, -2.165063509461101710 ) ) ;
#86251 = CARTESIAN_POINT ( 'NONE',  ( -9.150000000000009237, 2.500000000000000000, -7.088010851410848190 ) ) ;
#86252 = FACE_BOUND ( 'NONE', #89056, .T. ) ;
#86253 = CARTESIAN_POINT ( 'NONE',  ( 5.849999999999933031, 12.50000000000000000, 7.188010851410848723 ) ) ;
#86254 = CARTESIAN_POINT ( 'NONE',  ( -2.499999999999996003, 12.50000000000000000, -4.330127018922201643 ) ) ;
#86255 = CARTESIAN_POINT ( 'NONE',  ( -4.293440603042597559E-14, 12.50000000000000000, 5.022947341949748790 ) ) ;
#86256 = CARTESIAN_POINT ( 'NONE',  ( -7.500000000000011546, 2.500000000000000000, 3.637306695894644726 ) ) ;
#86257 = AXIS2_PLACEMENT_3D ( 'NONE', #83376, #44084, #113465 ) ;
#86258 = CARTESIAN_POINT ( 'NONE',  ( 185.5885416670080872, -6.551208109652273848, -3.782341765625003571 ) ) ;
#86259 = DIRECTION ( 'NONE',  ( -0.000000000000000000, -1.000000000000000000, -0.000000000000000000 ) ) ;
#86260 = LINE ( 'NONE', #7705, #57415 ) ;
#86261 = AXIS2_PLACEMENT_3D ( 'NONE', #126498, #95105, #85905 ) ;
#86262 = CIRCLE ( 'NONE', #27780, 0.1000000000000002554 ) ;
#86263 = AXIS2_PLACEMENT_3D ( 'NONE', #21758, #101608, #51863 ) ;
#86264 = DIRECTION ( 'NONE',  ( 0.000000000000000000, 0.000000000000000000, 1.000000000000000000 ) ) ;
#86265 = ORIENTED_EDGE ( 'NONE', *, *, #122429, .T. ) ;
#86266 = ORIENTED_EDGE ( 'NONE', *, *, #75507, .T. ) ;
#86267 = EDGE_LOOP ( 'NONE', ( #22917, #8426, #94340, #87521 ) ) ;
#86268 = EDGE_LOOP ( 'NONE', ( #30769, #64474, #128690 ) ) ;
#86269 = LINE ( 'NONE', #106564, #33995 ) ;
#86270 = FACE_BOUND ( 'NONE', #113436, .T. ) ;
#86271 = CONICAL_SURFACE ( 'NONE', #84221, 0.1000000000000002554, 0.003490658503988666988 ) ;
#86272 = CARTESIAN_POINT ( 'NONE',  ( -11.84999999999999609, 2.500000000000000000, 6.148780366869520897 ) ) ;
#86273 = AXIS2_PLACEMENT_3D ( 'NONE', #54476, #52551, #45322 ) ;
#86274 = LINE ( 'NONE', #88197, #43593 ) ;
#86275 = CIRCLE ( 'NONE', #67489, 0.06509327318403745899 ) ;
#86276 = AXIS2_PLACEMENT_3D ( 'NONE', #86554, #127143, #37479 ) ;
#86277 = EDGE_LOOP ( 'NONE', ( #94628, #64376, #115474, #53063 ) ) ;
#86278 = DIRECTION ( 'NONE',  ( 0.000000000000000000, -0.9999939076577903929, 0.003490651415223739937 ) ) ;
#86279 = CARTESIAN_POINT ( 'NONE',  ( -8.950000000000008171, 12.50000000000000000, -2.576566944158915184 ) ) ;
#86280 = ORIENTED_EDGE ( 'NONE', *, *, #58265, .F. ) ;
#86282 = CARTESIAN_POINT ( 'NONE',  ( -10.85000000000000142, 12.50000000000000000, -2.857883832488649745 ) ) ;
#86281 = CIRCLE ( 'NONE', #31934, 0.06509327318403745899 ) ;
#86283 = CARTESIAN_POINT ( 'NONE',  ( -5.400000000000019895, 2.500000000000000000, -0.6928203230275541413 ) ) ;
#86284 = CIRCLE ( 'NONE', #96750, 0.1000000000000000472 ) ;
#86285 = EDGE_CURVE ( 'NONE', #126271, #81614, #33251, .T. ) ;
#86286 = AXIS2_PLACEMENT_3D ( 'NONE', #120739, #29785, #39636 ) ;
#86287 = AXIS2_PLACEMENT_3D ( 'NONE', #55609, #14378, #105359 ) ;
#86288 = VECTOR ( 'NONE', #75853, 1000.000000000000000 ) ;
#86289 = ORIENTED_EDGE ( 'NONE', *, *, #47209, .F. ) ;
#86290 = FACE_OUTER_BOUND ( 'NONE', #72178, .T. ) ;
#86291 = LINE ( 'NONE', #116399, #76775 ) ;
#86292 = AXIS2_PLACEMENT_3D ( 'NONE', #1763, #12860, #121538 ) ;
#86293 = EDGE_CURVE ( 'NONE', #50067, #120204, #116145, .T. ) ;
#86294 = ORIENTED_EDGE ( 'NONE', *, *, #37621, .T. ) ;
#86295 = DIRECTION ( 'NONE',  ( -0.000000000000000000, 1.000000000000000000, -0.000000000000000000 ) ) ;
#86296 = AXIS2_PLACEMENT_3D ( 'NONE', #26745, #107877, #87585 ) ;
#86297 = DIRECTION ( 'NONE',  ( 0.000000000000000000, 0.000000000000000000, 1.000000000000000000 ) ) ;
#86298 = ORIENTED_EDGE ( 'NONE', *, *, #12141, .F. ) ;
#86299 = DIRECTION ( 'NONE',  ( -0.000000000000000000, 1.000000000000000000, -0.000000000000000000 ) ) ;
#86300 = ORIENTED_EDGE ( 'NONE', *, *, #89578, .T. ) ;
#86301 = ADVANCED_FACE ( 'NONE', ( #46125 ), #18558, .T. ) ;
#86302 = EDGE_LOOP ( 'NONE', ( #36016, #9266, #45456, #1809 ) ) ;
#86303 = EDGE_CURVE ( 'NONE', #58472, #21571, #110497, .T. ) ;
#86304 = CARTESIAN_POINT ( 'NONE',  ( -9.800000000000006040, 2.500000000000000000, -4.676537180435974328 ) ) ;
#86305 = VERTEX_POINT ( 'NONE', #58541 ) ;
#86306 = CARTESIAN_POINT ( 'NONE',  ( 4.349999999999939249, 2.500000000000000000, 2.611473670974873151 ) ) ;
#86307 = DIRECTION ( 'NONE',  ( 0.000000000000000000, 0.000000000000000000, 1.000000000000000000 ) ) ;
#86308 = ORIENTED_EDGE ( 'NONE', *, *, #21604, .F. ) ;
#86309 = CARTESIAN_POINT ( 'NONE',  ( -1.650000000000034328, 2.500000000000000000, -7.188010851410854052 ) ) ;
#86310 = CARTESIAN_POINT ( 'NONE',  ( -12.89999999999999325, 2.500000000000000000, 0.7928203230275536750 ) ) ;
#86311 = DIRECTION ( 'NONE',  ( 0.000000000000000000, -0.000000000000000000, 1.000000000000000000 ) ) ;
#86312 = DIRECTION ( 'NONE',  ( 0.000000000000000000, -0.9999939076577903929, 0.003490651415223739937 ) ) ;
#86313 = AXIS2_PLACEMENT_3D ( 'NONE', #39256, #7169, #47764 ) ;
#86315 = EDGE_CURVE ( 'NONE', #26633, #55841, #91718, .T. ) ;
#86314 = DIRECTION ( 'NONE',  ( 0.000000000000000000, 0.000000000000000000, -1.000000000000000000 ) ) ;
#86316 = CARTESIAN_POINT ( 'NONE',  ( -1.450000000000035927, 2.500000000000000000, -6.248780366869526759 ) ) ;
#86317 = ORIENTED_EDGE ( 'NONE', *, *, #8475, .T. ) ;
#86318 = ORIENTED_EDGE ( 'NONE', *, *, #13931, .F. ) ;
#86319 = DIRECTION ( 'NONE',  ( 0.000000000000000000, -0.000000000000000000, 1.000000000000000000 ) ) ;
#86320 = AXIS2_PLACEMENT_3D ( 'NONE', #102510, #101226, #81577 ) ;
#86321 = AXIS2_PLACEMENT_3D ( 'NONE', #81155, #30132, #51696 ) ;
#86322 = CARTESIAN_POINT ( 'NONE',  ( 20.37757664703727656, -0.6627606010238995538, 4.188167776336781500 ) ) ;
#86323 = AXIS2_PLACEMENT_3D ( 'NONE', #67967, #47707, #127547 ) ;
#86325 = DIRECTION ( 'NONE',  ( 0.000000000000000000, 1.000000000000000000, 0.000000000000000000 ) ) ;
#86324 = CIRCLE ( 'NONE', #11105, 0.1000000000000002554 ) ;
#86327 = EDGE_LOOP ( 'NONE', ( #62744, #23736 ) ) ;
#86326 = EDGE_LOOP ( 'NONE', ( #123072, #66644, #32636, #108594 ) ) ;
#86328 = ORIENTED_EDGE ( 'NONE', *, *, #37850, .T. ) ;
#86329 = CARTESIAN_POINT ( 'NONE',  ( -11.04999999999999893, 12.50000000000000000, 6.148780366869520009 ) ) ;
#86330 = DIRECTION ( 'NONE',  ( 0.000000000000000000, 0.000000000000000000, 1.000000000000000000 ) ) ;
#86331 = AXIS2_PLACEMENT_3D ( 'NONE', #67538, #57755, #117939 ) ;
#86333 = DIRECTION ( 'NONE',  ( 0.000000000000000000, -0.9999939076577903929, 0.003490651415223739937 ) ) ;
#86332 = VECTOR ( 'NONE', #58076, 1000.000000000000000 ) ;
#86334 = APPLICATION_PROTOCOL_DEFINITION ( 'draft international standard', 'automotive_design', 1998, #31330 ) ;
#86335 = CARTESIAN_POINT ( 'NONE',  ( 3.149999999999944400, 2.500000000000000000, 1.818653347947321475 ) ) ;
#86336 = CARTESIAN_POINT ( 'NONE',  ( 187.5000000000000000, 0.000000000000000000, 0.000000000000000000 ) ) ;
#86337 = AXIS2_PLACEMENT_3D ( 'NONE', #23378, #32599, #13558 ) ;
#86338 = DIRECTION ( 'NONE',  ( 0.000000000000000000, 1.000000000000000000, 0.000000000000000000 ) ) ;
#86339 = DIRECTION ( 'NONE',  ( 0.000000000000000000, 0.000000000000000000, 1.000000000000000000 ) ) ;
#86340 = AXIS2_PLACEMENT_3D ( 'NONE', #90858, #23392, #62700 ) ;
#86341 = DIRECTION ( 'NONE',  ( -0.000000000000000000, -1.000000000000000000, -0.000000000000000000 ) ) ;
#86342 = AXIS2_PLACEMENT_3D ( 'NONE', #98284, #100235, #10541 ) ;
#86343 = ORIENTED_EDGE ( 'NONE', *, *, #118017, .T. ) ;
#86344 = EDGE_CURVE ( 'NONE', #67419, #107723, #56197, .T. ) ;
#86345 = CARTESIAN_POINT ( 'NONE',  ( -4.800000000000022915, 12.50000000000000000, 4.048810130592458201 ) ) ;
#86346 = EDGE_LOOP ( 'NONE', ( #51649, #13345 ) ) ;
#86347 = ORIENTED_EDGE ( 'NONE', *, *, #43197, .T. ) ;
#86348 = EDGE_CURVE ( 'NONE', #128842, #77757, #104242, .T. ) ;
#86349 = CARTESIAN_POINT ( 'NONE',  ( 108.0000000000000142, 5.000000000000000000, -5.000000000000004441 ) ) ;
#86350 = CARTESIAN_POINT ( 'NONE',  ( 7.949999999999925571, 12.50000000000000000, 2.165063509461097713 ) ) ;
#86351 = DIRECTION ( 'NONE',  ( 0.000000000000000000, 0.000000000000000000, 1.000000000000000000 ) ) ;
#86352 = EDGE_CURVE ( 'NONE', #44450, #53076, #110835, .T. ) ;
#86353 = CIRCLE ( 'NONE', #65429, 0.1000000000000002554 ) ;
#86354 = DIRECTION ( 'NONE',  ( 0.000000000000000000, 0.000000000000000000, 1.000000000000000000 ) ) ;
#86355 = DIRECTION ( 'NONE',  ( 0.000000000000000000, 0.000000000000000000, 1.000000000000000000 ) ) ;
#86356 = CARTESIAN_POINT ( 'NONE',  ( 2.699999999999945555, 2.500000000000000000, 3.983716857408420076 ) ) ;
#86357 = DIRECTION ( 'NONE',  ( 0.000000000000000000, -0.000000000000000000, 1.000000000000000000 ) ) ;
#86358 = ORIENTED_EDGE ( 'NONE', *, *, #60380, .T. ) ;
#86359 = DIRECTION ( 'NONE',  ( 0.000000000000000000, 0.000000000000000000, 1.000000000000000000 ) ) ;
#86360 = EDGE_CURVE ( 'NONE', #35274, #40007, #61102, .T. ) ;
#86361 = EDGE_CURVE ( 'NONE', #125999, #65236, #81260, .T. ) ;
#86362 = EDGE_CURVE ( 'NONE', #30351, #25527, #11356, .T. ) ;
#86363 = EDGE_CURVE ( 'NONE', #26544, #118638, #93782, .T. ) ;
#86364 = AXIS2_PLACEMENT_3D ( 'NONE', #83677, #113127, #94780 ) ;
#86366 = CIRCLE ( 'NONE', #36216, 2.318304356886072615 ) ;
#86365 = DIRECTION ( 'NONE',  ( 0.000000000000000000, 0.000000000000000000, -1.000000000000000000 ) ) ;
#86367 = VERTEX_POINT ( 'NONE', #83168 ) ;
#86368 = AXIS2_PLACEMENT_3D ( 'NONE', #74715, #123796, #56351 ) ;
#86369 = VERTEX_POINT ( 'NONE', #98428 ) ;
#86370 = EDGE_CURVE ( 'NONE', #122996, #98982, #8086, .T. ) ;
#86371 = ORIENTED_EDGE ( 'NONE', *, *, #106482, .T. ) ;
#86372 = ORIENTED_EDGE ( 'NONE', *, *, #18403, .F. ) ;
#86373 = VECTOR ( 'NONE', #1909, 1000.000000000000000 ) ;
#86374 = FACE_OUTER_BOUND ( 'NONE', #7061, .T. ) ;
#86375 = FACE_OUTER_BOUND ( 'NONE', #34666, .T. ) ;
#86376 = CIRCLE ( 'NONE', #111515, 0.06509327318403745899 ) ;
#86377 = ADVANCED_FACE ( 'NONE', ( #73323 ), #47816, .T. ) ;
#86378 = AXIS2_PLACEMENT_3D ( 'NONE', #26605, #88069, #99221 ) ;
#86379 = ORIENTED_EDGE ( 'NONE', *, *, #74426, .T. ) ;
#86380 = CARTESIAN_POINT ( 'NONE',  ( 12.69999999999989981, 2.500000000000000000, -0.3464101615137783474 ) ) ;
#86381 = CONICAL_SURFACE ( 'NONE', #29968, 0.09999999999999982514, 0.003490658503988666988 ) ;
#86382 = CARTESIAN_POINT ( 'NONE',  ( 17.50000000000000000, 0.9166666666666685170, -2.864912725862979848 ) ) ;
#86383 = DIRECTION ( 'NONE',  ( 0.000000000000000000, 1.000000000000000000, 0.000000000000000000 ) ) ;
#86384 = ORIENTED_EDGE ( 'NONE', *, *, #16294, .T. ) ;
#86385 = FACE_OUTER_BOUND ( 'NONE', #64204, .T. ) ;
#86386 = DIRECTION ( 'NONE',  ( 0.000000000000000000, -0.9999939076577903929, 0.003490651415223739937 ) ) ;
#86387 = EDGE_LOOP ( 'NONE', ( #117701, #94652, #24200, #38230 ) ) ;
#86388 = CONICAL_SURFACE ( 'NONE', #63418, 0.1000000000000002554, 0.003490658503988666988 ) ;
#86389 = CIRCLE ( 'NONE', #38293, 10.00000000000000000 ) ;
#86390 = ORIENTED_EDGE ( 'NONE', *, *, #99675, .F. ) ;
#86391 = EDGE_LOOP ( 'NONE', ( #106307, #25259, #59588, #88366 ) ) ;
#86392 = FACE_OUTER_BOUND ( 'NONE', #94820, .T. ) ;
#86393 = CIRCLE ( 'NONE', #101172, 0.1000000000000002554 ) ;
#86394 = CARTESIAN_POINT ( 'NONE',  ( 108.0000000000000142, 9.000000000000001776, 2.749999999999997335 ) ) ;
#86395 = ORIENTED_EDGE ( 'NONE', *, *, #1907, .T. ) ;
#86396 = CARTESIAN_POINT ( 'NONE',  ( -3.100000000000028511, 2.500000000000000000, -0.4464101615137782142 ) ) ;
#86397 = FACE_OUTER_BOUND ( 'NONE', #108564, .T. ) ;
#86398 = CARTESIAN_POINT ( 'NONE',  ( -7.950000000000012612, 12.50000000000000000, -2.165063509461101710 ) ) ;
#86399 = LINE ( 'NONE', #46475, #29494 ) ;
#86400 = EDGE_LOOP ( 'NONE', ( #109664, #107687 ) ) ;
#86401 = DIRECTION ( 'NONE',  ( 0.000000000000000000, 0.000000000000000000, -1.000000000000000000 ) ) ;
#86402 = EDGE_CURVE ( 'NONE', #6482, #84545, #39563, .T. ) ;
#86403 = ORIENTED_EDGE ( 'NONE', *, *, #47928, .T. ) ;
#86404 = EDGE_LOOP ( 'NONE', ( #44660, #35169, #48107, #17368 ) ) ;
#86405 = AXIS2_PLACEMENT_3D ( 'NONE', #46419, #55606, #95539 ) ;
#86406 = ORIENTED_EDGE ( 'NONE', *, *, #95401, .F. ) ;
#86407 = CIRCLE ( 'NONE', #84365, 0.09999999999999982514 ) ;
#86408 = CARTESIAN_POINT ( 'NONE',  ( -9.550000000000006040, 12.50000000000000000, 2.165063509461097713 ) ) ;
#86409 = FACE_BOUND ( 'NONE', #109021, .T. ) ;
#86410 = DIRECTION ( 'NONE',  ( -4.274815082592931898E-19, -0.9999939076577903929, -0.003490651415223739937 ) ) ;
#86411 = DIRECTION ( 'NONE',  ( 0.000000000000000000, -0.000000000000000000, 1.000000000000000000 ) ) ;
#86412 = CARTESIAN_POINT ( 'NONE',  ( -4.800000000000028244, 2.500000000000000000, -3.983716857408426293 ) ) ;
#86413 = EDGE_CURVE ( 'NONE', #119463, #116333, #80104, .T. ) ;
#86414 = AXIS2_PLACEMENT_3D ( 'NONE', #63878, #103803, #65137 ) ;
#86415 = AXIS2_PLACEMENT_3D ( 'NONE', #86856, #35831, #125492 ) ;
#86416 = CONICAL_SURFACE ( 'NONE', #55135, 0.1000000000000000472, 0.003490658503988666988 ) ;
#86417 = AXIS2_PLACEMENT_3D ( 'NONE', #83611, #31930, #114974 ) ;
#86418 = CONICAL_SURFACE ( 'NONE', #96885, 0.1000000000000002554, 0.003490658503988666988 ) ;
#86419 = EDGE_LOOP ( 'NONE', ( #90006, #127590 ) ) ;
#86420 = CARTESIAN_POINT ( 'NONE',  ( -6.850000000000017408, 12.50000000000000000, -6.906693963081115051 ) ) ;
#86421 = CARTESIAN_POINT ( 'NONE',  ( -7.300000000000013145, 2.500000000000000000, 3.983716857408420076 ) ) ;
#86422 = DIRECTION ( 'NONE',  ( -0.000000000000000000, 1.000000000000000000, -0.000000000000000000 ) ) ;
#86423 = CARTESIAN_POINT ( 'NONE',  ( -4.600000000000028955, 2.500000000000000000, -4.230127018922201998 ) ) ;
#86424 = ORIENTED_EDGE ( 'NONE', *, *, #55054, .T. ) ;
#86426 = DIRECTION ( 'NONE',  ( 0.000000000000000000, -0.000000000000000000, 1.000000000000000000 ) ) ;
#86425 = AXIS2_PLACEMENT_3D ( 'NONE', #22982, #62899, #102802 ) ;
#86427 = CIRCLE ( 'NONE', #30022, 0.1000000000000002554 ) ;
#86428 = CONICAL_SURFACE ( 'NONE', #40498, 0.1000000000000002554, 0.003490658503988666988 ) ;
#86429 = FACE_OUTER_BOUND ( 'NONE', #64924, .T. ) ;
#86430 = AXIS2_PLACEMENT_3D ( 'NONE', #35165, #126760, #4363 ) ;
#86431 = ORIENTED_EDGE ( 'NONE', *, *, #93162, .T. ) ;
#86432 = CONICAL_SURFACE ( 'NONE', #115677, 0.1000000000000002554, 0.003490658503988666988 ) ;
#86433 = CARTESIAN_POINT ( 'NONE',  ( -9.150000000000009237, 12.50000000000000000, -6.495190528383297135 ) ) ;
#86434 = CARTESIAN_POINT ( 'NONE',  ( 11.24999999999994493, 12.50000000000000000, 6.560283801567334372 ) ) ;
#86435 = FACE_BOUND ( 'NONE', #2317, .T. ) ;
#86436 = DIRECTION ( 'NONE',  ( -0.000000000000000000, 1.000000000000000000, -0.000000000000000000 ) ) ;
#86437 = ORIENTED_EDGE ( 'NONE', *, *, #2270, .T. ) ;
#86438 = FACE_OUTER_BOUND ( 'NONE', #95071, .T. ) ;
#86439 = DIRECTION ( 'NONE',  ( 0.000000000000000000, -0.9999939076577903929, 0.003490651415223739937 ) ) ;
#86440 = ORIENTED_EDGE ( 'NONE', *, *, #100074, .T. ) ;
#86441 = VERTEX_POINT ( 'NONE', #48718 ) ;
#86442 = CARTESIAN_POINT ( 'NONE',  ( 184.1718750003414016, 9.264065473108010111E-16, -7.564683531250000925 ) ) ;
#86444 = EDGE_LOOP ( 'NONE', ( #10023, #125968 ) ) ;
#86443 = AXIS2_PLACEMENT_3D ( 'NONE', #86421, #116527, #126360 ) ;
#86445 = CARTESIAN_POINT ( 'NONE',  ( 185.5885416670080872, -6.551208109652273848, -3.782341765625003571 ) ) ;
#86446 = CARTESIAN_POINT ( 'NONE',  ( -9.800000000000004263, 2.500000000000000000, 3.983716857408420076 ) ) ;
#86447 = EDGE_CURVE ( 'NONE', #10025, #64587, #3880, .T. ) ;
#86448 = CARTESIAN_POINT ( 'NONE',  ( -1.900000000000034550, 2.500000000000000000, 4.676537180435972552 ) ) ;
#86449 = CARTESIAN_POINT ( 'NONE',  ( 11.24999999999994493, 2.500000000000000000, 6.495190528383297135 ) ) ;
#86450 = AXIS2_PLACEMENT_3D ( 'NONE', #21372, #22039, #29915 ) ;
#86451 = VECTOR ( 'NONE', #36881, 1000.000000000000000 ) ;
#86452 = EDGE_CURVE ( 'NONE', #82955, #65404, #118729, .T. ) ;
#86453 = CONICAL_SURFACE ( 'NONE', #32113, 0.1000000000000002554, 0.003490658503988666988 ) ;
#86454 = ORIENTED_EDGE ( 'NONE', *, *, #70778, .T. ) ;
#86455 = DIRECTION ( 'NONE',  ( 0.000000000000000000, -0.9999939076577903929, 0.003490651415223739937 ) ) ;
#86456 = CARTESIAN_POINT ( 'NONE',  ( -3.550000000000027356, 2.500000000000000000, -2.511473670974877948 ) ) ;
#86457 = DIRECTION ( 'NONE',  ( -4.274815082592931898E-19, -0.9999939076577903929, -0.003490651415223739937 ) ) ;
#86458 = DIRECTION ( 'NONE',  ( 0.000000000000000000, -0.9999939076577903929, 0.003490651415223739937 ) ) ;
#86459 = VERTEX_POINT ( 'NONE', #9426 ) ;
#86460 = EDGE_CURVE ( 'NONE', #62381, #12101, #14331, .T. ) ;
#86461 = DIRECTION ( 'NONE',  ( -0.000000000000000000, 1.000000000000000000, -0.000000000000000000 ) ) ;
#86462 = EDGE_LOOP ( 'NONE', ( #6945, #91167 ) ) ;
#86463 = CIRCLE ( 'NONE', #55180, 0.06509327318403745899 ) ;
#86464 = ADVANCED_FACE ( 'NONE', ( #119366 ), #29709, .T. ) ;
#86465 = DIRECTION ( 'NONE',  ( -0.000000000000000000, 1.000000000000000000, -0.000000000000000000 ) ) ;
#86466 = FACE_OUTER_BOUND ( 'NONE', #72366, .T. ) ;
#86467 = ORIENTED_EDGE ( 'NONE', *, *, #83534, .F. ) ;
#86469 = CARTESIAN_POINT ( 'NONE',  ( -4.150000000000025224, 2.500000000000000000, -1.472243186433550122 ) ) ;
#86468 = AXIS2_PLACEMENT_3D ( 'NONE', #31770, #30497, #102439 ) ;
#86470 = CARTESIAN_POINT ( 'NONE',  ( 87.50000000000000000, -4.424430252271037922, -6.079088403633667426 ) ) ;
#86471 = VECTOR ( 'NONE', #42305, 1000.000000000000000 ) ;
#86472 = CARTESIAN_POINT ( 'NONE',  ( 9.999999999999948486, 12.50000000000000000, 4.395220292106234439 ) ) ;
#86473 = DIRECTION ( 'NONE',  ( -4.274815082592931898E-19, -0.9999939076577903929, -0.003490651415223739937 ) ) ;
#86474 = ORIENTED_EDGE ( 'NONE', *, *, #51343, .T. ) ;
#86475 = ADVANCED_FACE ( 'NONE', ( #59846 ), #120962, .T. ) ;
#86476 = CARTESIAN_POINT ( 'NONE',  ( 5.849999999999933031, 2.500000000000000000, 7.188010851410848723 ) ) ;
#86477 = DIRECTION ( 'NONE',  ( 0.000000000000000000, 0.000000000000000000, 1.000000000000000000 ) ) ;
#86478 = CARTESIAN_POINT ( 'NONE',  ( 186.2343750003414016, 8.734944146203032389, 5.348610694689227483E-16 ) ) ;
#86479 = DIRECTION ( 'NONE',  ( -0.000000000000000000, 1.000000000000000000, -0.000000000000000000 ) ) ;
#86480 = EDGE_CURVE ( 'NONE', #47772, #86058, #125011, .T. ) ;
#86481 = DIRECTION ( 'NONE',  ( 0.000000000000000000, -0.9999939076577903929, 0.003490651415223739937 ) ) ;
#86482 = ORIENTED_EDGE ( 'NONE', *, *, #96524, .T. ) ;
#86483 = VERTEX_POINT ( 'NONE', #26173 ) ;
#86484 = CARTESIAN_POINT ( 'NONE',  ( 0.5999999999999547917, 2.500000000000000000, 3.983716857408420076 ) ) ;
#86486 = ORIENTED_EDGE ( 'NONE', *, *, #48875, .F. ) ;
#86485 = VECTOR ( 'NONE', #25731, 1000.000000000000000 ) ;
#86487 = DIRECTION ( 'NONE',  ( 0.000000000000000000, 0.000000000000000000, -1.000000000000000000 ) ) ;
#86489 = ORIENTED_EDGE ( 'NONE', *, *, #127819, .F. ) ;
#86488 = ORIENTED_EDGE ( 'NONE', *, *, #3443, .T. ) ;
#86490 = ORIENTED_EDGE ( 'NONE', *, *, #62602, .F. ) ;
#86491 = CIRCLE ( 'NONE', #25957, 0.06509327318403745899 ) ;
#86492 = DIRECTION ( 'NONE',  ( -0.000000000000000000, -1.000000000000000000, -0.000000000000000000 ) ) ;
#86493 = VECTOR ( 'NONE', #128491, 1000.000000000000000 ) ;
#86494 = DIRECTION ( 'NONE',  ( 0.000000000000000000, 0.000000000000000000, -1.000000000000000000 ) ) ;
#86495 = DIRECTION ( 'NONE',  ( 0.000000000000000000, -0.000000000000000000, 1.000000000000000000 ) ) ;
#86496 = DIRECTION ( 'NONE',  ( 0.000000000000000000, 0.000000000000000000, 1.000000000000000000 ) ) ;
#86497 = DIRECTION ( 'NONE',  ( -4.274815082592931898E-19, -0.9999939076577903929, -0.003490651415223739937 ) ) ;
#86498 = CARTESIAN_POINT ( 'NONE',  ( -3.750000000000027978, 12.50000000000000000, 7.188010851410848723 ) ) ;
#86499 = VERTEX_POINT ( 'NONE', #126309 ) ;
#86500 = DIRECTION ( 'NONE',  ( 0.000000000000000000, -0.000000000000000000, 1.000000000000000000 ) ) ;
#86501 = ORIENTED_EDGE ( 'NONE', *, *, #25303, .F. ) ;
#86502 = ORIENTED_EDGE ( 'NONE', *, *, #1956, .T. ) ;
#86503 = ORIENTED_EDGE ( 'NONE', *, *, #103667, .T. ) ;
#86504 = EDGE_LOOP ( 'NONE', ( #51230, #53004 ) ) ;
#86505 = DIRECTION ( 'NONE',  ( 0.000000000000000000, 0.000000000000000000, -1.000000000000000000 ) ) ;
#86506 = CONICAL_SURFACE ( 'NONE', #46814, 0.09999999999999982514, 0.003490658503988666988 ) ;
#86507 = ORIENTED_EDGE ( 'NONE', *, *, #65788, .F. ) ;
#86508 = VERTEX_POINT ( 'NONE', #85084 ) ;
#86510 = DIRECTION ( 'NONE',  ( 0.000000000000000000, 0.000000000000000000, 1.000000000000000000 ) ) ;
#86509 = CONICAL_SURFACE ( 'NONE', #4926, 0.1000000000000002554, 0.003490658503988666988 ) ;
#86511 = AXIS2_PLACEMENT_3D ( 'NONE', #84120, #24567, #54031 ) ;
#86512 = LINE ( 'NONE', #115981, #94239 ) ;
#86513 = DIRECTION ( 'NONE',  ( 0.000000000000000000, 1.000000000000000000, 0.000000000000000000 ) ) ;
#86514 = CARTESIAN_POINT ( 'NONE',  ( -6.250000000000021316, 2.500000000000000000, -1.572243186433550211 ) ) ;
#86515 = AXIS2_PLACEMENT_3D ( 'NONE', #2290, #33084, #3596 ) ;
#86517 = ADVANCED_FACE ( 'NONE', ( #115834 ), #125641, .T. ) ;
#86516 = VECTOR ( 'NONE', #19750, 1000.000000000000000 ) ;
#86518 = FACE_OUTER_BOUND ( 'NONE', #9379, .T. ) ;
#86519 = EDGE_LOOP ( 'NONE', ( #114944, #113191 ) ) ;
#86520 = ADVANCED_FACE ( 'NONE', ( #75905 ), #43616, .T. ) ;
#86521 = EDGE_CURVE ( 'NONE', #90795, #121936, #14398, .T. ) ;
#86522 = DIRECTION ( 'NONE',  ( 0.000000000000000000, -0.9999939076577903929, 0.003490651415223739937 ) ) ;
#86523 = EDGE_CURVE ( 'NONE', #57299, #123681, #97970, .T. ) ;
#86524 = AXIS2_PLACEMENT_3D ( 'NONE', #54838, #75771, #23457 ) ;
#86526 = VERTEX_POINT ( 'NONE', #66084 ) ;
#86525 = CONICAL_SURFACE ( 'NONE', #40595, 0.1000000000000000472, 0.003490658503988666988 ) ;
#86527 = DIRECTION ( 'NONE',  ( 0.000000000000000000, 1.000000000000000000, 0.000000000000000000 ) ) ;
#86528 = AXIS2_PLACEMENT_3D ( 'NONE', #112702, #102238, #101591 ) ;
#86529 = ORIENTED_EDGE ( 'NONE', *, *, #59793, .F. ) ;
#86530 = DIRECTION ( 'NONE',  ( 0.000000000000000000, 0.000000000000000000, 1.000000000000000000 ) ) ;
#86531 = EDGE_CURVE ( 'NONE', #20260, #38135, #41564, .T. ) ;
#86532 = ORIENTED_EDGE ( 'NONE', *, *, #62292, .F. ) ;
#86533 = VERTEX_POINT ( 'NONE', #73983 ) ;
#86534 = DIRECTION ( 'NONE',  ( 0.000000000000000000, -0.000000000000000000, 1.000000000000000000 ) ) ;
#86535 = DIRECTION ( 'NONE',  ( -4.274815082592931898E-19, -0.9999939076577903929, -0.003490651415223739937 ) ) ;
#86536 = EDGE_CURVE ( 'NONE', #58995, #105130, #95558, .T. ) ;
#86537 = EDGE_CURVE ( 'NONE', #53182, #43603, #123115, .T. ) ;
#86538 = CARTESIAN_POINT ( 'NONE',  ( 14.14999999999989733, 2.500000000000000000, 1.372243186433545370 ) ) ;
#86539 = CARTESIAN_POINT ( 'NONE',  ( 1.849999999999951017, 2.500000000000000000, -6.048780366869526581 ) ) ;
#86540 = CARTESIAN_POINT ( 'NONE',  ( 1.249999999999986899, 12.50000000000000000, 6.560283801567334372 ) ) ;
#86541 = ORIENTED_EDGE ( 'NONE', *, *, #40879, .T. ) ;
#86542 = CARTESIAN_POINT ( 'NONE',  ( -9.800000000000004263, 12.50000000000000000, 3.918623584224382839 ) ) ;
#86543 = CARTESIAN_POINT ( 'NONE',  ( 12.49999999999990585, 2.500000000000000000, 3.637306695894644726 ) ) ;
#86544 =( REPRESENTATION_RELATIONSHIP ('NONE','NONE', #102928, #89551 ) REPRESENTATION_RELATIONSHIP_WITH_TRANSFORMATION ( #49670 )SHAPE_REPRESENTATION_RELATIONSHIP( ) );
#86545 = DIRECTION ( 'NONE',  ( 0.000000000000000000, 1.000000000000000000, 0.000000000000000000 ) ) ;
#86546 = DIRECTION ( 'NONE',  ( 0.000000000000000000, 0.000000000000000000, 1.000000000000000000 ) ) ;
#86547 = AXIS2_PLACEMENT_3D ( 'NONE', #18106, #125488, #55469 ) ;
#86548 = DIRECTION ( 'NONE',  ( 0.000000000000000000, 0.000000000000000000, -1.000000000000000000 ) ) ;
#86549 = ORIENTED_EDGE ( 'NONE', *, *, #5055, .T. ) ;
#86550 = ORIENTED_EDGE ( 'NONE', *, *, #84116, .F. ) ;
#86551 = DIRECTION ( 'NONE',  ( 0.000000000000000000, 0.000000000000000000, 1.000000000000000000 ) ) ;
#86552 = EDGE_LOOP ( 'NONE', ( #41742, #52168, #128488, #95316 ) ) ;
#86553 = CIRCLE ( 'NONE', #42671, 0.1000000000000002554 ) ;
#86554 = CARTESIAN_POINT ( 'NONE',  ( -8.150000000000012790, 2.500000000000000000, 2.511473670974873507 ) ) ;
#86555 = FACE_OUTER_BOUND ( 'NONE', #61662, .T. ) ;
#86556 = CIRCLE ( 'NONE', #44812, 0.1000000000000002554 ) ;
#86557 = ORIENTED_EDGE ( 'NONE', *, *, #112788, .F. ) ;
#86558 = CARTESIAN_POINT ( 'NONE',  ( 185.1666666666666856, -6.668395609140176816, -3.850000000000003642 ) ) ;
#86559 = CARTESIAN_POINT ( 'NONE',  ( 2.000000000000000000, 0.000000000000000000, -5.000000000000004441 ) ) ;
#86560 = CARTESIAN_POINT ( 'NONE',  ( 7.699999999999925571, 2.500000000000000000, -4.676537180435978769 ) ) ;
#86561 = LINE ( 'NONE', #16519, #9974 ) ;
#86562 = ORIENTED_EDGE ( 'NONE', *, *, #92411, .T. ) ;
#86563 = AXIS2_PLACEMENT_3D ( 'NONE', #65793, #105731, #27802 ) ;
#86564 = CARTESIAN_POINT ( 'NONE',  ( 16.56576425165007649, -1.499999999999997113, -6.084390597445788806 ) ) ;
#86565 = CARTESIAN_POINT ( 'NONE',  ( 8.099999999999921485, 12.50000000000000000, 0.2813168883297361700 ) ) ;
#86566 = VERTEX_POINT ( 'NONE', #113251 ) ;
#86567 = FACE_OUTER_BOUND ( 'NONE', #57548, .T. ) ;
#86568 = DIRECTION ( 'NONE',  ( 0.000000000000000000, 1.000000000000000000, 0.000000000000000000 ) ) ;
#86569 = CARTESIAN_POINT ( 'NONE',  ( -13.09999999999999076, 2.500000000000000000, 4.676537180435972552 ) ) ;
#86570 = EDGE_CURVE ( 'NONE', #83172, #27784, #55629, .T. ) ;
#86571 = ORIENTED_EDGE ( 'NONE', *, *, #87093, .F. ) ;
#86572 = CIRCLE ( 'NONE', #30166, 0.1000000000000002554 ) ;
#86573 = VECTOR ( 'NONE', #23515, 1000.000000000000000 ) ;
#86574 = CIRCLE ( 'NONE', #5000, 0.1000000000000002554 ) ;
#86575 = CARTESIAN_POINT ( 'NONE',  ( -11.64999999999999858, 12.50000000000000000, -1.472243186433546125 ) ) ;
#86577 = ORIENTED_EDGE ( 'NONE', *, *, #15215, .T. ) ;
#86576 = CONICAL_SURFACE ( 'NONE', #67705, 0.1000000000000000472, 0.003490658503988666988 ) ;
#86578 = CARTESIAN_POINT ( 'NONE',  ( 9.399999999999915090, 2.500000000000000000, 4.083716857408421497 ) ) ;
#86579 = CARTESIAN_POINT ( 'NONE',  ( -4.350000000000023626, 2.500000000000000000, -2.511473670974877948 ) ) ;
#86580 = FACE_OUTER_BOUND ( 'NONE', #60434, .T. ) ;
#86581 = AXIS2_PLACEMENT_3D ( 'NONE', #80332, #40419, #107848 ) ;
#86582 = EDGE_LOOP ( 'NONE', ( #48162, #53245, #114823, #50219 ) ) ;
#86583 = CARTESIAN_POINT ( 'NONE',  ( 10.39999999999990976, 2.500000000000000000, -4.430127018922202176 ) ) ;
#86584 = CARTESIAN_POINT ( 'NONE',  ( -2.900000000000029221, 2.500000000000000000, -2.276824562219559311E-15 ) ) ;
#86585 = ORIENTED_EDGE ( 'NONE', *, *, #33068, .T. ) ;
#86586 = ORIENTED_EDGE ( 'NONE', *, *, #73435, .T. ) ;
#86587 = CARTESIAN_POINT ( 'NONE',  ( 7.899999999999924860, 12.50000000000000000, 3.637306695894644726 ) ) ;
#86588 = CIRCLE ( 'NONE', #17637, 0.1000000000000002554 ) ;
#86589 = VERTEX_POINT ( 'NONE', #114532 ) ;
#86590 = CARTESIAN_POINT ( 'NONE',  ( -1.250000000000035749, 2.500000000000000000, -7.188010851410854052 ) ) ;
#86591 = CARTESIAN_POINT ( 'NONE',  ( 3.749999999999940492, 12.50000000000000000, 2.792790559304612064 ) ) ;
#86592 = AXIS2_PLACEMENT_3D ( 'NONE', #105203, #57406, #24722 ) ;
#86593 = AXIS2_PLACEMENT_3D ( 'NONE', #70429, #80256, #18095 ) ;
#86594 = AXIS2_PLACEMENT_3D ( 'NONE', #111760, #31280, #50916 ) ;
#86595 = VERTEX_POINT ( 'NONE', #75261 ) ;
#86596 = ORIENTED_EDGE ( 'NONE', *, *, #58870, .T. ) ;
#86597 = DIRECTION ( 'NONE',  ( 0.000000000000000000, 0.000000000000000000, -1.000000000000000000 ) ) ;
#86598 = CARTESIAN_POINT ( 'NONE',  ( 1.849999999999950573, 2.500000000000000000, -1.918653347947326004 ) ) ;
#86599 = VERTEX_POINT ( 'NONE', #115162 ) ;
#86600 = FACE_OUTER_BOUND ( 'NONE', #126521, .T. ) ;
#86602 = PLANE ( 'NONE',  #86855 ) ;
#86601 = AXIS2_PLACEMENT_3D ( 'NONE', #36852, #129113, #29592 ) ;
#86603 = VECTOR ( 'NONE', #92810, 1000.000000000000000 ) ;
#86604 = CIRCLE ( 'NONE', #115853, 0.06509327318403745899 ) ;
#86605 = DIRECTION ( 'NONE',  ( 0.000000000000000000, 0.000000000000000000, 1.000000000000000000 ) ) ;
#86606 = CARTESIAN_POINT ( 'NONE',  ( 7.699999999999922018, 2.500000000000000000, 0.2464101615137735679 ) ) ;
#86607 = CARTESIAN_POINT ( 'NONE',  ( 12.94999999999989981, 12.50000000000000000, -2.099970236277064473 ) ) ;
#86608 = FACE_OUTER_BOUND ( 'NONE', #83234, .T. ) ;
#86609 = AXIS2_PLACEMENT_3D ( 'NONE', #7018, #7668, #29273 ) ;
#86610 = AXIS2_PLACEMENT_3D ( 'NONE', #549, #21492, #119681 ) ;
#86612 = EDGE_CURVE ( 'NONE', #59835, #50117, #23583, .T. ) ;
#86611 = CIRCLE ( 'NONE', #113733, 0.06509327318403745899 ) ;
#86613 = VERTEX_POINT ( 'NONE', #34727 ) ;
#86614 = VERTEX_POINT ( 'NONE', #63526 ) ;
#86615 = EDGE_LOOP ( 'NONE', ( #20869, #91390, #37673, #16698 ) ) ;
#86616 = ORIENTED_EDGE ( 'NONE', *, *, #94769, .T. ) ;
#86617 = DIRECTION ( 'NONE',  ( 0.000000000000000000, 0.000000000000000000, -1.000000000000000000 ) ) ;
#86618 = CARTESIAN_POINT ( 'NONE',  ( 11.04999999999990656, 12.50000000000000000, -6.083687093685488989 ) ) ;
#86619 = CONICAL_SURFACE ( 'NONE', #30217, 0.1000000000000002554, 0.003490658503988666988 ) ;
#86620 = FACE_OUTER_BOUND ( 'NONE', #75064, .T. ) ;
#86621 = ORIENTED_EDGE ( 'NONE', *, *, #57183, .T. ) ;
#86622 = EDGE_CURVE ( 'NONE', #95311, #56692, #5863, .T. ) ;
#86623 = FACE_BOUND ( 'NONE', #27507, .T. ) ;
#86624 = ADVANCED_FACE ( 'NONE', ( #15682 ), #104327, .T. ) ;
#86625 = LINE ( 'NONE', #35609, #18634 ) ;
#86626 = DIRECTION ( 'NONE',  ( 0.000000000000000000, 0.000000000000000000, 1.000000000000000000 ) ) ;
#86627 = DIRECTION ( 'NONE',  ( 0.000000000000000000, 0.000000000000000000, -1.000000000000000000 ) ) ;
#86628 = CARTESIAN_POINT ( 'NONE',  ( -10.60000000000000320, 2.500000000000000000, -3.983716857408421852 ) ) ;
#86629 = CARTESIAN_POINT ( 'NONE',  ( 3.749999999999976907, 2.500000000000000000, 2.265063509461097357 ) ) ;
#86630 = EDGE_CURVE ( 'NONE', #85856, #6770, #3942, .T. ) ;
#86631 = DIRECTION ( 'NONE',  ( 0.000000000000000000, 0.000000000000000000, 1.000000000000000000 ) ) ;
#86632 = EDGE_CURVE ( 'NONE', #32010, #54474, #54166, .T. ) ;
#86633 = VERTEX_POINT ( 'NONE', #113915 ) ;
#86634 = DIRECTION ( 'NONE',  ( 0.000000000000000000, 0.000000000000000000, 1.000000000000000000 ) ) ;
#86635 = ADVANCED_FACE ( 'NONE', ( #54337 ), #118995, .T. ) ;
#86636 = DIRECTION ( 'NONE',  ( -0.000000000000000000, -1.000000000000000000, -0.000000000000000000 ) ) ;
#86637 = EDGE_CURVE ( 'NONE', #51195, #13525, #74623, .T. ) ;
#86638 = EDGE_CURVE ( 'NONE', #29908, #32550, #14426, .T. ) ;
#86639 = CIRCLE ( 'NONE', #101320, 0.06509327318403745899 ) ;
#86640 = CARTESIAN_POINT ( 'NONE',  ( -8.550000000000011369, 2.500000000000000000, -2.511473670974877948 ) ) ;
#86641 = ORIENTED_EDGE ( 'NONE', *, *, #93610, .F. ) ;
#86642 = ORIENTED_EDGE ( 'NONE', *, *, #83556, .T. ) ;
#86643 = EDGE_LOOP ( 'NONE', ( #73095, #6235 ) ) ;
#86644 = ORIENTED_EDGE ( 'NONE', *, *, #102482, .T. ) ;
#86645 = CARTESIAN_POINT ( 'NONE',  ( 9.549999999999915445, 12.50000000000000000, 6.495190528383297135 ) ) ;
#86646 = CARTESIAN_POINT ( 'NONE',  ( 14.19999999999989626, 2.500000000000000000, -0.1000000000000022815 ) ) ;
#86648 = VERTEX_POINT ( 'NONE', #19570 ) ;
#86647 = ORIENTED_EDGE ( 'NONE', *, *, #118973, .F. ) ;
#86649 = EDGE_CURVE ( 'NONE', #83282, #96180, #66754, .T. ) ;
#86650 = ORIENTED_EDGE ( 'NONE', *, *, #73753, .F. ) ;
#86651 = DIRECTION ( 'NONE',  ( 0.000000000000000000, 0.000000000000000000, 1.000000000000000000 ) ) ;
#86652 = AXIS2_PLACEMENT_3D ( 'NONE', #33819, #73733, #16092 ) ;
#86653 = AXIS2_PLACEMENT_3D ( 'NONE', #89022, #20271, #41226 ) ;
#86654 = CARTESIAN_POINT ( 'NONE',  ( 10.30524027341030369, -2.500000000000510703, 9.130939513284465292 ) ) ;
#86655 = DIRECTION ( 'NONE',  ( 0.000000000000000000, 1.000000000000000000, 0.000000000000000000 ) ) ;
#86656 = DIRECTION ( 'NONE',  ( 0.000000000000000000, 1.000000000000000000, 0.000000000000000000 ) ) ;
#86657 = DIRECTION ( 'NONE',  ( 0.000000000000000000, 1.000000000000000000, 0.000000000000000000 ) ) ;
#86658 = ORIENTED_EDGE ( 'NONE', *, *, #55364, .F. ) ;
#86659 = EDGE_LOOP ( 'NONE', ( #32450, #45524 ) ) ;
#86660 = CIRCLE ( 'NONE', #26034, 0.06509327318403745899 ) ;
#86661 = ORIENTED_EDGE ( 'NONE', *, *, #17830, .F. ) ;
#86662 = ORIENTED_EDGE ( 'NONE', *, *, #97709, .F. ) ;
#86663 = AXIS2_PLACEMENT_3D ( 'NONE', #68096, #107387, #3 ) ;
#86664 = DIRECTION ( 'NONE',  ( 0.000000000000000000, 1.000000000000000000, 0.000000000000000000 ) ) ;
#86665 = ORIENTED_EDGE ( 'NONE', *, *, #33329, .F. ) ;
#86666 = EDGE_LOOP ( 'NONE', ( #111244, #81725, #77207, #106152 ) ) ;
#86667 = CARTESIAN_POINT ( 'NONE',  ( 4.399999999999939071, 12.50000000000000000, -0.3464101615137782364 ) ) ;
#86669 = AXIS2_PLACEMENT_3D ( 'NONE', #54711, #40593, #101421 ) ;
#86668 = CARTESIAN_POINT ( 'NONE',  ( -3.150000000000029665, 2.500000000000000000, 6.841600689897072485 ) ) ;
#86670 = CARTESIAN_POINT ( 'NONE',  ( -7.050000000000013145, 12.50000000000000000, 2.099970236277060032 ) ) ;
#86671 = CIRCLE ( 'NONE', #30263, 0.09999999999999999167 ) ;
#86672 = DIRECTION ( 'NONE',  ( 0.000000000000000000, -0.000000000000000000, 1.000000000000000000 ) ) ;
#86673 = ADVANCED_FACE ( 'NONE', ( #116467 ), #98761, .T. ) ;
#86675 = CIRCLE ( 'NONE', #15559, 0.1000000000000002554 ) ;
#86674 = FACE_OUTER_BOUND ( 'NONE', #93090, .T. ) ;
#86676 = ADVANCED_FACE ( 'NONE', ( #9100 ), #121052, .T. ) ;
#86677 = VERTEX_POINT ( 'NONE', #26815 ) ;
#86678 = EDGE_CURVE ( 'NONE', #28644, #63269, #49695, .T. ) ;
#86679 = CIRCLE ( 'NONE', #61571, 0.06509327318403745899 ) ;
#86680 = FACE_OUTER_BOUND ( 'NONE', #83797, .T. ) ;
#86681 = ORIENTED_EDGE ( 'NONE', *, *, #927, .F. ) ;
#86683 = EDGE_CURVE ( 'NONE', #34661, #46223, #47750, .T. ) ;
#86682 = CARTESIAN_POINT ( 'NONE',  ( 186.2083333333333428, -4.445597072760145707, -7.699999999999951328 ) ) ;
#86684 = VERTEX_POINT ( 'NONE', #27439 ) ;
#86685 = DIRECTION ( 'NONE',  ( 0.000000000000000000, 1.000000000000000000, 0.000000000000000000 ) ) ;
#86686 = CARTESIAN_POINT ( 'NONE',  ( 10.59999999999991260, 2.500000000000000000, 0.2464101615137735679 ) ) ;
#86687 = ORIENTED_EDGE ( 'NONE', *, *, #93143, .F. ) ;
#86688 = CARTESIAN_POINT ( 'NONE',  ( -6.850000000000013856, 12.50000000000000000, 2.511473670974873507 ) ) ;
#86689 = ADVANCED_FACE ( 'NONE', ( #128252 ), #41662, .T. ) ;
#86690 = CARTESIAN_POINT ( 'NONE',  ( -4.350000000000027178, 2.500000000000000000, -6.841600689897077814 ) ) ;
#86691 = ORIENTED_EDGE ( 'NONE', *, *, #76607, .F. ) ;
#86692 = ADVANCED_FACE ( 'NONE', ( #38592 ), #127327, .T. ) ;
#86693 = EDGE_CURVE ( 'NONE', #90873, #118431, #116835, .T. ) ;
#86694 = EDGE_CURVE ( 'NONE', #92950, #32930, #16566, .T. ) ;
#86695 = VECTOR ( 'NONE', #128902, 1000.000000000000000 ) ;
#86697 = FACE_OUTER_BOUND ( 'NONE', #92760, .T. ) ;
#86696 = VECTOR ( 'NONE', #23931, 1000.000000000000000 ) ;
#86698 = ORIENTED_EDGE ( 'NONE', *, *, #80658, .T. ) ;
#86699 = CONICAL_SURFACE ( 'NONE', #69985, 0.1000000000000002554, 0.003490658503988666988 ) ;
#86700 = VERTEX_POINT ( 'NONE', #47114 ) ;
#86701 = DIRECTION ( 'NONE',  ( 0.000000000000000000, 0.000000000000000000, 1.000000000000000000 ) ) ;
#86702 = CARTESIAN_POINT ( 'NONE',  ( 8.149999999999923972, 12.50000000000000000, -6.776507416713039689 ) ) ;
#86703 = CARTESIAN_POINT ( 'NONE',  ( 184.0260416670080588, -6.551208109652273848, -3.782341765625003571 ) ) ;
#86704 = CARTESIAN_POINT ( 'NONE',  ( 9.349999999999916156, 2.500000000000000000, -2.511473670974877948 ) ) ;
#86705 = EDGE_CURVE ( 'NONE', #125180, #93363, #64616, .T. ) ;
#86706 = CONICAL_SURFACE ( 'NONE', #32453, 0.1000000000000002554, 0.003490658503988666988 ) ;
#86707 = DIRECTION ( 'NONE',  ( 0.000000000000000000, 0.000000000000000000, -1.000000000000000000 ) ) ;
#86708 = VECTOR ( 'NONE', #56833, 1000.000000000000000 ) ;
#86709 = CONICAL_SURFACE ( 'NONE', #36555, 0.09999999999999999167, 0.003490658503988666988 ) ;
#86710 = PLANE ( 'NONE',  #8967 ) ;
#86711 = CIRCLE ( 'NONE', #109708, 0.06509327318403745899 ) ;
#86712 = VERTEX_POINT ( 'NONE', #68020 ) ;
#86713 = AXIS2_PLACEMENT_3D ( 'NONE', #124205, #73804, #33887 ) ;
#86714 = CARTESIAN_POINT ( 'NONE',  ( -13.14999999999999147, 12.50000000000000000, -2.511473670974875727 ) ) ;
#86715 = AXIS2_PLACEMENT_3D ( 'NONE', #76493, #93546, #64722 ) ;
#86716 = ORIENTED_EDGE ( 'NONE', *, *, #127903, .F. ) ;
#86717 = AXIS2_PLACEMENT_3D ( 'NONE', #105861, #16161, #46284 ) ;
#86718 = CARTESIAN_POINT ( 'NONE',  ( -13.29999999999998828, 2.500000000000000000, 4.330127018922196314 ) ) ;
#86720 = ADVANCED_FACE ( 'NONE', ( #119063 ), #123216, .T. ) ;
#86719 = DIRECTION ( 'NONE',  ( -0.000000000000000000, 1.000000000000000000, -0.000000000000000000 ) ) ;
#86721 = DIRECTION ( 'NONE',  ( 0.000000000000000000, 0.000000000000000000, 1.000000000000000000 ) ) ;
#86722 = DIRECTION ( 'NONE',  ( 0.000000000000000000, -0.9999939076577903929, 0.003490651415223739937 ) ) ;
#86723 = CARTESIAN_POINT ( 'NONE',  ( -0.4000000000000404898, 12.50000000000000000, 5.022947341949748790 ) ) ;
#86724 = EDGE_LOOP ( 'NONE', ( #122202, #5692, #70722, #78074 ) ) ;
#86725 = FACE_OUTER_BOUND ( 'NONE', #73058, .T. ) ;
#86726 = CARTESIAN_POINT ( 'NONE',  ( -6.900000000000019007, 2.500000000000000000, -4.083716857408426826 ) ) ;
#86727 = CIRCLE ( 'NONE', #5247, 10.00000000000000000 ) ;
#86728 = ORIENTED_EDGE ( 'NONE', *, *, #65101, .F. ) ;
#86729 = CARTESIAN_POINT ( 'NONE',  ( 3.749999999999940492, 2.500000000000000000, 5.702370205355745014 ) ) ;
#86730 = EDGE_CURVE ( 'NONE', #119380, #15697, #91814, .T. ) ;
#86731 = EDGE_LOOP ( 'NONE', ( #40187, #6769, #58805, #71426 ) ) ;
#86732 = VERTEX_POINT ( 'NONE', #109222 ) ;
#86733 = CARTESIAN_POINT ( 'NONE',  ( -0.8500000000000395017, 2.500000000000000000, 2.165063509461097713 ) ) ;
#86734 = ORIENTED_EDGE ( 'NONE', *, *, #90042, .T. ) ;
#86735 = CARTESIAN_POINT ( 'NONE',  ( 187.5000000000000000, 0.000000000000000000, 0.000000000000000000 ) ) ;
#86736 = CARTESIAN_POINT ( 'NONE',  ( 2.699999999999947331, 2.500000000000000000, -0.3464101615137783474 ) ) ;
#86737 = AXIS2_PLACEMENT_3D ( 'NONE', #103048, #43515, #52037 ) ;
#86738 = DIRECTION ( 'NONE',  ( -0.000000000000000000, 1.000000000000000000, -0.000000000000000000 ) ) ;
#86739 = ORIENTED_EDGE ( 'NONE', *, *, #104212, .F. ) ;
#86740 = FACE_BOUND ( 'NONE', #33204, .T. ) ;
#86742 = ORIENTED_EDGE ( 'NONE', *, *, #129403, .T. ) ;
#86741 = LINE ( 'NONE', #74999, #59945 ) ;
#86743 = CARTESIAN_POINT ( 'NONE',  ( -3.350000000000031619, 2.500000000000000000, -7.188010851410854052 ) ) ;
#86744 = EDGE_CURVE ( 'NONE', #1738, #105627, #10333, .T. ) ;
#86745 = PLANE ( 'NONE',  #13294 ) ;
#86746 = EDGE_LOOP ( 'NONE', ( #68989, #88222 ) ) ;
#86747 = VECTOR ( 'NONE', #17155, 1000.000000000000000 ) ;
#86748 = ORIENTED_EDGE ( 'NONE', *, *, #45929, .T. ) ;
#86749 = VERTEX_POINT ( 'NONE', #57576 ) ;
#86750 = DIRECTION ( 'NONE',  ( -4.274815082592931898E-19, -0.9999939076577903929, -0.003490651415223739937 ) ) ;
#86751 = LINE ( 'NONE', #16700, #26894 ) ;
#86752 = DIRECTION ( 'NONE',  ( 0.000000000000000000, 0.000000000000000000, -1.000000000000000000 ) ) ;
#86753 = FACE_BOUND ( 'NONE', #47525, .T. ) ;
#86754 = ORIENTED_EDGE ( 'NONE', *, *, #112538, .T. ) ;
#86755 = DIRECTION ( 'NONE',  ( 0.000000000000000000, 0.000000000000000000, -1.000000000000000000 ) ) ;
#86756 = DIRECTION ( 'NONE',  ( -0.000000000000000000, -1.000000000000000000, -0.000000000000000000 ) ) ;
#86757 = CARTESIAN_POINT ( 'NONE',  ( -14.99999999999998224, 12.50000000000000000, -0.7579135962115893799 ) ) ;
#86758 = AXIS2_PLACEMENT_3D ( 'NONE', #1620, #81487, #42878 ) ;
#86759 = DIRECTION ( 'NONE',  ( 0.000000000000000000, 1.000000000000000000, 0.000000000000000000 ) ) ;
#86760 = DIRECTION ( 'NONE',  ( 0.000000000000000000, 1.000000000000000000, 0.000000000000000000 ) ) ;
#86761 = PLANE ( 'NONE',  #128633 ) ;
#86762 = FACE_OUTER_BOUND ( 'NONE', #44598, .T. ) ;
#86763 = EDGE_CURVE ( 'NONE', #48547, #6862, #70888, .T. ) ;
#86764 = ORIENTED_EDGE ( 'NONE', *, *, #116502, .T. ) ;
#86765 = EDGE_LOOP ( 'NONE', ( #26628, #51862, #21210, #41850 ) ) ;
#86766 = VERTEX_POINT ( 'NONE', #39243 ) ;
#86767 = EDGE_LOOP ( 'NONE', ( #11435, #46461, #45315, #70380 ) ) ;
#86768 = ORIENTED_EDGE ( 'NONE', *, *, #7625, .T. ) ;
#86769 = DIRECTION ( 'NONE',  ( 0.000000000000000000, 0.000000000000000000, 1.000000000000000000 ) ) ;
#86770 = CARTESIAN_POINT ( 'NONE',  ( -11.84999999999999609, 2.500000000000000000, 2.511473670974873507 ) ) ;
#86771 = ORIENTED_EDGE ( 'NONE', *, *, #100378, .F. ) ;
#86772 = FACE_BOUND ( 'NONE', #50381, .T. ) ;
#86773 = AXIS2_PLACEMENT_3D ( 'NONE', #50446, #93596, #53671 ) ;
#86774 = EDGE_CURVE ( 'NONE', #117651, #84736, #73028, .T. ) ;
#86775 = CARTESIAN_POINT ( 'NONE',  ( 6.899999999999928413, 2.500000000000000000, -3.883716857408426648 ) ) ;
#86776 = AXIS2_PLACEMENT_3D ( 'NONE', #129322, #21933, #91949 ) ;
#86777 = CARTESIAN_POINT ( 'NONE',  ( 1.849999999999949685, 12.50000000000000000, 1.883746621131358934 ) ) ;
#86778 = ADVANCED_FACE ( 'NONE', ( #20859 ), #125257, .T. ) ;
#86779 = CIRCLE ( 'NONE', #124446, 0.06509327318403745899 ) ;
#86780 = DIRECTION ( 'NONE',  ( 0.000000000000000000, 0.000000000000000000, -1.000000000000000000 ) ) ;
#86781 = EDGE_CURVE ( 'NONE', #119766, #30225, #30703, .T. ) ;
#86782 = PLANE ( 'NONE',  #19762 ) ;
#86783 = ADVANCED_FACE ( 'NONE', ( #40523 ), #110525, .T. ) ;
#86784 = CARTESIAN_POINT ( 'NONE',  ( 11.69999999999990514, 2.500000000000000000, -2.276824562219559311E-15 ) ) ;
#86785 = ADVANCED_FACE ( 'NONE', ( #62089 ), #24911, .T. ) ;
#86786 = ORIENTED_EDGE ( 'NONE', *, *, #19997, .F. ) ;
#86787 = DIRECTION ( 'NONE',  ( 0.000000000000000000, 1.000000000000000000, 0.000000000000000000 ) ) ;
#86788 = VERTEX_POINT ( 'NONE', #102629 ) ;
#86789 = AXIS2_PLACEMENT_3D ( 'NONE', #40466, #81019, #90833 ) ;
#86790 = AXIS2_PLACEMENT_3D ( 'NONE', #75411, #34228, #15187 ) ;
#86791 = ORIENTED_EDGE ( 'NONE', *, *, #48209, .F. ) ;
#86792 = ORIENTED_EDGE ( 'NONE', *, *, #110015, .F. ) ;
#86793 = DIRECTION ( 'NONE',  ( 0.000000000000000000, 0.000000000000000000, -1.000000000000000000 ) ) ;
#86794 = AXIS2_PLACEMENT_3D ( 'NONE', #126660, #16669, #97827 ) ;
#86795 = DIRECTION ( 'NONE',  ( -4.274815082592931898E-19, -0.9999939076577903929, -0.003490651415223739937 ) ) ;
#86796 = LINE ( 'NONE', #66506, #795 ) ;
#86797 = ORIENTED_EDGE ( 'NONE', *, *, #5924, .T. ) ;
#86798 = ADVANCED_FACE ( 'NONE', ( #11019 ), #1914, .T. ) ;
#86799 = CARTESIAN_POINT ( 'NONE',  ( 4.599999999999938360, 2.500000000000000000, -2.276824562219559311E-15 ) ) ;
#86800 = ADVANCED_FACE ( 'NONE', ( #12951 ), #26979, .T. ) ;
#86801 = AXIS2_PLACEMENT_3D ( 'NONE', #112878, #52031, #114166 ) ;
#86802 = CARTESIAN_POINT ( 'NONE',  ( 5.399999999999936406, 2.500000000000000000, -5.022947341949754119 ) ) ;
#86803 = EDGE_CURVE ( 'NONE', #75566, #90750, #60445, .T. ) ;
#86804 = DIRECTION ( 'NONE',  ( 0.000000000000000000, 1.000000000000000000, 0.000000000000000000 ) ) ;
#86805 = CARTESIAN_POINT ( 'NONE',  ( 186.6093750003414016, 9.264065473108010111E-16, -7.564683531250000925 ) ) ;
#86806 = DIRECTION ( 'NONE',  ( 0.000000000000000000, 0.000000000000000000, 1.000000000000000000 ) ) ;
#86808 = VECTOR ( 'NONE', #47924, 1000.000000000000000 ) ;
#86807 = DIRECTION ( 'NONE',  ( 0.000000000000000000, 1.000000000000000000, 0.000000000000000000 ) ) ;
#86809 = PRODUCT_RELATED_PRODUCT_CATEGORY ( 'part', '', ( #126727 ) ) ;
#86810 = CARTESIAN_POINT ( 'NONE',  ( -4.400000000000028777, 12.50000000000000000, -4.048810130592463530 ) ) ;
#86811 = ORIENTED_EDGE ( 'NONE', *, *, #116555, .T. ) ;
#86812 = CARTESIAN_POINT ( 'NONE',  ( -12.69999999999999218, 2.500000000000000000, -0.2464101615137741230 ) ) ;
#86813 = ORIENTED_EDGE ( 'NONE', *, *, #39836, .T. ) ;
#86814 = VERTEX_POINT ( 'NONE', #60162 ) ;
#86815 = FACE_OUTER_BOUND ( 'NONE', #113048, .T. ) ;
#86816 = DIRECTION ( 'NONE',  ( -0.000000000000000000, 1.000000000000000000, -0.000000000000000000 ) ) ;
#86817 = DIRECTION ( 'NONE',  ( 0.000000000000000000, 1.000000000000000000, 0.000000000000000000 ) ) ;
#86818 = VECTOR ( 'NONE', #97571, 1000.000000000000000 ) ;
#86819 = ORIENTED_EDGE ( 'NONE', *, *, #67455, .F. ) ;
#86820 = VERTEX_POINT ( 'NONE', #61447 ) ;
#86821 = DIRECTION ( 'NONE',  ( 0.000000000000000000, 0.000000000000000000, -1.000000000000000000 ) ) ;
#86822 = CARTESIAN_POINT ( 'NONE',  ( 48.81598501501260046, 3.619493961087981493, -4.312659849359727460 ) ) ;
#86823 = DIRECTION ( 'NONE',  ( -4.274815082592931898E-19, -0.9999939076577903929, -0.003490651415223739937 ) ) ;
#86824 = ORIENTED_EDGE ( 'NONE', *, *, #63037, .T. ) ;
#86825 = ORIENTED_EDGE ( 'NONE', *, *, #55461, .T. ) ;
#86826 = PLANE ( 'NONE',  #50288 ) ;
#86827 = CIRCLE ( 'NONE', #72185, 7.700000000000000178 ) ;
#86828 = CIRCLE ( 'NONE', #61810, 0.06509327318403745899 ) ;
#86829 = ORIENTED_EDGE ( 'NONE', *, *, #74363, .F. ) ;
#86831 = CIRCLE ( 'NONE', #1154, 0.06509327318403745899 ) ;
#86830 = CARTESIAN_POINT ( 'NONE',  ( 0.000000000000000000, 2.500000000000000000, 0.000000000000000000 ) ) ;
#86832 = DIRECTION ( 'NONE',  ( 0.000000000000000000, -0.000000000000000000, 1.000000000000000000 ) ) ;
#86833 = VERTEX_POINT ( 'NONE', #31341 ) ;
#86834 = CARTESIAN_POINT ( 'NONE',  ( -12.49999999999999289, 12.50000000000000000, 5.022947341949748790 ) ) ;
#86835 = PLANE ( 'NONE',  #12774 ) ;
#86836 = DIRECTION ( 'NONE',  ( -4.274815082592931898E-19, -0.9999939076577903929, -0.003490651415223739937 ) ) ;
#86837 = EDGE_CURVE ( 'NONE', #69080, #103801, #102001, .T. ) ;
#86838 = DIRECTION ( 'NONE',  ( 0.000000000000000000, 1.000000000000000000, 0.000000000000000000 ) ) ;
#86839 = ORIENTED_EDGE ( 'NONE', *, *, #115917, .T. ) ;
#86840 = VECTOR ( 'NONE', #74671, 1000.000000000000000 ) ;
#86841 = EDGE_CURVE ( 'NONE', #63043, #20499, #50981, .T. ) ;
#86842 = DIRECTION ( 'NONE',  ( -0.000000000000000000, -1.000000000000000000, -0.000000000000000000 ) ) ;
#86845 = EDGE_CURVE ( 'NONE', #114315, #23628, #121627, .T. ) ;
#86844 = AXIS2_PLACEMENT_3D ( 'NONE', #102556, #50901, #482 ) ;
#86843 = DIRECTION ( 'NONE',  ( -0.000000000000000000, -1.000000000000000000, -0.000000000000000000 ) ) ;
#86846 = ORIENTED_EDGE ( 'NONE', *, *, #97437, .F. ) ;
#86847 = EDGE_LOOP ( 'NONE', ( #27556, #14732, #57592, #5372 ) ) ;
#86848 = CARTESIAN_POINT ( 'NONE',  ( 184.7968750003414016, 8.734944146203032389, 5.348610694689227483E-16 ) ) ;
#86849 = DIRECTION ( 'NONE',  ( 0.000000000000000000, 1.000000000000000000, 0.000000000000000000 ) ) ;
#86850 = DIRECTION ( 'NONE',  ( 0.000000000000000000, 0.000000000000000000, -1.000000000000000000 ) ) ;
#86851 = CARTESIAN_POINT ( 'NONE',  ( -6.850000000000013856, 2.500000000000000000, 6.248780366869521430 ) ) ;
#86852 = DIRECTION ( 'NONE',  ( 0.000000000000000000, 1.000000000000000000, 0.000000000000000000 ) ) ;
#86853 = EDGE_CURVE ( 'NONE', #57270, #79310, #20711, .T. ) ;
#86854 = CARTESIAN_POINT ( 'NONE',  ( -5.850000000000022737, 2.500000000000000000, -2.265063509461101798 ) ) ;
#86855 = AXIS2_PLACEMENT_3D ( 'NONE', #97076, #116066, #75488 ) ;
#86856 = CARTESIAN_POINT ( 'NONE',  ( 175.5000000000000000, 0.000000000000000000, 2.000000000000000000 ) ) ;
#86857 = DIRECTION ( 'NONE',  ( -0.000000000000000000, 1.000000000000000000, -0.000000000000000000 ) ) ;
#86858 = FACE_OUTER_BOUND ( 'NONE', #100925, .T. ) ;
#86859 = PLANE ( 'NONE',  #98149 ) ;
#86861 = VERTEX_POINT ( 'NONE', #71237 ) ;
#86860 = VECTOR ( 'NONE', #93421, 1000.000000000000000 ) ;
#86862 = DIRECTION ( 'NONE',  ( 0.000000000000000000, 1.000000000000000000, 0.000000000000000000 ) ) ;
#86863 = VERTEX_POINT ( 'NONE', #72553 ) ;
#86864 = DIRECTION ( 'NONE',  ( 0.000000000000000000, 1.000000000000000000, 0.000000000000000000 ) ) ;
#86866 = ADVANCED_FACE ( 'NONE', ( #122298 ), #90887, .T. ) ;
#86865 = CONICAL_SURFACE ( 'NONE', #59715, 0.1000000000000000056, 0.003490658503988666988 ) ;
#86867 = DIRECTION ( 'NONE',  ( -0.000000000000000000, -1.000000000000000000, -0.000000000000000000 ) ) ;
#86868 = CARTESIAN_POINT ( 'NONE',  ( 2.499999999999983569, 2.500000000000000000, -4.230127018922201998 ) ) ;
#86869 = ORIENTED_EDGE ( 'NONE', *, *, #11996, .T. ) ;
#86870 = FACE_OUTER_BOUND ( 'NONE', #85541, .T. ) ;
#86871 = CIRCLE ( 'NONE', #120339, 2.000000000000000000 ) ;
#86872 = CIRCLE ( 'NONE', #99422, 0.06509327318403745899 ) ;
#86873 = DIRECTION ( 'NONE',  ( -0.000000000000000000, 1.000000000000000000, -0.000000000000000000 ) ) ;
#86875 = VERTEX_POINT ( 'NONE', #60786 ) ;
#86874 = CARTESIAN_POINT ( 'NONE',  ( -11.89999999999999503, 12.50000000000000000, 3.983716857408420076 ) ) ;
#86876 =( BOUNDED_SURFACE ( )  B_SPLINE_SURFACE ( 1, 2, ( 
 ( #67917, #107847, #69862, #49591, #39777, #50232, #18170, #60696, #447, #29941, #109785, #117639, #79050, #68558, #58116, #58753, #100591, #98021, #20115, #48941, #60062, #80331, #88851, #120256, #90118, #39142, #99967, #70496, #118953, #29300, #110420, #12210, #90781, #50865, #62628, #23985, #22707, #3058, #101248, #43006, #23316, #43636, #122827, #32533, #53451, #1108, #71797, #92061, #101898, #120883, #63904, #82264, #63254, #103183, #41067, #91428, #82908, #121512, #21392, #13496, #113647, #10901, #111715, #93365, #61332, #102531, #72441, #52152, #33173, #3688, #12837, #52788, #80971, #122188, #42333, #112366, #92722, #73078, #11573, #2375, #22062, #113000, #31236, #51515, #83555 ),
 ( #123453, #33793, #73705, #71137, #111041, #1745, #41703, #81604, #31870, #61980, #34457, #25243, #126027, #6242, #54083, #44915, #46190, #124103, #5599, #44248, #66469, #74366, #14141, #94004, #4305, #86092, #55373, #114283, #95938, #94635, #65821, #65162, #64538, #36393, #35105, #76303, #105098, #84172, #125401, #116209, #26558, #56000, #4962, #106396, #24628, #104464, #14765, #54704, #84821, #15423, #16705, #124755, #25915, #95298, #75015, #115554, #114918, #45564, #75634, #85469, #105763, #16063, #103832, #35731, #74149, #91859, #81403, #123873, #31647, #34244, #2828, #13276, #72860, #2172, #114072, #102324, #63691, #82024, #12635, #102951, #24402, #112144, #112790, #51939, #52566 ) ),
 .UNSPECIFIED., .F., .F., .F. ) 
 B_SPLINE_SURFACE_WITH_KNOTS ( ( 2, 2 ),
 ( 3, 2, 2, 2, 2, 2, 2, 2, 2, 2, 2, 2, 2, 2, 2, 2, 2, 2, 2, 2, 2, 2, 2, 2, 2, 2, 2, 2, 2, 2, 2, 2, 2, 2, 2, 2, 2, 2, 2, 2, 2, 2, 3 ),
 ( 0.000000000000000000, 1.000000000000000000 ),
 ( 0.000000000000000000, 0.02380952380952380820, 0.04761904761904761640, 0.07142857142857142461, 0.09523809523809523281, 0.1190476190476190410, 0.1428571428571428492, 0.1666666666666666574, 0.1904761904761904656, 0.2142857142857142738, 0.2380952380952380820, 0.2619047619047619180, 0.2857142857142856984, 0.3095238095238095344, 0.3333333333333333148, 0.3571428571428571508, 0.3809523809523809312, 0.4047619047619047672, 0.4285714285714285476, 0.4523809523809523836, 0.4761904761904761640, 0.5000000000000000000, 0.5238095238095238360, 0.5476190476190476719, 0.5714285714285713969, 0.5952380952380952328, 0.6190476190476190688, 0.6428571428571429047, 0.6666666666666666297, 0.6904761904761904656, 0.7142857142857143016, 0.7380952380952381375, 0.7619047619047618625, 0.7857142857142856984, 0.8095238095238095344, 0.8333333333333333703, 0.8571428571428570953, 0.8809523809523809312, 0.9047619047619047672, 0.9285714285714286031, 0.9523809523809523281, 0.9761904761904761640, 1.000000000000000000 ),
 .UNSPECIFIED. ) 
 GEOMETRIC_REPRESENTATION_ITEM ( )  RATIONAL_B_SPLINE_SURFACE ( (
 ( 1.000000000000000000, 0.8660254037844387076, 1.000000000000000000, 0.8660254037844387076, 1.000000000000000000, 0.8660254037844387076, 1.000000000000000000, 0.8660254037844387076, 1.000000000000000000, 0.8660254037844387076, 1.000000000000000000, 0.8660254037844387076, 1.000000000000000000, 0.8660254037844387076, 1.000000000000000000, 0.8660254037844387076, 1.000000000000000000, 0.8660254037844387076, 1.000000000000000000, 0.8660254037844387076, 1.000000000000000000, 0.8660254037844387076, 1.000000000000000000, 0.8660254037844387076, 1.000000000000000000, 0.8660254037844387076, 1.000000000000000000, 0.8660254037844387076, 1.000000000000000000, 0.8660254037844387076, 1.000000000000000000, 0.8660254037844387076, 1.000000000000000000, 0.8660254037844387076, 1.000000000000000000, 0.8660254037844387076, 1.000000000000000000, 0.8660254037844387076, 1.000000000000000000, 0.8660254037844387076, 1.000000000000000000, 0.8660254037844387076, 1.000000000000000000, 0.8660254037844387076, 1.000000000000000000, 0.8660254037844387076, 1.000000000000000000, 0.8660254037844387076, 1.000000000000000000, 0.8660254037844387076, 1.000000000000000000, 0.8660254037844387076, 1.000000000000000000, 0.8660254037844387076, 1.000000000000000000, 0.8660254037844387076, 1.000000000000000000, 0.8660254037844387076, 1.000000000000000000, 0.8660254037844387076, 1.000000000000000000, 0.8660254037844387076, 1.000000000000000000, 0.8660254037844387076, 1.000000000000000000, 0.8660254037844387076, 1.000000000000000000, 0.8660254037844387076, 1.000000000000000000, 0.8660254037844387076, 1.000000000000000000, 0.8660254037844387076, 1.000000000000000000, 0.8660254037844387076, 1.000000000000000000, 0.8660254037844387076, 1.000000000000000000, 0.8660254037844387076, 1.000000000000000000, 0.8660254037844387076, 1.000000000000000000, 0.8660254037844387076, 1.000000000000000000, 0.8660254037844387076, 1.000000000000000000),
 ( 1.000000000000000000, 0.8660254037844387076, 1.000000000000000000, 0.8660254037844387076, 1.000000000000000000, 0.8660254037844387076, 1.000000000000000000, 0.8660254037844387076, 1.000000000000000000, 0.8660254037844387076, 1.000000000000000000, 0.8660254037844387076, 1.000000000000000000, 0.8660254037844387076, 1.000000000000000000, 0.8660254037844387076, 1.000000000000000000, 0.8660254037844387076, 1.000000000000000000, 0.8660254037844387076, 1.000000000000000000, 0.8660254037844387076, 1.000000000000000000, 0.8660254037844387076, 1.000000000000000000, 0.8660254037844387076, 1.000000000000000000, 0.8660254037844387076, 1.000000000000000000, 0.8660254037844387076, 1.000000000000000000, 0.8660254037844387076, 1.000000000000000000, 0.8660254037844387076, 1.000000000000000000, 0.8660254037844387076, 1.000000000000000000, 0.8660254037844387076, 1.000000000000000000, 0.8660254037844387076, 1.000000000000000000, 0.8660254037844387076, 1.000000000000000000, 0.8660254037844387076, 1.000000000000000000, 0.8660254037844387076, 1.000000000000000000, 0.8660254037844387076, 1.000000000000000000, 0.8660254037844387076, 1.000000000000000000, 0.8660254037844387076, 1.000000000000000000, 0.8660254037844387076, 1.000000000000000000, 0.8660254037844387076, 1.000000000000000000, 0.8660254037844387076, 1.000000000000000000, 0.8660254037844387076, 1.000000000000000000, 0.8660254037844387076, 1.000000000000000000, 0.8660254037844387076, 1.000000000000000000, 0.8660254037844387076, 1.000000000000000000, 0.8660254037844387076, 1.000000000000000000, 0.8660254037844387076, 1.000000000000000000, 0.8660254037844387076, 1.000000000000000000, 0.8660254037844387076, 1.000000000000000000, 0.8660254037844387076, 1.000000000000000000, 0.8660254037844387076, 1.000000000000000000, 0.8660254037844387076, 1.000000000000000000, 0.8660254037844387076, 1.000000000000000000, 0.8660254037844387076, 1.000000000000000000) ) ) 
 REPRESENTATION_ITEM ( '' )  SURFACE ( )  );
#86877 = ORIENTED_EDGE ( 'NONE', *, *, #117610, .T. ) ;
#86878 = AXIS2_PLACEMENT_3D ( 'NONE', #24389, #64304, #84596 ) ;
#86880 = ORIENTED_EDGE ( 'NONE', *, *, #34956, .F. ) ;
#86879 = EDGE_CURVE ( 'NONE', #94866, #21053, #92167, .T. ) ;
#86881 = ORIENTED_EDGE ( 'NONE', *, *, #61884, .F. ) ;
#86882 = ORIENTED_EDGE ( 'NONE', *, *, #99351, .T. ) ;
#86883 = FACE_OUTER_BOUND ( 'NONE', #82279, .T. ) ;
#86884 = AXIS2_PLACEMENT_3D ( 'NONE', #79498, #923, #110862 ) ;
#86885 = DIRECTION ( 'NONE',  ( -0.05223670945016245515, 0.9986347311133432214, 0.000000000000000000 ) ) ;
#86886 = CARTESIAN_POINT ( 'NONE',  ( -11.64999999999999680, 2.500000000000000000, -6.395190528383298378 ) ) ;
#86887 = CIRCLE ( 'NONE', #128781, 0.1000000000000000056 ) ;
#86888 = DIRECTION ( 'NONE',  ( 0.000000000000000000, 1.000000000000000000, 0.000000000000000000 ) ) ;
#86889 = AXIS2_PLACEMENT_3D ( 'NONE', #10622, #79406, #108196 ) ;
#86890 = VERTEX_POINT ( 'NONE', #2489 ) ;
#86891 = CIRCLE ( 'NONE', #30493, 0.06509327318403745899 ) ;
#86893 = VECTOR ( 'NONE', #123713, 1000.000000000000000 ) ;
#86892 = CARTESIAN_POINT ( 'NONE',  ( 11.64999999999990266, 12.50000000000000000, -6.495190528383302464 ) ) ;
#86894 = EDGE_LOOP ( 'NONE', ( #56976, #23396 ) ) ;
#86895 = CARTESIAN_POINT ( 'NONE',  ( 5.849999999999933920, 2.500000000000000000, 5.802370205355744659 ) ) ;
#86896 = DIRECTION ( 'NONE',  ( -0.000000000000000000, 1.000000000000000000, -0.000000000000000000 ) ) ;
#86897 = LINE ( 'NONE', #86241, #455 ) ;
#86898 = DIRECTION ( 'NONE',  ( 0.000000000000000000, 0.000000000000000000, 1.000000000000000000 ) ) ;
#86899 = ADVANCED_FACE ( 'NONE', ( #101364 ), #66850, .T. ) ;
#86900 = ORIENTED_EDGE ( 'NONE', *, *, #60821, .F. ) ;
#86901 = ORIENTED_EDGE ( 'NONE', *, *, #31260, .T. ) ;
#86902 = EDGE_LOOP ( 'NONE', ( #24147, #51688 ) ) ;
#86903 = ORIENTED_EDGE ( 'NONE', *, *, #60048, .T. ) ;
#86904 = CARTESIAN_POINT ( 'NONE',  ( -4.800000000000024691, 12.50000000000000000, 4.676537180435972552 ) ) ;
#86905 = CARTESIAN_POINT ( 'NONE',  ( 21.24754738303277435, 0.7337760880902381988, 4.182111650399361835 ) ) ;
#86906 = EDGE_CURVE ( 'NONE', #89946, #83439, #68906, .T. ) ;
#86907 = CARTESIAN_POINT ( 'NONE',  ( -6.450000000000017941, 2.500000000000000000, -2.611473670974877592 ) ) ;
#86908 = FACE_BOUND ( 'NONE', #2068, .T. ) ;
#86909 = DIRECTION ( 'NONE',  ( 0.000000000000000000, 0.000000000000000000, 1.000000000000000000 ) ) ;
#86910 = DIRECTION ( 'NONE',  ( 0.000000000000000000, 0.000000000000000000, 1.000000000000000000 ) ) ;
#86911 = DIRECTION ( 'NONE',  ( 0.000000000000000000, 0.000000000000000000, 1.000000000000000000 ) ) ;
#86912 = CARTESIAN_POINT ( 'NONE',  ( -11.89999999999999503, 2.500000000000000000, 3.883716857408420431 ) ) ;
#86913 = CARTESIAN_POINT ( 'NONE',  ( 184.5052083336747444, -6.551208109652278289, 3.782341765624995134 ) ) ;
#86914 = VECTOR ( 'NONE', #99533, 1000.000000000000000 ) ;
#86915 = CARTESIAN_POINT ( 'NONE',  ( 1.899999999999951283, 2.500000000000000000, -0.3464101615137782364 ) ) ;
#86916 = DIRECTION ( 'NONE',  ( -0.000000000000000000, -1.000000000000000000, -0.000000000000000000 ) ) ;
#86917 = CONICAL_SURFACE ( 'NONE', #74411, 0.09999999999999982514, 0.003490658503988666988 ) ;
#86918 = VECTOR ( 'NONE', #11431, 1000.000000000000000 ) ;
#86919 = FACE_OUTER_BOUND ( 'NONE', #51932, .T. ) ;
#86920 = AXIS2_PLACEMENT_3D ( 'NONE', #88357, #47175, #65509 ) ;
#86921 = ADVANCED_FACE ( 'NONE', ( #81078 ), #62732, .T. ) ;
#86922 = ORIENTED_EDGE ( 'NONE', *, *, #115253, .T. ) ;
#86923 = ORIENTED_EDGE ( 'NONE', *, *, #69895, .F. ) ;
#86924 = ORIENTED_EDGE ( 'NONE', *, *, #104781, .T. ) ;
#86925 = ORIENTED_EDGE ( 'NONE', *, *, #111527, .T. ) ;
#86926 = DIRECTION ( 'NONE',  ( 0.000000000000000000, 0.000000000000000000, 1.000000000000000000 ) ) ;
#86927 = FACE_BOUND ( 'NONE', #93350, .T. ) ;
#86928 = FACE_OUTER_BOUND ( 'NONE', #38310, .T. ) ;
#86930 = CARTESIAN_POINT ( 'NONE',  ( 11.69999999999990870, 2.500000000000000000, -4.430127018922202176 ) ) ;
#86929 = CIRCLE ( 'NONE', #24158, 0.1000000000000000472 ) ;
#86931 = EDGE_CURVE ( 'NONE', #120557, #46758, #14246, .T. ) ;
#86933 = CIRCLE ( 'NONE', #30533, 0.1000000000000002554 ) ;
#86932 = AXIS2_PLACEMENT_3D ( 'NONE', #45784, #67305, #17584 ) ;
#86934 = ORIENTED_EDGE ( 'NONE', *, *, #52894, .F. ) ;
#86935 = EDGE_CURVE ( 'NONE', #64023, #781, #112838, .T. ) ;
#86936 = CARTESIAN_POINT ( 'NONE',  ( 10.59999999999991260, 2.500000000000000000, -0.3464101615137783474 ) ) ;
#86937 = ADVANCED_FACE ( 'NONE', ( #125497 ), #84284, .T. ) ;
#86938 = DIRECTION ( 'NONE',  ( -4.274815082592931898E-19, -0.9999939076577903929, -0.003490651415223739937 ) ) ;
#86939 = EDGE_CURVE ( 'NONE', #74400, #27754, #87686, .T. ) ;
#86940 = EDGE_CURVE ( 'NONE', #594, #55743, #119094, .T. ) ;
#86941 = VERTEX_POINT ( 'NONE', #105864 ) ;
#86942 = CARTESIAN_POINT ( 'NONE',  ( 1.449999999999952216, 12.50000000000000000, 1.818653347947321475 ) ) ;
#86943 = CARTESIAN_POINT ( 'NONE',  ( 20.59313469514036399, 2.666874593322338338, -2.243770147468779896 ) ) ;
#86944 = CIRCLE ( 'NONE', #92939, 0.09999999999999982514 ) ;
#86945 = AXIS2_PLACEMENT_3D ( 'NONE', #96285, #125738, #73428 ) ;
#86946 = ADVANCED_FACE ( 'NONE', ( #16167 ), #37533, .T. ) ;
#86947 = EDGE_LOOP ( 'NONE', ( #63803, #63771, #83846, #123647 ) ) ;
#86948 = DIRECTION ( 'NONE',  ( -0.000000000000000000, 1.000000000000000000, -0.000000000000000000 ) ) ;
#86949 = ADVANCED_FACE ( 'NONE', ( #103295 ), #13601, .F. ) ;
#86950 = CARTESIAN_POINT ( 'NONE',  ( 6.249999999999932498, 2.500000000000000000, -2.857883832488653741 ) ) ;
#86951 = EDGE_CURVE ( 'NONE', #64286, #113932, #54817, .T. ) ;
#86952 = VERTEX_POINT ( 'NONE', #124218 ) ;
#86953 = DIRECTION ( 'NONE',  ( 0.000000000000000000, 0.000000000000000000, 1.000000000000000000 ) ) ;
#86954 = EDGE_CURVE ( 'NONE', #21274, #77248, #83597, .T. ) ;
#86955 = FACE_OUTER_BOUND ( 'NONE', #98322, .T. ) ;
#86956 = ORIENTED_EDGE ( 'NONE', *, *, #75664, .T. ) ;
#86957 = CARTESIAN_POINT ( 'NONE',  ( 13.14999999999990088, 12.50000000000000000, 2.576566944158910744 ) ) ;
#86958 = ORIENTED_EDGE ( 'NONE', *, *, #13919, .F. ) ;
#86959 = ORIENTED_EDGE ( 'NONE', *, *, #128714, .T. ) ;
#86960 = DIRECTION ( 'NONE',  ( -0.000000000000000000, 1.000000000000000000, -0.000000000000000000 ) ) ;
#86961 = EDGE_CURVE ( 'NONE', #102321, #125657, #25004, .T. ) ;
#86962 = ORIENTED_EDGE ( 'NONE', *, *, #25058, .F. ) ;
#86963 = DIRECTION ( 'NONE',  ( 0.000000000000000000, 1.000000000000000000, 0.000000000000000000 ) ) ;
#86964 = DIRECTION ( 'NONE',  ( 0.000000000000000000, 0.000000000000000000, -1.000000000000000000 ) ) ;
#86965 = AXIS2_PLACEMENT_3D ( 'NONE', #95030, #54441, #93738 ) ;
#86966 = ORIENTED_EDGE ( 'NONE', *, *, #38854, .F. ) ;
#86967 = CIRCLE ( 'NONE', #76514, 0.06509327318403741736 ) ;
#86968 = DIRECTION ( 'NONE',  ( 0.000000000000000000, 1.000000000000000000, 0.000000000000000000 ) ) ;
#86969 = VERTEX_POINT ( 'NONE', #44359 ) ;
#86970 = CARTESIAN_POINT ( 'NONE',  ( 7.499999999999925393, 2.500000000000000000, 4.922947341949748257 ) ) ;
#86971 = DIRECTION ( 'NONE',  ( 0.000000000000000000, 0.000000000000000000, 1.000000000000000000 ) ) ;
#86972 = DIRECTION ( 'NONE',  ( 0.000000000000000000, 0.000000000000000000, 1.000000000000000000 ) ) ;
#86973 = DIRECTION ( 'NONE',  ( 0.000000000000000000, 0.000000000000000000, 1.000000000000000000 ) ) ;
#86974 = CARTESIAN_POINT ( 'NONE',  ( 12.49999999999990585, 12.50000000000000000, 3.572213422710607489 ) ) ;
#86976 = ORIENTED_EDGE ( 'NONE', *, *, #102788, .F. ) ;
#86975 = CIRCLE ( 'NONE', #103720, 0.06509327318403745899 ) ;
#86977 = ORIENTED_EDGE ( 'NONE', *, *, #44102, .F. ) ;
#86978 = CARTESIAN_POINT ( 'NONE',  ( -9.600000000000006750, 2.500000000000000000, -0.6928203230275542523 ) ) ;
#86979 = CARTESIAN_POINT ( 'NONE',  ( 0.6499999999999566125, 2.500000000000000000, -6.248780366869526759 ) ) ;
#86980 = CARTESIAN_POINT ( 'NONE',  ( -9.600000000000006750, 2.500000000000000000, 0.6928203230275494784 ) ) ;
#86982 = ORIENTED_EDGE ( 'NONE', *, *, #88908, .F. ) ;
#86981 = ORIENTED_EDGE ( 'NONE', *, *, #9692, .T. ) ;
#86983 = VERTEX_POINT ( 'NONE', #53550 ) ;
#86984 = DIRECTION ( 'NONE',  ( 0.000000000000000000, 0.000000000000000000, 1.000000000000000000 ) ) ;
#86985 = VECTOR ( 'NONE', #96350, 1000.000000000000000 ) ;
#86986 = DIRECTION ( 'NONE',  ( 0.000000000000000000, 0.000000000000000000, 1.000000000000000000 ) ) ;
#86987 = CARTESIAN_POINT ( 'NONE',  ( -1.250000000000001554, 2.500000000000000000, 6.495190528383297135 ) ) ;
#86988 = AXIS2_PLACEMENT_3D ( 'NONE', #5992, #7932, #47239 ) ;
#86989 = APPLICATION_PROTOCOL_DEFINITION ( 'draft international standard', 'automotive_design', 1998, #4514 ) ;
#86990 = CARTESIAN_POINT ( 'NONE',  ( -5.850000000000018296, 2.500000000000000000, 1.372243186433545370 ) ) ;
#86991 = CARTESIAN_POINT ( 'NONE',  ( -6.900000000000015454, 12.50000000000000000, 3.983716857408420076 ) ) ;
#86992 = DIRECTION ( 'NONE',  ( 0.000000000000000000, 0.000000000000000000, 1.000000000000000000 ) ) ;
#86993 = DIRECTION ( 'NONE',  ( -0.000000000000000000, -1.000000000000000000, -0.000000000000000000 ) ) ;
#86994 = FACE_OUTER_BOUND ( 'NONE', #90802, .T. ) ;
#86995 = CARTESIAN_POINT ( 'NONE',  ( -5.850000000000021849, 2.500000000000000000, -1.472243186433550122 ) ) ;
#86996 = VERTEX_POINT ( 'NONE', #65280 ) ;
#86997 = EDGE_CURVE ( 'NONE', #124869, #32548, #56387, .T. ) ;
#86998 = ADVANCED_FACE ( 'NONE', ( #43748 ), #47997, .T. ) ;
#86999 = CARTESIAN_POINT ( 'NONE',  ( 6.699999999999930012, 2.500000000000000000, -4.230127018922201998 ) ) ;
#87000 = EDGE_LOOP ( 'NONE', ( #109544, #121824, #75068 ) ) ;
#87001 = ORIENTED_EDGE ( 'NONE', *, *, #39372, .T. ) ;
#87002 = DIRECTION ( 'NONE',  ( 0.000000000000000000, -0.000000000000000000, 1.000000000000000000 ) ) ;
#87003 = DIRECTION ( 'NONE',  ( 0.000000000000000000, 0.000000000000000000, -1.000000000000000000 ) ) ;
#87004 = CONICAL_SURFACE ( 'NONE', #74490, 0.1000000000000002554, 0.003490658503988666988 ) ;
#87005 = LINE ( 'NONE', #37281, #105111 ) ;
#87006 = DIRECTION ( 'NONE',  ( 0.000000000000000000, -0.9999939076577903929, 0.003490651415223739937 ) ) ;
#87008 = DIRECTION ( 'NONE',  ( 0.000000000000000000, 0.000000000000000000, 1.000000000000000000 ) ) ;
#87007 = PRODUCT_DEFINITION_SHAPE ( 'NONE', 'NONE',  #92424 ) ;
#87009 = DIRECTION ( 'NONE',  ( 0.000000000000000000, 1.000000000000000000, 0.000000000000000000 ) ) ;
#87010 = AXIS2_PLACEMENT_3D ( 'NONE', #105693, #56567, #96485 ) ;
#87011 = DIRECTION ( 'NONE',  ( 0.000000000000000000, 1.000000000000000000, 0.000000000000000000 ) ) ;
#87012 = EDGE_LOOP ( 'NONE', ( #96296, #30262 ) ) ;
#87013 = CARTESIAN_POINT ( 'NONE',  ( 9.399999999999918643, 2.500000000000000000, 0.2464101615137736789 ) ) ;
#87014 = AXIS2_PLACEMENT_3D ( 'NONE', #114485, #45117, #35301 ) ;
#87015 = AXIS2_PLACEMENT_3D ( 'NONE', #9673, #11602, #31899 ) ;
#87016 = CIRCLE ( 'NONE', #128908, 0.09999999999999982514 ) ;
#87017 = CARTESIAN_POINT ( 'NONE',  ( -11.44999999999999751, 12.50000000000000000, -2.511473670974873951 ) ) ;
#87018 = ORIENTED_EDGE ( 'NONE', *, *, #29432, .F. ) ;
#87019 = AXIS2_PLACEMENT_3D ( 'NONE', #46357, #5147, #115084 ) ;
#87020 = VERTEX_POINT ( 'NONE', #123552 ) ;
#87021 = VERTEX_POINT ( 'NONE', #85575 ) ;
#87022 = ORIENTED_EDGE ( 'NONE', *, *, #123175, .F. ) ;
#87023 = CARTESIAN_POINT ( 'NONE',  ( -4.293440603042597559E-14, 2.500000000000000000, 5.122947341949749323 ) ) ;
#87024 = CARTESIAN_POINT ( 'NONE',  ( -5.600000000000020073, 2.500000000000000000, -0.3464101615137782364 ) ) ;
#87025 = CONICAL_SURFACE ( 'NONE', #24341, 0.1000000000000002554, 0.003490658503988666988 ) ;
#87026 = ORIENTED_EDGE ( 'NONE', *, *, #37970, .T. ) ;
#87027 = DIRECTION ( 'NONE',  ( 0.000000000000000000, 0.000000000000000000, -1.000000000000000000 ) ) ;
#87028 = LINE ( 'NONE', #106667, #8950 ) ;
#87030 = CONICAL_SURFACE ( 'NONE', #122551, 0.1000000000000002554, 0.003490658503988666988 ) ;
#87029 = CIRCLE ( 'NONE', #45280, 0.09999999999999982514 ) ;
#87031 = CARTESIAN_POINT ( 'NONE',  ( 0.5999999999999612310, 2.500000000000000000, -0.3464101615137760715 ) ) ;
#87032 = ORIENTED_EDGE ( 'NONE', *, *, #115766, .F. ) ;
#87033 = LINE ( 'NONE', #88307, #5566 ) ;
#87034 = CARTESIAN_POINT ( 'NONE',  ( 1.049999999999952971, 2.500000000000000000, 6.048780366869521252 ) ) ;
#87035 = EDGE_CURVE ( 'NONE', #120902, #515, #79389, .T. ) ;
#87036 = ORIENTED_EDGE ( 'NONE', *, *, #24549, .T. ) ;
#87037 = VERTEX_POINT ( 'NONE', #113761 ) ;
#87038 = ORIENTED_EDGE ( 'NONE', *, *, #95360, .F. ) ;
#87039 = FACE_OUTER_BOUND ( 'NONE', #26640, .T. ) ;
#87040 = PLANE ( 'NONE',  #46053 ) ;
#87042 = EDGE_LOOP ( 'NONE', ( #114745, #63065 ) ) ;
#87041 = ADVANCED_FACE ( 'NONE', ( #114383 ), #4066, .T. ) ;
#87043 = DIRECTION ( 'NONE',  ( -0.000000000000000000, -1.000000000000000000, -0.000000000000000000 ) ) ;
#87044 = FACE_OUTER_BOUND ( 'NONE', #31910, .T. ) ;
#87045 = CARTESIAN_POINT ( 'NONE',  ( 5.399999999999932854, 2.500000000000000000, 3.637306695894644726 ) ) ;
#87046 = CARTESIAN_POINT ( 'NONE',  ( 11.04999999999990834, 12.50000000000000000, 1.753560074763284016 ) ) ;
#87047 = ADVANCED_FACE ( 'NONE', ( #45023 ), #43803, .T. ) ;
#87048 = ORIENTED_EDGE ( 'NONE', *, *, #6333, .F. ) ;
#87049 = CIRCLE ( 'NONE', #72499, 0.06509327318403745899 ) ;
#87050 = DIRECTION ( 'NONE',  ( 0.000000000000000000, 0.000000000000000000, 1.000000000000000000 ) ) ;
#87051 = CIRCLE ( 'NONE', #20164, 0.06509327318403745899 ) ;
#87052 = ORIENTED_EDGE ( 'NONE', *, *, #79697, .F. ) ;
#87053 = EDGE_LOOP ( 'NONE', ( #6497, #23342, #10353, #89310 ) ) ;
#87054 = ORIENTED_EDGE ( 'NONE', *, *, #303, .F. ) ;
#87055 = EDGE_CURVE ( 'NONE', #113182, #111375, #116924, .T. ) ;
#87056 = FACE_OUTER_BOUND ( 'NONE', #76118, .T. ) ;
#87057 = FACE_BOUND ( 'NONE', #121916, .T. ) ;
#87058 = CARTESIAN_POINT ( 'NONE',  ( 8.099999999999921485, 2.500000000000000000, -0.3464101615137783474 ) ) ;
#87059 = CARTESIAN_POINT ( 'NONE',  ( -8.350000000000013856, 2.500000000000000000, -6.595190528383296780 ) ) ;
#87061 = CONICAL_SURFACE ( 'NONE', #91276, 0.09999999999999982514, 0.003490658503988666988 ) ;
#87060 = AXIS2_PLACEMENT_3D ( 'NONE', #50499, #59047, #90412 ) ;
#87062 = DIRECTION ( 'NONE',  ( 0.000000000000000000, 0.000000000000000000, -1.000000000000000000 ) ) ;
#87063 = ORIENTED_EDGE ( 'NONE', *, *, #102019, .F. ) ;
#87064 = LINE ( 'NONE', #127011, #361 ) ;
#87065 = CARTESIAN_POINT ( 'NONE',  ( -12.89999999999999325, 2.500000000000000000, -3.637306695894647390 ) ) ;
#87066 = CARTESIAN_POINT ( 'NONE',  ( 1.449999999999951772, 2.500000000000000000, -6.148780366869526226 ) ) ;
#87067 = DIRECTION ( 'NONE',  ( 0.000000000000000000, 0.000000000000000000, 1.000000000000000000 ) ) ;
#87068 = VERTEX_POINT ( 'NONE', #27945 ) ;
#87069 = CIRCLE ( 'NONE', #124834, 0.1000000000000002554 ) ;
#87070 = DIRECTION ( 'NONE',  ( -4.274815082592931898E-19, -0.9999939076577903929, -0.003490651415223739937 ) ) ;
#87071 = AXIS2_PLACEMENT_3D ( 'NONE', #32769, #41930, #73298 ) ;
#87072 = CARTESIAN_POINT ( 'NONE',  ( 87.50000000000001421, 0.000000000000000000, 0.000000000000000000 ) ) ;
#87073 = EDGE_LOOP ( 'NONE', ( #41059, #36482 ) ) ;
#87074 = CARTESIAN_POINT ( 'NONE',  ( 3.949999999999940670, 2.500000000000000000, 1.918653347947321564 ) ) ;
#87075 = LINE ( 'NONE', #77899, #69393 ) ;
#87076 = FACE_BOUND ( 'NONE', #10637, .T. ) ;
#87077 = CARTESIAN_POINT ( 'NONE',  ( -10.65000000000000391, 2.500000000000000000, -6.841600689897075149 ) ) ;
#87078 = EDGE_CURVE ( 'NONE', #118132, #112463, #6992, .T. ) ;
#87079 = ORIENTED_EDGE ( 'NONE', *, *, #93483, .F. ) ;
#87080 = CARTESIAN_POINT ( 'NONE',  ( -4.150000000000025224, 2.500000000000000000, 5.902370205355745192 ) ) ;
#87081 = EDGE_LOOP ( 'NONE', ( #96578, #102388 ) ) ;
#87082 = EDGE_LOOP ( 'NONE', ( #25473, #17811, #108064, #114366 ) ) ;
#87083 = CARTESIAN_POINT ( 'NONE',  ( 16.55874544816229488, 0.4845305829427787869, -6.091953208798931207 ) ) ;
#87084 = ADVANCED_FACE ( 'NONE', ( #97331 ), #16660, .T. ) ;
#87085 = CARTESIAN_POINT ( 'NONE',  ( 186.5000000000000000, 0.000000000000000000, 7.700000000000000178 ) ) ;
#87086 = VECTOR ( 'NONE', #124152, 1000.000000000000000 ) ;
#87087 = ADVANCED_FACE ( 'NONE', ( #128088 ), #86202, .T. ) ;
#87088 = ORIENTED_EDGE ( 'NONE', *, *, #8614, .T. ) ;
#87089 = CARTESIAN_POINT ( 'NONE',  ( -5.850000000000021849, 2.500000000000000000, -7.188010851410854052 ) ) ;
#87090 = AXIS2_PLACEMENT_3D ( 'NONE', #94518, #15945, #104969 ) ;
#87091 = CARTESIAN_POINT ( 'NONE',  ( -10.84999999999999964, 2.500000000000000000, 1.372243186433545370 ) ) ;
#87092 = CONICAL_SURFACE ( 'NONE', #116335, 0.1000000000000002554, 0.003490658503988666988 ) ;
#87093 = EDGE_CURVE ( 'NONE', #76525, #79082, #7646, .T. ) ;
#87094 = ADVANCED_FACE ( 'NONE', ( #47599 ), #86859, .T. ) ;
#87095 = DIRECTION ( 'NONE',  ( 0.000000000000000000, -0.000000000000000000, 1.000000000000000000 ) ) ;
#87096 = ADVANCED_FACE ( 'NONE', ( #77050 ), #6200, .T. ) ;
#87097 = CONICAL_SURFACE ( 'NONE', #62087, 0.09999999999999982514, 0.003490658503988666988 ) ;
#87098 = VECTOR ( 'NONE', #104790, 1000.000000000000000 ) ;
#87099 = ORIENTED_EDGE ( 'NONE', *, *, #39111, .F. ) ;
#87100 = CIRCLE ( 'NONE', #30706, 0.1000000000000000472 ) ;
#87101 = DIRECTION ( 'NONE',  ( 0.000000000000000000, -0.000000000000000000, 1.000000000000000000 ) ) ;
#87102 = ADVANCED_FACE ( 'NONE', ( #68508 ), #58468, .T. ) ;
#87103 = CARTESIAN_POINT ( 'NONE',  ( -11.05000000000000071, 2.500000000000000000, -6.941600689897075682 ) ) ;
#87104 = CARTESIAN_POINT ( 'NONE',  ( -5.800000000000018474, 12.50000000000000000, 0.06509327318403515528 ) ) ;
#87105 = CARTESIAN_POINT ( 'NONE',  ( 3.349999999999941913, 2.500000000000000000, 6.495190528383297135 ) ) ;
#87106 = VERTEX_POINT ( 'NONE', #96666 ) ;
#87107 = DIRECTION ( 'NONE',  ( 0.000000000000000000, 0.000000000000000000, -1.000000000000000000 ) ) ;
#87108 = EDGE_LOOP ( 'NONE', ( #9299, #125558, #16192, #1346 ) ) ;
#87109 = AXIS2_PLACEMENT_3D ( 'NONE', #51733, #41278, #81192 ) ;
#87110 = CARTESIAN_POINT ( 'NONE',  ( 7.949999999999925571, 12.50000000000000000, -6.560283801567339701 ) ) ;
#87111 = DIRECTION ( 'NONE',  ( 0.000000000000000000, 0.000000000000000000, 1.000000000000000000 ) ) ;
#87112 = EDGE_CURVE ( 'NONE', #121932, #54992, #118256, .T. ) ;
#87113 = CIRCLE ( 'NONE', #97578, 0.06509327318403745899 ) ;
#87114 = ORIENTED_EDGE ( 'NONE', *, *, #118281, .T. ) ;
#87115 = DIRECTION ( 'NONE',  ( 0.000000000000000000, 0.000000000000000000, 1.000000000000000000 ) ) ;
#87116 = DIRECTION ( 'NONE',  ( -0.000000000000000000, -1.000000000000000000, -0.000000000000000000 ) ) ;
#87117 = DIRECTION ( 'NONE',  ( 0.000000000000000000, 1.000000000000000000, 0.000000000000000000 ) ) ;
#87118 = VECTOR ( 'NONE', #95500, 1000.000000000000000 ) ;
#87119 = LINE ( 'NONE', #46544, #119733 ) ;
#87120 = ORIENTED_EDGE ( 'NONE', *, *, #106115, .F. ) ;
#87121 = DIRECTION ( 'NONE',  ( -0.000000000000000000, 1.000000000000000000, -0.000000000000000000 ) ) ;
#87122 = DIRECTION ( 'NONE',  ( 0.000000000000000000, 0.000000000000000000, 1.000000000000000000 ) ) ;
#87123 = DIRECTION ( 'NONE',  ( 0.000000000000000000, -0.000000000000000000, 1.000000000000000000 ) ) ;
#87124 = CARTESIAN_POINT ( 'NONE',  ( 7.099999999999928590, 2.500000000000000000, -4.430127018922202176 ) ) ;
#87125 = DIRECTION ( 'NONE',  ( 0.000000000000000000, 0.000000000000000000, 1.000000000000000000 ) ) ;
#87126 = EDGE_LOOP ( 'NONE', ( #58130, #61020 ) ) ;
#87127 = ORIENTED_EDGE ( 'NONE', *, *, #100776, .F. ) ;
#87128 = LINE ( 'NONE', #55740, #9435 ) ;
#87129 = ORIENTED_EDGE ( 'NONE', *, *, #68620, .F. ) ;
#87130 = FACE_OUTER_BOUND ( 'NONE', #19963, .T. ) ;
#87132 = EDGE_LOOP ( 'NONE', ( #105689, #89667 ) ) ;
#87131 = EDGE_LOOP ( 'NONE', ( #48096, #49625, #27265, #50150 ) ) ;
#87133 = VERTEX_POINT ( 'NONE', #116308 ) ;
#87134 = VECTOR ( 'NONE', #94690, 1000.000000000000000 ) ;
#87135 = DIRECTION ( 'NONE',  ( -0.000000000000000000, -1.000000000000000000, -0.000000000000000000 ) ) ;
#87136 = FACE_OUTER_BOUND ( 'NONE', #34823, .T. ) ;
#87137 = DIRECTION ( 'NONE',  ( -0.000000000000000000, 1.000000000000000000, -0.000000000000000000 ) ) ;
#87138 = CARTESIAN_POINT ( 'NONE',  ( -1.250000000000035749, 12.50000000000000000, -2.857883832488653741 ) ) ;
#87139 = CARTESIAN_POINT ( 'NONE',  ( -2.100000000000034728, 2.500000000000000000, 4.430127018922196847 ) ) ;
#87140 = CARTESIAN_POINT ( 'NONE',  ( -14.19999999999998685, 2.500000000000000000, 0.09999999999999989453 ) ) ;
#87141 = EDGE_LOOP ( 'NONE', ( #3350, #45635 ) ) ;
#87142 = CARTESIAN_POINT ( 'NONE',  ( -4.150000000000024336, 12.50000000000000000, -2.922977105672691422 ) ) ;
#87143 = VERTEX_POINT ( 'NONE', #46958 ) ;
#87145 = ORIENTED_EDGE ( 'NONE', *, *, #52833, .F. ) ;
#87144 = AXIS2_PLACEMENT_3D ( 'NONE', #47710, #78471, #118364 ) ;
#87146 = ORIENTED_EDGE ( 'NONE', *, *, #34177, .T. ) ;
#87147 = ADVANCED_FACE ( 'NONE', ( #108430 ), #35481, .T. ) ;
#87148 = VERTEX_POINT ( 'NONE', #8934 ) ;
#87149 = AXIS2_PLACEMENT_3D ( 'NONE', #117436, #3180, #76904 ) ;
#87150 = DIRECTION ( 'NONE',  ( 0.000000000000000000, 0.000000000000000000, 1.000000000000000000 ) ) ;
#87151 = ORIENTED_EDGE ( 'NONE', *, *, #109463, .T. ) ;
#87152 = ORIENTED_EDGE ( 'NONE', *, *, #59197, .T. ) ;
#87153 = AXIS2_PLACEMENT_3D ( 'NONE', #111162, #12962, #82391 ) ;
#87154 = EDGE_CURVE ( 'NONE', #110307, #93392, #100314, .T. ) ;
#87155 = CARTESIAN_POINT ( 'NONE',  ( 11.84999999999990727, 12.50000000000000000, -1.883746621131363597 ) ) ;
#87156 = LINE ( 'NONE', #127731, #123163 ) ;
#87157 = CARTESIAN_POINT ( 'NONE',  ( 0.8499999999999557909, 2.500000000000000000, -6.595190528383302109 ) ) ;
#87158 = DIRECTION ( 'NONE',  ( -4.274815082592931898E-19, -0.9999939076577903929, -0.003490651415223739937 ) ) ;
#87159 = DIRECTION ( 'NONE',  ( 0.000000000000000000, 1.000000000000000000, 0.000000000000000000 ) ) ;
#87160 = VERTEX_POINT ( 'NONE', #57413 ) ;
#87161 = DIRECTION ( 'NONE',  ( 0.000000000000000000, 1.000000000000000000, 0.000000000000000000 ) ) ;
#87162 = AXIS2_PLACEMENT_3D ( 'NONE', #97976, #28609, #128760 ) ;
#87163 = ORIENTED_EDGE ( 'NONE', *, *, #128667, .T. ) ;
#87164 = DIRECTION ( 'NONE',  ( 0.000000000000000000, 0.000000000000000000, 1.000000000000000000 ) ) ;
#87165 = CIRCLE ( 'NONE', #126890, 0.1000000000000002554 ) ;
#87166 = ORIENTED_EDGE ( 'NONE', *, *, #80341, .F. ) ;
#87167 = FACE_OUTER_BOUND ( 'NONE', #53463, .T. ) ;
#87168 = ORIENTED_EDGE ( 'NONE', *, *, #103485, .T. ) ;
#87169 = VERTEX_POINT ( 'NONE', #6339 ) ;
#87170 = CARTESIAN_POINT ( 'NONE',  ( 6.849999999999929479, 12.50000000000000000, -1.753560074763288679 ) ) ;
#87171 = DIRECTION ( 'NONE',  ( -4.274815082592931898E-19, -0.9999939076577903929, -0.003490651415223739937 ) ) ;
#87172 = DIRECTION ( 'NONE',  ( 0.000000000000000000, 0.000000000000000000, 1.000000000000000000 ) ) ;
#87173 = DIRECTION ( 'NONE',  ( 0.000000000000000000, 0.000000000000000000, 1.000000000000000000 ) ) ;
#87174 = DIRECTION ( 'NONE',  ( -4.274815082592931898E-19, -0.9999939076577903929, -0.003490651415223739937 ) ) ;
#87175 = ORIENTED_EDGE ( 'NONE', *, *, #93804, .F. ) ;
#87176 = CARTESIAN_POINT ( 'NONE',  ( 11.89999999999990443, 2.500000000000000000, 0.3464101615137736845 ) ) ;
#87177 = CARTESIAN_POINT ( 'NONE',  ( -10.60000000000000142, 2.500000000000000000, -0.3464101615137782364 ) ) ;
#87178 = DIRECTION ( 'NONE',  ( 0.000000000000000000, 0.000000000000000000, -1.000000000000000000 ) ) ;
#87179 = CARTESIAN_POINT ( 'NONE',  ( 13.94999999999989626, 2.500000000000000000, 2.511473670974873507 ) ) ;
#87180 = CIRCLE ( 'NONE', #105974, 5.000000000000000000 ) ;
#87181 = CONICAL_SURFACE ( 'NONE', #70468, 0.09999999999999999167, 0.003490658503988666988 ) ;
#87182 = CARTESIAN_POINT ( 'NONE',  ( -2.700000000000029932, 12.50000000000000000, -4.676537180435977881 ) ) ;
#87183 = EDGE_CURVE ( 'NONE', #45516, #87698, #91905, .T. ) ;
#87184 = ORIENTED_EDGE ( 'NONE', *, *, #114862, .T. ) ;
#87185 = CIRCLE ( 'NONE', #78813, 0.1000000000000002554 ) ;
#87186 = ORIENTED_EDGE ( 'NONE', *, *, #62556, .T. ) ;
#87187 = CARTESIAN_POINT ( 'NONE',  ( 3.099999999999944134, 12.50000000000000000, 4.676537180435972552 ) ) ;
#87188 = CIRCLE ( 'NONE', #103934, 0.1000000000000002554 ) ;
#87189 = EDGE_LOOP ( 'NONE', ( #56148, #107283, #102596, #109446 ) ) ;
#87190 = CIRCLE ( 'NONE', #7775, 0.06509327318403745899 ) ;
#87191 = CARTESIAN_POINT ( 'NONE',  ( -8.750000000000005329, 2.500000000000000000, 5.902370205355745192 ) ) ;
#87193 = ADVANCED_FACE ( 'NONE', ( #48233 ), #102376, .T. ) ;
#87192 = CARTESIAN_POINT ( 'NONE',  ( -4.600000000000024514, 12.50000000000000000, 3.702399969078682407 ) ) ;
#87194 = CIRCLE ( 'NONE', #16170, 0.1000000000000000056 ) ;
#87196 = ORIENTED_EDGE ( 'NONE', *, *, #19233, .F. ) ;
#87195 = ADVANCED_FACE ( 'NONE', ( #124640 ), #89930, .T. ) ;
#87197 = CARTESIAN_POINT ( 'NONE',  ( 185.0416666666666856, -4.445597072760122614, 7.699999999999998401 ) ) ;
#87199 = AXIS2_PLACEMENT_3D ( 'NONE', #7766, #37881, #117703 ) ;
#87198 = DIRECTION ( 'NONE',  ( 0.000000000000000000, 0.000000000000000000, 1.000000000000000000 ) ) ;
#87200 = DIRECTION ( 'NONE',  ( 0.000000000000000000, -0.000000000000000000, 1.000000000000000000 ) ) ;
#87201 = EDGE_CURVE ( 'NONE', #47551, #25742, #73220, .T. ) ;
#87202 = DIRECTION ( 'NONE',  ( 0.000000000000000000, 1.000000000000000000, 0.000000000000000000 ) ) ;
#87203 = ORIENTED_EDGE ( 'NONE', *, *, #101293, .F. ) ;
#87205 = VECTOR ( 'NONE', #106442, 1000.000000000000000 ) ;
#87204 = AXIS2_PLACEMENT_3D ( 'NONE', #96474, #84742, #64451 ) ;
#87206 = DIRECTION ( 'NONE',  ( -4.274815082592931898E-19, -0.9999939076577903929, -0.003490651415223739937 ) ) ;
#87207 = PLANE ( 'NONE',  #125030 ) ;
#87208 = ADVANCED_FACE ( 'NONE', ( #33680 ), #66350, .T. ) ;
#87209 = ORIENTED_EDGE ( 'NONE', *, *, #33082, .T. ) ;
#87210 = EDGE_CURVE ( 'NONE', #64313, #37202, #87774, .T. ) ;
#87211 = FACE_BOUND ( 'NONE', #126452, .T. ) ;
#87212 = CARTESIAN_POINT ( 'NONE',  ( 108.0000000000000142, 8.500000000000000000, 5.000000000000004441 ) ) ;
#87213 = FACE_OUTER_BOUND ( 'NONE', #13331, .T. ) ;
#87214 = ORIENTED_EDGE ( 'NONE', *, *, #121501, .F. ) ;
#87215 = CARTESIAN_POINT ( 'NONE',  ( 4.599999999999936584, 2.500000000000000000, 4.330127018922196314 ) ) ;
#87216 = VERTEX_POINT ( 'NONE', #84707 ) ;
#87217 = CARTESIAN_POINT ( 'NONE',  ( 13.74999999999993427, 12.50000000000000000, 2.230156782645134950 ) ) ;
#87218 = CARTESIAN_POINT ( 'NONE',  ( 4.999999999999971578, 12.50000000000000000, 0.06509327318403515528 ) ) ;
#87219 = CIRCLE ( 'NONE', #108152, 0.1000000000000002554 ) ;
#87220 = FACE_OUTER_BOUND ( 'NONE', #25414, .T. ) ;
#87221 = VERTEX_POINT ( 'NONE', #16595 ) ;
#87222 = DIRECTION ( 'NONE',  ( 0.000000000000000000, 1.000000000000000000, 0.000000000000000000 ) ) ;
#87223 = DIRECTION ( 'NONE',  ( 0.000000000000000000, 0.000000000000000000, -1.000000000000000000 ) ) ;
#87224 = EDGE_LOOP ( 'NONE', ( #89890, #96845, #120056, #59454 ) ) ;
#87225 = DIRECTION ( 'NONE',  ( 0.000000000000000000, -0.000000000000000000, 1.000000000000000000 ) ) ;
#87226 = ORIENTED_EDGE ( 'NONE', *, *, #13062, .T. ) ;
#87227 = DIRECTION ( 'NONE',  ( 0.000000000000000000, -0.000000000000000000, 1.000000000000000000 ) ) ;
#87228 = ADVANCED_FACE ( 'NONE', ( #34991 ), #66931, .T. ) ;
#87229 = VERTEX_POINT ( 'NONE', #96444 ) ;
#87230 = CARTESIAN_POINT ( 'NONE',  ( 6.899999999999928413, 2.500000000000000000, 3.983716857408420964 ) ) ;
#87231 = DIRECTION ( 'NONE',  ( 0.000000000000000000, 0.000000000000000000, 1.000000000000000000 ) ) ;
#87232 = VERTEX_POINT ( 'NONE', #65709 ) ;
#87233 = EDGE_LOOP ( 'NONE', ( #113571, #77392 ) ) ;
#87234 = DIRECTION ( 'NONE',  ( -4.274815082592931898E-19, -0.9999939076577903929, -0.003490651415223739937 ) ) ;
#87235 = DIRECTION ( 'NONE',  ( -0.000000000000000000, 1.000000000000000000, -0.000000000000000000 ) ) ;
#87236 = ORIENTED_EDGE ( 'NONE', *, *, #22675, .F. ) ;
#87238 = EDGE_CURVE ( 'NONE', #82307, #98236, #6757, .T. ) ;
#87237 = AXIS2_PLACEMENT_3D ( 'NONE', #51638, #73841, #121643 ) ;
#87239 = CARTESIAN_POINT ( 'NONE',  ( -2.100000000000033396, 2.500000000000000000, 0.5928203230275495006 ) ) ;
#87240 = DIRECTION ( 'NONE',  ( 0.000000000000000000, -0.9999939076577903929, 0.003490651415223739937 ) ) ;
#87241 = CONICAL_SURFACE ( 'NONE', #32989, 0.1000000000000002554, 0.003490658503988666988 ) ;
#87242 = CARTESIAN_POINT ( 'NONE',  ( -3.950000000000028155, 2.500000000000000000, -6.941600689897077459 ) ) ;
#87243 = DIRECTION ( 'NONE',  ( 0.000000000000000000, 1.000000000000000000, 0.000000000000000000 ) ) ;
#87244 = EDGE_CURVE ( 'NONE', #35273, #37478, #44799, .T. ) ;
#87245 = DIRECTION ( 'NONE',  ( 0.000000000000000000, 0.000000000000000000, -1.000000000000000000 ) ) ;
#87246 = DIRECTION ( 'NONE',  ( 0.000000000000000000, -0.000000000000000000, 1.000000000000000000 ) ) ;
#87247 = EDGE_CURVE ( 'NONE', #121877, #55444, #117008, .T. ) ;
#87250 = ADVANCED_FACE ( 'NONE', ( #14660 ), #114961, .T. ) ;
#87249 = CIRCLE ( 'NONE', #66327, 0.06509327318403745899 ) ;
#87248 = AXIS2_PLACEMENT_3D ( 'NONE', #21198, #91878, #109591 ) ;
#87251 = VERTEX_POINT ( 'NONE', #123347 ) ;
#87252 = EDGE_LOOP ( 'NONE', ( #43568, #58213 ) ) ;
#87254 = ORIENTED_EDGE ( 'NONE', *, *, #66899, .T. ) ;
#87253 = EDGE_CURVE ( 'NONE', #104830, #121148, #73585, .T. ) ;
#87255 = VERTEX_POINT ( 'NONE', #103717 ) ;
#87256 = PLANE ( 'NONE',  #83078 ) ;
#87257 = DIRECTION ( 'NONE',  ( 0.000000000000000000, 0.000000000000000000, 1.000000000000000000 ) ) ;
#87258 = CARTESIAN_POINT ( 'NONE',  ( 13.74999999999989342, 12.50000000000000000, -1.537336459617587581 ) ) ;
#87259 = ORIENTED_EDGE ( 'NONE', *, *, #5064, .T. ) ;
#87260 = FACE_BOUND ( 'NONE', #5002, .T. ) ;
#87261 = CARTESIAN_POINT ( 'NONE',  ( 9.399999999999918643, 12.50000000000000000, -0.3464101615137782364 ) ) ;
#87262 = PLANE ( 'NONE',  #91877 ) ;
#87263 = ADVANCED_FACE ( 'NONE', ( #76185 ), #75264, .T. ) ;
#87264 = DIRECTION ( 'NONE',  ( 0.000000000000000000, 1.000000000000000000, 0.000000000000000000 ) ) ;
#87265 = AXIS2_PLACEMENT_3D ( 'NONE', #15296, #34986, #114172 ) ;
#87266 = EDGE_CURVE ( 'NONE', #27091, #50160, #23871, .T. ) ;
#87267 = DIRECTION ( 'NONE',  ( 0.000000000000000000, 0.000000000000000000, -1.000000000000000000 ) ) ;
#87268 = DIRECTION ( 'NONE',  ( -0.000000000000000000, 1.000000000000000000, -0.000000000000000000 ) ) ;
#87269 = AXIS2_PLACEMENT_3D ( 'NONE', #93263, #23214, #31768 ) ;
#87270 = DIRECTION ( 'NONE',  ( 0.000000000000000000, 0.000000000000000000, -1.000000000000000000 ) ) ;
#87271 = DIRECTION ( 'NONE',  ( -4.274815082592931898E-19, -0.9999939076577903929, -0.003490651415223739937 ) ) ;
#87272 = DIRECTION ( 'NONE',  ( 0.000000000000000000, -0.9999939076577903929, 0.003490651415223739937 ) ) ;
#87273 = FACE_OUTER_BOUND ( 'NONE', #92280, .T. ) ;
#87274 = AXIS2_PLACEMENT_3D ( 'NONE', #94539, #35009, #4861 ) ;
#87275 = AXIS2_PLACEMENT_3D ( 'NONE', #60888, #70711, #10490 ) ;
#87276 = DIRECTION ( 'NONE',  ( 0.000000000000000000, 1.000000000000000000, 0.000000000000000000 ) ) ;
#87277 = ORIENTED_EDGE ( 'NONE', *, *, #117304, .T. ) ;
#87278 = EDGE_LOOP ( 'NONE', ( #58469, #65284, #61965, #56357 ) ) ;
#87279 = ORIENTED_EDGE ( 'NONE', *, *, #109533, .F. ) ;
#87280 = ORIENTED_EDGE ( 'NONE', *, *, #104818, .T. ) ;
#87281 = FACE_OUTER_BOUND ( 'NONE', #127814, .T. ) ;
#87282 = DIRECTION ( 'NONE',  ( 0.000000000000000000, 0.000000000000000000, -1.000000000000000000 ) ) ;
#87284 = EDGE_LOOP ( 'NONE', ( #88970, #80395, #97265, #77241 ) ) ;
#87283 = ORIENTED_EDGE ( 'NONE', *, *, #122745, .T. ) ;
#87285 = VERTEX_POINT ( 'NONE', #123977 ) ;
#87287 = AXIS2_PLACEMENT_3D ( 'NONE', #42883, #71664, #112886 ) ;
#87286 = DIRECTION ( 'NONE',  ( -0.000000000000000000, 1.000000000000000000, -0.000000000000000000 ) ) ;
#87288 = CONICAL_SURFACE ( 'NONE', #116534, 0.09999999999999982514, 0.003490658503988666988 ) ;
#87289 = CIRCLE ( 'NONE', #53943, 0.09999999999999982514 ) ;
#87290 = CARTESIAN_POINT ( 'NONE',  ( 2.499999999999947153, 2.500000000000000000, -3.637306695894650055 ) ) ;
#87291 = DIRECTION ( 'NONE',  ( 0.000000000000000000, -0.000000000000000000, 1.000000000000000000 ) ) ;
#87292 = DIRECTION ( 'NONE',  ( 0.000000000000000000, -0.9999939076577903929, 0.003490651415223739937 ) ) ;
#87293 = CARTESIAN_POINT ( 'NONE',  ( -8.750000000000010658, 12.50000000000000000, -7.253104124594885960 ) ) ;
#87294 = LINE ( 'NONE', #109534, #56996 ) ;
#87295 = AXIS2_PLACEMENT_3D ( 'NONE', #33855, #4368, #114983 ) ;
#87296 = VERTEX_POINT ( 'NONE', #34345 ) ;
#87297 = DIRECTION ( 'NONE',  ( 0.000000000000000000, 0.000000000000000000, -1.000000000000000000 ) ) ;
#87298 = ORIENTED_EDGE ( 'NONE', *, *, #22761, .F. ) ;
#87300 = AXIS2_PLACEMENT_3D ( 'NONE', #17829, #5429, #66920 ) ;
#87299 = AXIS2_PLACEMENT_3D ( 'NONE', #210, #58526, #40165 ) ;
#87301 = ORIENTED_EDGE ( 'NONE', *, *, #44871, .F. ) ;
#87302 = ORIENTED_EDGE ( 'NONE', *, *, #105736, .T. ) ;
#87303 = DIRECTION ( 'NONE',  ( -4.274815082592931898E-19, -0.9999939076577903929, -0.003490651415223739937 ) ) ;
#87304 = ORIENTED_EDGE ( 'NONE', *, *, #4366, .T. ) ;
#87305 = ORIENTED_EDGE ( 'NONE', *, *, #96280, .T. ) ;
#87306 = DIRECTION ( 'NONE',  ( 0.000000000000000000, 0.000000000000000000, -1.000000000000000000 ) ) ;
#87307 = EDGE_CURVE ( 'NONE', #37082, #38247, #85723, .T. ) ;
#87308 = CARTESIAN_POINT ( 'NONE',  ( 13.74999999999989697, 2.500000000000000000, 2.957883832488649389 ) ) ;
#87309 = CARTESIAN_POINT ( 'NONE',  ( 15.39999999999989200, 12.50000000000000000, -0.6928203230275542523 ) ) ;
#87310 = PLANE ( 'NONE',  #58789 ) ;
#87311 = DIRECTION ( 'NONE',  ( 0.000000000000000000, 0.000000000000000000, -1.000000000000000000 ) ) ;
#87312 = VECTOR ( 'NONE', #109154, 1000.000000000000000 ) ;
#87313 = ORIENTED_EDGE ( 'NONE', *, *, #128714, .F. ) ;
#87314 = CARTESIAN_POINT ( 'NONE',  ( 2.049999999999950084, 12.50000000000000000, 2.165063509461097713 ) ) ;
#87315 = VERTEX_POINT ( 'NONE', #35618 ) ;
#87316 = DIRECTION ( 'NONE',  ( 0.000000000000000000, 1.000000000000000000, 0.000000000000000000 ) ) ;
#87317 = VERTEX_POINT ( 'NONE', #46081 ) ;
#87318 = DIRECTION ( 'NONE',  ( 0.000000000000000000, 0.000000000000000000, 1.000000000000000000 ) ) ;
#87319 = DIRECTION ( 'NONE',  ( -0.000000000000000000, -1.000000000000000000, -0.000000000000000000 ) ) ;
#87320 = ORIENTED_EDGE ( 'NONE', *, *, #103970, .T. ) ;
#87321 = CARTESIAN_POINT ( 'NONE',  ( -13.29999999999998828, 12.50000000000000000, 4.395220292106234439 ) ) ;
#87322 = DIRECTION ( 'NONE',  ( 0.000000000000000000, -0.9999939076577903929, 0.003490651415223739937 ) ) ;
#87323 = VERTEX_POINT ( 'NONE', #85975 ) ;
#87324 = CIRCLE ( 'NONE', #70614, 0.1000000000000000472 ) ;
#87325 = CIRCLE ( 'NONE', #104069, 0.06509327318403745899 ) ;
#87326 = LINE ( 'NONE', #37613, #65400 ) ;
#87327 = ORIENTED_EDGE ( 'NONE', *, *, #44201, .T. ) ;
#87328 = VERTEX_POINT ( 'NONE', #114175 ) ;
#87329 = DIRECTION ( 'NONE',  ( 0.000000000000000000, 1.000000000000000000, 0.000000000000000000 ) ) ;
#87330 = FACE_OUTER_BOUND ( 'NONE', #106842, .T. ) ;
#87331 = CARTESIAN_POINT ( 'NONE',  ( 186.0468750003414300, -8.734944146203032389, -1.604583208406768146E-15 ) ) ;
#87332 = DIRECTION ( 'NONE',  ( 0.000000000000000000, 0.000000000000000000, -1.000000000000000000 ) ) ;
#87333 = AXIS2_PLACEMENT_3D ( 'NONE', #27119, #65742, #105683 ) ;
#87334 = DIRECTION ( 'NONE',  ( 0.000000000000000000, 1.000000000000000000, 0.000000000000000000 ) ) ;
#87335 = VECTOR ( 'NONE', #99053, 1000.000000000000000 ) ;
#87336 = DIRECTION ( 'NONE',  ( 0.000000000000000000, 0.000000000000000000, 1.000000000000000000 ) ) ;
#87337 = EDGE_LOOP ( 'NONE', ( #17345, #78577, #42242, #99948, #14725, #11235, #55765 ) ) ;
#87338 = CARTESIAN_POINT ( 'NONE',  ( 6.449999999999931788, 2.500000000000000000, -2.411473670974877859 ) ) ;
#87341 = ADVANCED_FACE ( 'NONE', ( #105646 ), #71068, .T. ) ;
#87340 = AXIS2_PLACEMENT_3D ( 'NONE', #86456, #28197, #7896 ) ;
#87339 = CARTESIAN_POINT ( 'NONE',  ( 12.09999999999990550, 12.50000000000000000, -4.957854068765716882 ) ) ;
#87342 = ORIENTED_EDGE ( 'NONE', *, *, #77132, .T. ) ;
#87343 = AXIS2_PLACEMENT_3D ( 'NONE', #102329, #51945, #61107 ) ;
#87344 = EDGE_CURVE ( 'NONE', #9507, #20279, #54339, .T. ) ;
#87345 = DIRECTION ( 'NONE',  ( 0.000000000000000000, 0.000000000000000000, 1.000000000000000000 ) ) ;
#87346 = LINE ( 'NONE', #127301, #34312 ) ;
#87347 = CARTESIAN_POINT ( 'NONE',  ( 1.899999999999951283, 12.50000000000000000, 0.2813168883297362810 ) ) ;
#87348 = DIRECTION ( 'NONE',  ( 0.000000000000000000, 0.000000000000000000, 1.000000000000000000 ) ) ;
#87349 = EDGE_CURVE ( 'NONE', #114894, #13624, #60621, .T. ) ;
#87350 = DIRECTION ( 'NONE',  ( 0.000000000000000000, 0.000000000000000000, 1.000000000000000000 ) ) ;
#87351 = VERTEX_POINT ( 'NONE', #39507 ) ;
#87352 = CIRCLE ( 'NONE', #118664, 0.06509327318403745899 ) ;
#87353 = DIRECTION ( 'NONE',  ( 0.000000000000000000, 0.000000000000000000, 1.000000000000000000 ) ) ;
#87354 = DIRECTION ( 'NONE',  ( 0.000000000000000000, 1.000000000000000000, 0.000000000000000000 ) ) ;
#87355 = AXIS2_PLACEMENT_3D ( 'NONE', #70890, #42749, #50591 ) ;
#87356 = ADVANCED_FACE ( 'NONE', ( #48022 ), #79418, .T. ) ;
#87357 = EDGE_CURVE ( 'NONE', #44082, #4682, #37631, .T. ) ;
#87358 = EDGE_CURVE ( 'NONE', #119819, #107613, #123381, .T. ) ;
#87359 = ADVANCED_FACE ( 'NONE', ( #87906 ), #41840, .T. ) ;
#87360 = AXIS2_PLACEMENT_3D ( 'NONE', #4693, #42751, #114667 ) ;
#87361 = VERTEX_POINT ( 'NONE', #17223 ) ;
#87362 = VECTOR ( 'NONE', #46412, 1000.000000000000000 ) ;
#87363 = FACE_OUTER_BOUND ( 'NONE', #62315, .T. ) ;
#87364 = AXIS2_PLACEMENT_3D ( 'NONE', #33616, #34275, #93189 ) ;
#87365 = ORIENTED_EDGE ( 'NONE', *, *, #58041, .T. ) ;
#87366 = EDGE_LOOP ( 'NONE', ( #103830, #11499 ) ) ;
#87367 = DIRECTION ( 'NONE',  ( -0.000000000000000000, -1.000000000000000000, -0.000000000000000000 ) ) ;
#87368 = CIRCLE ( 'NONE', #62366, 0.1000000000000000472 ) ;
#87369 = VERTEX_POINT ( 'NONE', #29659 ) ;
#87370 = DIRECTION ( 'NONE',  ( 0.000000000000000000, 1.000000000000000000, 0.000000000000000000 ) ) ;
#87371 = DIRECTION ( 'NONE',  ( -0.000000000000000000, -1.000000000000000000, -0.000000000000000000 ) ) ;
#87372 = CIRCLE ( 'NONE', #76642, 0.06509327318403741736 ) ;
#87373 = DIRECTION ( 'NONE',  ( 0.000000000000000000, 1.000000000000000000, 0.000000000000000000 ) ) ;
#87374 = ORIENTED_EDGE ( 'NONE', *, *, #93356, .F. ) ;
#87375 = FACE_BOUND ( 'NONE', #23890, .T. ) ;
#87377 = ORIENTED_EDGE ( 'NONE', *, *, #14862, .F. ) ;
#87376 = DIRECTION ( 'NONE',  ( 0.000000000000000000, 0.000000000000000000, -1.000000000000000000 ) ) ;
#87378 = CARTESIAN_POINT ( 'NONE',  ( -1.050000000000038236, 12.50000000000000000, -1.818653347947326138 ) ) ;
#87379 = VECTOR ( 'NONE', #1442, 1000.000000000000000 ) ;
#87380 = CARTESIAN_POINT ( 'NONE',  ( 5.849999999999933031, 12.50000000000000000, 7.188010851410848723 ) ) ;
#87381 = ORIENTED_EDGE ( 'NONE', *, *, #77977, .T. ) ;
#87383 = AXIS2_PLACEMENT_3D ( 'NONE', #119251, #40060, #120550 ) ;
#87382 = CIRCLE ( 'NONE', #28926, 0.06509327318403745899 ) ;
#87384 = ORIENTED_EDGE ( 'NONE', *, *, #128105, .T. ) ;
#87385 = ORIENTED_EDGE ( 'NONE', *, *, #544, .F. ) ;
#87386 = CARTESIAN_POINT ( 'NONE',  ( -12.49999999999999467, 12.50000000000000000, 0.6928203230275535862 ) ) ;
#87387 = CARTESIAN_POINT ( 'NONE',  ( -10.40000000000000213, 2.500000000000000000, 3.737306695894644371 ) ) ;
#87388 = CARTESIAN_POINT ( 'NONE',  ( 11.04999999999990834, 2.500000000000000000, 1.818653347947321475 ) ) ;
#87389 = EDGE_CURVE ( 'NONE', #34323, #128096, #69001, .T. ) ;
#87390 = FACE_BOUND ( 'NONE', #109340, .T. ) ;
#87391 = ORIENTED_EDGE ( 'NONE', *, *, #13925, .F. ) ;
#87392 = PLANE ( 'NONE',  #3067 ) ;
#87393 = CARTESIAN_POINT ( 'NONE',  ( 0.8499999999999527933, 2.500000000000000000, 7.288010851410849256 ) ) ;
#87394 = EDGE_LOOP ( 'NONE', ( #18629, #73115, #106334, #103199 ) ) ;
#87395 = DIRECTION ( 'NONE',  ( 0.000000000000000000, 0.000000000000000000, 1.000000000000000000 ) ) ;
#87397 = EDGE_CURVE ( 'NONE', #53276, #108500, #76830, .T. ) ;
#87396 = PLANE ( 'NONE',  #86224 ) ;
#87398 = DIRECTION ( 'NONE',  ( 0.000000000000000000, 0.000000000000000000, 1.000000000000000000 ) ) ;
#87399 = ADVANCED_FACE ( 'NONE', ( #127853 ), #109506, .T. ) ;
#87400 = DIRECTION ( 'NONE',  ( 0.000000000000000000, 0.000000000000000000, 1.000000000000000000 ) ) ;
#87401 = CARTESIAN_POINT ( 'NONE',  ( -7.500000000000016875, 12.50000000000000000, -3.702399969078687292 ) ) ;
#87402 = EDGE_CURVE ( 'NONE', #109920, #79243, #119186, .T. ) ;
#87403 = VERTEX_POINT ( 'NONE', #89220 ) ;
#87404 = EDGE_LOOP ( 'NONE', ( #12143, #51732 ) ) ;
#87405 = ORIENTED_EDGE ( 'NONE', *, *, #48692, .F. ) ;
#87406 = AXIS2_PLACEMENT_3D ( 'NONE', #91637, #2593, #80542 ) ;
#87407 = CONICAL_SURFACE ( 'NONE', #41487, 0.1000000000000000472, 0.003490658503988666988 ) ;
#87408 = EDGE_LOOP ( 'NONE', ( #46915, #79013, #70423, #117710 ) ) ;
#87409 = VERTEX_POINT ( 'NONE', #49323 ) ;
#87410 = DIRECTION ( 'NONE',  ( -4.274815082592931898E-19, -0.9999939076577903929, -0.003490651415223739937 ) ) ;
#87411 = EDGE_CURVE ( 'NONE', #2269, #86712, #118029, .T. ) ;
#87412 = CARTESIAN_POINT ( 'NONE',  ( -7.100000000000018296, 2.500000000000000000, -4.330127018922201643 ) ) ;
#87414 = EDGE_CURVE ( 'NONE', #35299, #123030, #4142, .T. ) ;
#87413 = ORIENTED_EDGE ( 'NONE', *, *, #82982, .F. ) ;
#87415 = FACE_BOUND ( 'NONE', #35820, .T. ) ;
#87416 = DIRECTION ( 'NONE',  ( 0.000000000000000000, 0.000000000000000000, 1.000000000000000000 ) ) ;
#87417 = EDGE_CURVE ( 'NONE', #41715, #112785, #98246, .T. ) ;
#87419 = EDGE_CURVE ( 'NONE', #72558, #110762, #97747, .T. ) ;
#87418 = AXIS2_PLACEMENT_3D ( 'NONE', #9885, #99568, #49828 ) ;
#87420 = AXIS2_PLACEMENT_3D ( 'NONE', #92806, #12917, #103905 ) ;
#87421 = ADVANCED_FACE ( 'NONE', ( #77464 ), #50239, .T. ) ;
#87422 = CARTESIAN_POINT ( 'NONE',  ( -9.150000000000011013, 12.50000000000000000, -5.867463478539781896 ) ) ;
#87423 = CARTESIAN_POINT ( 'NONE',  ( 184.4999999999999716, -5.927738724303143414, 4.757631484588563886 ) ) ;
#87424 = CARTESIAN_POINT ( 'NONE',  ( 13.34999999999989662, 2.500000000000000000, -2.957883832488653830 ) ) ;
#87425 = CARTESIAN_POINT ( 'NONE',  ( 4.349999999999938360, 12.50000000000000000, 1.883746621131358934 ) ) ;
#87426 = ORIENTED_EDGE ( 'NONE', *, *, #99415, .T. ) ;
#87427 = DIRECTION ( 'NONE',  ( 0.000000000000000000, -0.000000000000000000, 1.000000000000000000 ) ) ;
#87428 = EDGE_CURVE ( 'NONE', #3076, #92060, #121235, .T. ) ;
#87429 = VERTEX_POINT ( 'NONE', #117355 ) ;
#87430 = CIRCLE ( 'NONE', #68563, 0.06509327318403741736 ) ;
#87431 = ORIENTED_EDGE ( 'NONE', *, *, #99197, .F. ) ;
#87432 = ORIENTED_EDGE ( 'NONE', *, *, #39706, .F. ) ;
#87433 = CARTESIAN_POINT ( 'NONE',  ( 5.649999999999932854, 2.500000000000000000, 1.718653347947321386 ) ) ;
#87434 = CARTESIAN_POINT ( 'NONE',  ( 7.180215335565443446, 2.499999999999999112, 8.697219394475776966 ) ) ;
#87435 = CARTESIAN_POINT ( 'NONE',  ( 1.849999999999951017, 12.50000000000000000, -6.213873640053564351 ) ) ;
#87436 = VERTEX_POINT ( 'NONE', #126574 ) ;
#87437 = CARTESIAN_POINT ( 'NONE',  ( 12.30568799110194611, 2.500000000000000000, -7.490555764795464810 ) ) ;
#87438 = AXIS2_PLACEMENT_3D ( 'NONE', #75206, #63461, #32730 ) ;
#87439 = CARTESIAN_POINT ( 'NONE',  ( -13.34999999999999076, 2.500000000000000000, 1.472243186433549456 ) ) ;
#87440 = DIRECTION ( 'NONE',  ( 0.000000000000000000, 1.000000000000000000, 0.000000000000000000 ) ) ;
#87441 = CARTESIAN_POINT ( 'NONE',  ( 186.3593750003414016, 0.000000000000000000, 7.564683531250000925 ) ) ;
#87442 = CARTESIAN_POINT ( 'NONE',  ( 7.699999999999925571, 12.50000000000000000, 3.918623584224382839 ) ) ;
#87443 = DIRECTION ( 'NONE',  ( 0.000000000000000000, 0.000000000000000000, -1.000000000000000000 ) ) ;
#87444 = CONICAL_SURFACE ( 'NONE', #24769, 0.09999999999999982514, 0.003490658503988666988 ) ;
#87445 = DIRECTION ( 'NONE',  ( 0.000000000000000000, 0.000000000000000000, -1.000000000000000000 ) ) ;
#87446 = ORIENTED_EDGE ( 'NONE', *, *, #5355, .T. ) ;
#87447 = DIRECTION ( 'NONE',  ( 0.000000000000000000, 0.000000000000000000, -1.000000000000000000 ) ) ;
#87448 = AXIS2_PLACEMENT_3D ( 'NONE', #56885, #120356, #10388 ) ;
#87449 = VERTEX_POINT ( 'NONE', #27710 ) ;
#87450 = ORIENTED_EDGE ( 'NONE', *, *, #91048, .F. ) ;
#87451 = CARTESIAN_POINT ( 'NONE',  ( -1.450000000000035927, 12.50000000000000000, -1.818653347947326138 ) ) ;
#87452 = CARTESIAN_POINT ( 'NONE',  ( -6.850000000000017408, 12.50000000000000000, -6.148780366869526226 ) ) ;
#87453 = FACE_OUTER_BOUND ( 'NONE', #76958, .T. ) ;
#87454 = EDGE_LOOP ( 'NONE', ( #95516, #80058 ) ) ;
#87455 = ORIENTED_EDGE ( 'NONE', *, *, #83179, .F. ) ;
#87456 = CARTESIAN_POINT ( 'NONE',  ( -6.250000000000015987, 2.500000000000000000, 1.472243186433545459 ) ) ;
#87457 = AXIS2_PLACEMENT_3D ( 'NONE', #123743, #45214, #124415 ) ;
#87458 = ADVANCED_FACE ( 'NONE', ( #8699 ), #35570, .T. ) ;
#87459 = DIRECTION ( 'NONE',  ( 0.000000000000000000, 0.000000000000000000, -1.000000000000000000 ) ) ;
#87460 = CARTESIAN_POINT ( 'NONE',  ( 11.04999999999991012, 2.500000000000000000, 6.841600689897072485 ) ) ;
#87461 = EDGE_LOOP ( 'NONE', ( #100981, #103388 ) ) ;
#87462 = VERTEX_POINT ( 'NONE', #60140 ) ;
#87463 = FACE_OUTER_BOUND ( 'NONE', #118352, .T. ) ;
#87464 = AXIS2_PLACEMENT_3D ( 'NONE', #106747, #17048, #85818 ) ;
#87465 = VERTEX_POINT ( 'NONE', #20192 ) ;
#87466 = DIRECTION ( 'NONE',  ( 0.000000000000000000, 0.000000000000000000, 1.000000000000000000 ) ) ;
#87467 = CARTESIAN_POINT ( 'NONE',  ( 1.849999999999949685, 2.500000000000000000, -2.511473670974877948 ) ) ;
#87468 = ORIENTED_EDGE ( 'NONE', *, *, #84640, .T. ) ;
#87469 = DIRECTION ( 'NONE',  ( 0.000000000000000000, 0.000000000000000000, -1.000000000000000000 ) ) ;
#87470 = CARTESIAN_POINT ( 'NONE',  ( -14.54999999999998472, 12.50000000000000000, -2.165063509461099489 ) ) ;
#87471 = FACE_OUTER_BOUND ( 'NONE', #41060, .T. ) ;
#87472 = CIRCLE ( 'NONE', #68699, 0.06509327318403745899 ) ;
#87473 = EDGE_CURVE ( 'NONE', #26297, #81382, #56472, .T. ) ;
#87474 = CARTESIAN_POINT ( 'NONE',  ( 4.799999999999939426, 2.500000000000000000, -4.776537180435977525 ) ) ;
#87475 = ORIENTED_EDGE ( 'NONE', *, *, #45929, .F. ) ;
#87476 = LINE ( 'NONE', #7629, #117849 ) ;
#87478 = AXIS2_PLACEMENT_3D ( 'NONE', #26050, #36529, #95435 ) ;
#87477 = CIRCLE ( 'NONE', #83388, 0.5000000000000004441 ) ;
#87479 = VERTEX_POINT ( 'NONE', #21478 ) ;
#87480 = VERTEX_POINT ( 'NONE', #111804 ) ;
#87481 = PLANE ( 'NONE',  #37397 ) ;
#87482 = DIRECTION ( 'NONE',  ( 0.000000000000000000, -0.000000000000000000, 1.000000000000000000 ) ) ;
#87483 = CARTESIAN_POINT ( 'NONE',  ( 10.39999999999990976, 2.500000000000000000, -4.230127018922201998 ) ) ;
#87484 = CARTESIAN_POINT ( 'NONE',  ( 9.349999999999916156, 2.500000000000000000, 6.048780366869520364 ) ) ;
#87485 = CARTESIAN_POINT ( 'NONE',  ( -12.89999999999999147, 2.500000000000000000, -4.230127018922199333 ) ) ;
#87486 = DIRECTION ( 'NONE',  ( -0.000000000000000000, -1.000000000000000000, -0.000000000000000000 ) ) ;
#87487 = CARTESIAN_POINT ( 'NONE',  ( 10.84999999999991260, 12.50000000000000000, 7.188010851410848723 ) ) ;
#87488 = DIRECTION ( 'NONE',  ( 0.000000000000000000, -0.9999939076577903929, 0.003490651415223739937 ) ) ;
#87489 = DIRECTION ( 'NONE',  ( 0.000000000000000000, 1.000000000000000000, 0.000000000000000000 ) ) ;
#87490 = CIRCLE ( 'NONE', #26866, 0.1000000000000002554 ) ;
#87491 = CARTESIAN_POINT ( 'NONE',  ( -4.600000000000024514, 2.500000000000000000, -0.5928203230275542746 ) ) ;
#87492 = AXIS2_PLACEMENT_3D ( 'NONE', #77854, #7824, #108610 ) ;
#87493 = EDGE_CURVE ( 'NONE', #7181, #117167, #90196, .T. ) ;
#87494 = AXIS2_PLACEMENT_3D ( 'NONE', #35994, #35352, #56265 ) ;
#87495 = ORIENTED_EDGE ( 'NONE', *, *, #5373, .T. ) ;
#87496 = CIRCLE ( 'NONE', #129310, 0.06509327318403745899 ) ;
#87497 = DIRECTION ( 'NONE',  ( 0.000000000000000000, 1.000000000000000000, 0.000000000000000000 ) ) ;
#87498 = CARTESIAN_POINT ( 'NONE',  ( 8.949999999999919353, 2.500000000000000000, 2.611473670974873151 ) ) ;
#87499 = CARTESIAN_POINT ( 'NONE',  ( -2.100000000000033840, 2.500000000000000000, 4.922947341949748257 ) ) ;
#87500 = FACE_OUTER_BOUND ( 'NONE', #10287, .T. ) ;
#87501 = LINE ( 'NONE', #58074, #10304 ) ;
#87502 = EDGE_CURVE ( 'NONE', #7687, #32088, #2088, .T. ) ;
#87503 = CIRCLE ( 'NONE', #47827, 0.09999999999999982514 ) ;
#87504 = VERTEX_POINT ( 'NONE', #110499 ) ;
#87505 = CONICAL_SURFACE ( 'NONE', #127335, 0.1000000000000002554, 0.003490658503988666988 ) ;
#87506 = CARTESIAN_POINT ( 'NONE',  ( -9.200000000000006395, 2.500000000000000000, 4.330127018922196314 ) ) ;
#87507 = AXIS2_PLACEMENT_3D ( 'NONE', #27918, #68479, #67836 ) ;
#87508 = AXIS2_PLACEMENT_3D ( 'NONE', #19842, #37552, #78115 ) ;
#87509 = DIRECTION ( 'NONE',  ( 0.000000000000000000, 0.000000000000000000, 1.000000000000000000 ) ) ;
#87511 = ORIENTED_EDGE ( 'NONE', *, *, #123228, .T. ) ;
#87510 = CARTESIAN_POINT ( 'NONE',  ( -0.4500000000000402012, 12.50000000000000000, 6.495190528383297135 ) ) ;
#87512 = EDGE_CURVE ( 'NONE', #63031, #6029, #94139, .T. ) ;
#87513 = EDGE_CURVE ( 'NONE', #5812, #105300, #83768, .T. ) ;
#87514 = EDGE_CURVE ( 'NONE', #76556, #42141, #106737, .T. ) ;
#87515 = EDGE_CURVE ( 'NONE', #120954, #87216, #90011, .T. ) ;
#87516 = EDGE_CURVE ( 'NONE', #70542, #126334, #39217, .T. ) ;
#87517 = AXIS2_PLACEMENT_3D ( 'NONE', #15418, #55369, #5594 ) ;
#87518 = ORIENTED_EDGE ( 'NONE', *, *, #25621, .F. ) ;
#87519 = CIRCLE ( 'NONE', #64543, 0.09999999999999999167 ) ;
#87520 = EDGE_LOOP ( 'NONE', ( #100982, #14456, #47893, #67932 ) ) ;
#87521 = ORIENTED_EDGE ( 'NONE', *, *, #108820, .T. ) ;
#87522 = ORIENTED_EDGE ( 'NONE', *, *, #50687, .T. ) ;
#87523 = FACE_OUTER_BOUND ( 'NONE', #75841, .T. ) ;
#87524 = EDGE_CURVE ( 'NONE', #79569, #95487, #71149, .T. ) ;
#87525 = FACE_OUTER_BOUND ( 'NONE', #6452, .T. ) ;
#87526 = CARTESIAN_POINT ( 'NONE',  ( -9.350000000000008527, 2.500000000000000000, -6.148780366869520897 ) ) ;
#87527 = EDGE_CURVE ( 'NONE', #13366, #63398, #1827, .T. ) ;
#87528 = FACE_OUTER_BOUND ( 'NONE', #8861, .T. ) ;
#87529 = AXIS2_PLACEMENT_3D ( 'NONE', #65714, #14665, #104357 ) ;
#87531 = EDGE_LOOP ( 'NONE', ( #127857, #89711 ) ) ;
#87530 = EDGE_CURVE ( 'NONE', #86533, #2794, #110852, .T. ) ;
#87533 = CARTESIAN_POINT ( 'NONE',  ( 3.149999999999942624, 2.500000000000000000, 6.048780366869521252 ) ) ;
#87532 = B_SPLINE_CURVE_WITH_KNOTS ( 'NONE', 3,
 ( #56522, #18537, #76178, #116094 ),
 .UNSPECIFIED., .F., .F.,
 ( 4, 4 ),
 ( 8.673617379884035472E-19, 0.002128161363186473892 ),
 .UNSPECIFIED. ) ;
#87534 = ORIENTED_EDGE ( 'NONE', *, *, #86177, .T. ) ;
#87535 = VECTOR ( 'NONE', #26671, 1000.000000000000000 ) ;
#87536 = CARTESIAN_POINT ( 'NONE',  ( 35.04009662971161276, -1.562391656609272594, -4.793251516055618389 ) ) ;
#87537 = DIRECTION ( 'NONE',  ( 0.000000000000000000, -0.9999939076577903929, 0.003490651415223739937 ) ) ;
#87538 = CARTESIAN_POINT ( 'NONE',  ( 12.49999999999990052, 2.500000000000000000, 0.7928203230275495672 ) ) ;
#87539 = CARTESIAN_POINT ( 'NONE',  ( -6.700000000000016165, 2.500000000000000000, 4.230127018922196669 ) ) ;
#87540 = CARTESIAN_POINT ( 'NONE',  ( -12.09999999999999609, 2.500000000000000000, 4.430127018922196847 ) ) ;
#87541 = VERTEX_POINT ( 'NONE', #99405 ) ;
#87542 = AXIS2_PLACEMENT_3D ( 'NONE', #114860, #23928, #113590 ) ;
#87543 = EDGE_LOOP ( 'NONE', ( #118838, #89509, #129247, #57865 ) ) ;
#87544 = ORIENTED_EDGE ( 'NONE', *, *, #82991, .T. ) ;
#87545 = ORIENTED_EDGE ( 'NONE', *, *, #64687, .F. ) ;
#87546 = DIRECTION ( 'NONE',  ( 0.000000000000000000, 0.000000000000000000, 1.000000000000000000 ) ) ;
#87547 = CARTESIAN_POINT ( 'NONE',  ( 1.849999999999949685, 2.500000000000000000, 1.818653347947321475 ) ) ;
#87548 = DIRECTION ( 'NONE',  ( 0.000000000000000000, 0.000000000000000000, 1.000000000000000000 ) ) ;
#87549 = FACE_BOUND ( 'NONE', #78947, .T. ) ;
#87550 = DIRECTION ( 'NONE',  ( 0.000000000000000000, 0.000000000000000000, 1.000000000000000000 ) ) ;
#87551 = DIRECTION ( 'NONE',  ( 0.000000000000000000, 0.000000000000000000, -1.000000000000000000 ) ) ;
#87552 = CIRCLE ( 'NONE', #29096, 0.06509327318403745899 ) ;
#87553 = DIRECTION ( 'NONE',  ( -0.000000000000000000, -1.000000000000000000, -0.000000000000000000 ) ) ;
#87554 = LINE ( 'NONE', #35890, #60408 ) ;
#87555 = VECTOR ( 'NONE', #22997, 1000.000000000000000 ) ;
#87556 = CARTESIAN_POINT ( 'NONE',  ( 185.5468750003414300, -8.734944146203032389, -1.604583208406767949E-15 ) ) ;
#87557 = PLANE ( 'NONE',  #113670 ) ;
#87558 = AXIS2_PLACEMENT_3D ( 'NONE', #12109, #11470, #31769 ) ;
#87559 = DIRECTION ( 'NONE',  ( 0.000000000000000000, 1.000000000000000000, 0.000000000000000000 ) ) ;
#87560 = CARTESIAN_POINT ( 'NONE',  ( 7.699999999999923794, 2.500000000000000000, 4.776537180435972196 ) ) ;
#87561 = AXIS2_PLACEMENT_3D ( 'NONE', #119230, #120526, #29561 ) ;
#87562 = EDGE_LOOP ( 'NONE', ( #54139, #68237, #57770, #97008 ) ) ;
#87563 = VERTEX_POINT ( 'NONE', #100664 ) ;
#87564 = EDGE_LOOP ( 'NONE', ( #42841, #26738, #75667, #52018 ) ) ;
#87565 = VERTEX_POINT ( 'NONE', #100044 ) ;
#87566 = VECTOR ( 'NONE', #118823, 1000.000000000000000 ) ;
#87567 = FACE_OUTER_BOUND ( 'NONE', #97804, .T. ) ;
#87568 = EDGE_CURVE ( 'NONE', #120419, #20260, #9728, .T. ) ;
#87569 = FACE_BOUND ( 'NONE', #108327, .T. ) ;
#87570 = FACE_OUTER_BOUND ( 'NONE', #56168, .T. ) ;
#87571 = EDGE_CURVE ( 'NONE', #79978, #4381, #123462, .T. ) ;
#87573 = AXIS2_PLACEMENT_3D ( 'NONE', #111697, #53428, #33145 ) ;
#87572 = CIRCLE ( 'NONE', #79288, 0.1000000000000000472 ) ;
#87574 = ADVANCED_FACE ( 'NONE', ( #1190 ), #41142, .T. ) ;
#87575 = VERTEX_POINT ( 'NONE', #51599 ) ;
#87576 = PLANE ( 'NONE',  #36278 ) ;
#87577 = CARTESIAN_POINT ( 'NONE',  ( 7.899999999999924860, 12.50000000000000000, -4.330127018922201643 ) ) ;
#87578 = CARTESIAN_POINT ( 'NONE',  ( -6.450000000000016165, 12.50000000000000000, 2.576566944158910744 ) ) ;
#87579 = ORIENTED_EDGE ( 'NONE', *, *, #125485, .F. ) ;
#87580 = DIRECTION ( 'NONE',  ( 0.000000000000000000, 0.000000000000000000, 1.000000000000000000 ) ) ;
#87581 = DIRECTION ( 'NONE',  ( -0.000000000000000000, 1.000000000000000000, -0.000000000000000000 ) ) ;
#87582 = ADVANCED_FACE ( 'NONE', ( #81682 ), #37714, .T. ) ;
#87583 = VERTEX_POINT ( 'NONE', #88933 ) ;
#87584 = AXIS2_PLACEMENT_3D ( 'NONE', #14943, #54897, #94831 ) ;
#87585 = DIRECTION ( 'NONE',  ( 0.000000000000000000, 0.000000000000000000, -1.000000000000000000 ) ) ;
#87586 = LINE ( 'NONE', #117031, #70604 ) ;
#87587 = ORIENTED_EDGE ( 'NONE', *, *, #83944, .T. ) ;
#87588 = AXIS2_PLACEMENT_3D ( 'NONE', #118429, #98784, #69988 ) ;
#87589 = CARTESIAN_POINT ( 'NONE',  ( 10.59999999999991260, 12.50000000000000000, 0.2813168883297361700 ) ) ;
#87590 = AXIS2_PLACEMENT_3D ( 'NONE', #7807, #108593, #118410 ) ;
#87591 = DIRECTION ( 'NONE',  ( 0.000000000000000000, 0.000000000000000000, 1.000000000000000000 ) ) ;
#87592 = ORIENTED_EDGE ( 'NONE', *, *, #115542, .F. ) ;
#87593 = DIRECTION ( 'NONE',  ( 0.000000000000000000, -0.9999939076577903929, 0.003490651415223739937 ) ) ;
#87594 = ORIENTED_EDGE ( 'NONE', *, *, #95668, .T. ) ;
#87595 = ORIENTED_EDGE ( 'NONE', *, *, #4467, .F. ) ;
#87596 = FACE_OUTER_BOUND ( 'NONE', #98336, .T. ) ;
#87597 = EDGE_CURVE ( 'NONE', #68741, #28244, #67021, .T. ) ;
#87599 = EDGE_LOOP ( 'NONE', ( #49946, #33565, #92713, #40088 ) ) ;
#87598 = CONICAL_SURFACE ( 'NONE', #35302, 0.1000000000000000472, 0.003490658503988666988 ) ;
#87600 = CARTESIAN_POINT ( 'NONE',  ( -1.050000000000038236, 12.50000000000000000, -1.818653347947326138 ) ) ;
#87601 = FACE_BOUND ( 'NONE', #36066, .T. ) ;
#87602 = CONICAL_SURFACE ( 'NONE', #79318, 0.1000000000000002554, 0.003490658503988666988 ) ;
#87603 = AXIS2_PLACEMENT_3D ( 'NONE', #39362, #9876, #120470 ) ;
#87604 = VERTEX_POINT ( 'NONE', #119039 ) ;
#87605 = CARTESIAN_POINT ( 'NONE',  ( -3.350000000000028955, 12.50000000000000000, 5.867463478539781896 ) ) ;
#87606 = ORIENTED_EDGE ( 'NONE', *, *, #72772, .T. ) ;
#87607 = LINE ( 'NONE', #96774, #85893 ) ;
#87608 = DIRECTION ( 'NONE',  ( -4.274815082592931898E-19, -0.9999939076577903929, -0.003490651415223739937 ) ) ;
#87609 = CARTESIAN_POINT ( 'NONE',  ( -3.749999999999991118, 12.50000000000000000, 2.230156782645134950 ) ) ;
#87610 = CARTESIAN_POINT ( 'NONE',  ( -8.350000000000012079, 2.500000000000000000, 2.957883832488649389 ) ) ;
#87611 = CARTESIAN_POINT ( 'NONE',  ( 17.50000000000011013, 2.362783583789868302, -3.757116699121217707 ) ) ;
#87612 = CIRCLE ( 'NONE', #56406, 0.06509327318403745899 ) ;
#87613 = EDGE_LOOP ( 'NONE', ( #93219, #91758, #45577, #126557 ) ) ;
#87614 = ORIENTED_EDGE ( 'NONE', *, *, #3861, .T. ) ;
#87615 = FACE_OUTER_BOUND ( 'NONE', #63598, .T. ) ;
#87616 = EDGE_CURVE ( 'NONE', #76977, #84673, #29404, .T. ) ;
#87617 = LINE ( 'NONE', #86979, #112083 ) ;
#87618 = CARTESIAN_POINT ( 'NONE',  ( -2.950000000000033484, 12.50000000000000000, -6.430097255199264339 ) ) ;
#87620 = EDGE_LOOP ( 'NONE', ( #28937, #29552, #12139, #35995 ) ) ;
#87619 = ORIENTED_EDGE ( 'NONE', *, *, #6252, .F. ) ;
#87621 = ORIENTED_EDGE ( 'NONE', *, *, #51964, .T. ) ;
#87622 = CARTESIAN_POINT ( 'NONE',  ( -5.850000000000018296, 12.50000000000000000, 2.792790559304612064 ) ) ;
#87623 = DIRECTION ( 'NONE',  ( -0.000000000000000000, 1.000000000000000000, -0.000000000000000000 ) ) ;
#87624 = ITEM_DEFINED_TRANSFORMATION ( 'NONE', 'NONE', #94426,  #108296 ) ;
#87625 = CARTESIAN_POINT ( 'NONE',  ( 1.049999999999954525, 2.500000000000000000, -2.511473670974877948 ) ) ;
#87626 = DIRECTION ( 'NONE',  ( 0.000000000000000000, 0.000000000000000000, 1.000000000000000000 ) ) ;
#87627 = DIRECTION ( 'NONE',  ( -4.274815082592931898E-19, -0.9999939076577903929, -0.003490651415223739937 ) ) ;
#87628 = DIRECTION ( 'NONE',  ( -1.000000000000000000, 0.000000000000000000, 0.000000000000000000 ) ) ;
#87629 = CIRCLE ( 'NONE', #39645, 0.09999999999999982514 ) ;
#87630 = DIRECTION ( 'NONE',  ( 0.000000000000000000, 1.000000000000000000, 0.000000000000000000 ) ) ;
#87631 = EDGE_CURVE ( 'NONE', #15166, #103763, #81611, .T. ) ;
#87632 = CARTESIAN_POINT ( 'NONE',  ( 184.7395833340161175, 4.445597072760175905, 7.699999999999896261 ) ) ;
#87633 = VERTEX_POINT ( 'NONE', #33254 ) ;
#87634 = ORIENTED_EDGE ( 'NONE', *, *, #104727, .F. ) ;
#87635 = CARTESIAN_POINT ( 'NONE',  ( 3.349999999999941913, 12.50000000000000000, 6.495190528383297135 ) ) ;
#87636 = LINE ( 'NONE', #98743, #44542 ) ;
#87637 = EDGE_LOOP ( 'NONE', ( #56859, #3126 ) ) ;
#87638 = ORIENTED_EDGE ( 'NONE', *, *, #64625, .T. ) ;
#87639 = DIRECTION ( 'NONE',  ( 0.000000000000000000, 0.000000000000000000, 1.000000000000000000 ) ) ;
#87640 = CARTESIAN_POINT ( 'NONE',  ( -13.34999999999999076, 2.500000000000000000, -2.065063509461099844 ) ) ;
#87641 = AXIS2_PLACEMENT_3D ( 'NONE', #123856, #74136, #42098 ) ;
#87642 = CARTESIAN_POINT ( 'NONE',  ( -5.850000000000018296, 2.500000000000000000, 7.188010851410848723 ) ) ;
#87643 = DIRECTION ( 'NONE',  ( 1.000000000000000000, 0.000000000000000000, 0.000000000000000000 ) ) ;
#87644 = CARTESIAN_POINT ( 'NONE',  ( -3.950000000000025491, 2.500000000000000000, 6.148780366869520897 ) ) ;
#87645 = FACE_OUTER_BOUND ( 'NONE', #82962, .T. ) ;
#87646 = DIRECTION ( 'NONE',  ( -4.274815082592931898E-19, -0.9999939076577903929, -0.003490651415223739937 ) ) ;
#87647 = ORIENTED_EDGE ( 'NONE', *, *, #86853, .F. ) ;
#87648 = LINE ( 'NONE', #87013, #36851 ) ;
#87649 = AXIS2_PLACEMENT_3D ( 'NONE', #17908, #78795, #87291 ) ;
#87650 = DIRECTION ( 'NONE',  ( 0.000000000000000000, 1.000000000000000000, 0.000000000000000000 ) ) ;
#87651 = ORIENTED_EDGE ( 'NONE', *, *, #22918, .T. ) ;
#87652 = EDGE_CURVE ( 'NONE', #126997, #24357, #35183, .T. ) ;
#87654 = AXIS2_PLACEMENT_3D ( 'NONE', #6389, #116369, #46341 ) ;
#87653 = CIRCLE ( 'NONE', #102346, 0.1000000000000000472 ) ;
#87655 = ORIENTED_EDGE ( 'NONE', *, *, #91665, .T. ) ;
#87656 = CIRCLE ( 'NONE', #10394, 0.06509327318403745899 ) ;
#87657 = VERTEX_POINT ( 'NONE', #52877 ) ;
#87658 = VERTEX_POINT ( 'NONE', #22790 ) ;
#87659 = DIRECTION ( 'NONE',  ( 0.000000000000000000, 0.000000000000000000, -1.000000000000000000 ) ) ;
#87660 = DIRECTION ( 'NONE',  ( 0.000000000000000000, -0.9999939076577903929, 0.003490651415223739937 ) ) ;
#87661 = EDGE_CURVE ( 'NONE', #59275, #62448, #100489, .T. ) ;
#87664 = ORIENTED_EDGE ( 'NONE', *, *, #43518, .T. ) ;
#87663 = CONICAL_SURFACE ( 'NONE', #31259, 0.09999999999999982514, 0.003490658503988666988 ) ;
#87662 = AXIS2_PLACEMENT_3D ( 'NONE', #109049, #80912, #10236 ) ;
#87665 = LINE ( 'NONE', #36666, #65216 ) ;
#87666 = CARTESIAN_POINT ( 'NONE',  ( -4.800000000000028244, 2.500000000000000000, -3.983716857408426293 ) ) ;
#87667 = ORIENTED_EDGE ( 'NONE', *, *, #87414, .T. ) ;
#87668 = ADVANCED_FACE ( 'NONE', ( #24063 ), #75091, .T. ) ;
#87669 = ADVANCED_FACE ( 'NONE', ( #114994 ), #72527, .T. ) ;
#87670 = ADVANCED_FACE ( 'NONE', ( #12921 ), #62705, .T. ) ;
#87671 = CARTESIAN_POINT ( 'NONE',  ( -13.54999999999999005, 12.50000000000000000, 2.576566944158914740 ) ) ;
#87672 = EDGE_CURVE ( 'NONE', #97290, #3112, #102606, .T. ) ;
#87673 = DIRECTION ( 'NONE',  ( 0.000000000000000000, 0.000000000000000000, 1.000000000000000000 ) ) ;
#87674 = EDGE_LOOP ( 'NONE', ( #69721, #77518 ) ) ;
#87675 = EDGE_LOOP ( 'NONE', ( #54281, #35860 ) ) ;
#87677 = ORIENTED_EDGE ( 'NONE', *, *, #118219, .F. ) ;
#87676 = ADVANCED_FACE ( 'NONE', ( #14846 ), #87860, .T. ) ;
#87678 = AXIS2_PLACEMENT_3D ( 'NONE', #1615, #122690, #101767 ) ;
#87679 = PLANE ( 'NONE',  #92699 ) ;
#87680 = ADVANCED_FACE ( 'NONE', ( #124193 ), #3136, .T. ) ;
#87681 = EDGE_CURVE ( 'NONE', #33854, #58766, #31459, .T. ) ;
#87682 = DIRECTION ( 'NONE',  ( 0.000000000000000000, 1.000000000000000000, 0.000000000000000000 ) ) ;
#87683 = EDGE_CURVE ( 'NONE', #61095, #113875, #5045, .T. ) ;
#87684 = CIRCLE ( 'NONE', #83508, 0.09999999999999982514 ) ;
#87685 = ADVANCED_FACE ( 'NONE', ( #43722 ), #35656, .T. ) ;
#87686 = CIRCLE ( 'NONE', #75177, 0.06509327318403745899 ) ;
#87687 = ORIENTED_EDGE ( 'NONE', *, *, #19094, .T. ) ;
#87688 = CARTESIAN_POINT ( 'NONE',  ( -6.250000000000021316, 2.500000000000000000, -1.472243186433550122 ) ) ;
#87689 = DIRECTION ( 'NONE',  ( -0.000000000000000000, 1.000000000000000000, -0.000000000000000000 ) ) ;
#87690 = CARTESIAN_POINT ( 'NONE',  ( 6.649999999999931966, 2.500000000000000000, -7.088010851410853519 ) ) ;
#87691 = CARTESIAN_POINT ( 'NONE',  ( 4.799999999999939426, 12.50000000000000000, -4.741630453620015118 ) ) ;
#87692 = EDGE_CURVE ( 'NONE', #73692, #2801, #94086, .T. ) ;
#87693 = CONICAL_SURFACE ( 'NONE', #104426, 0.1000000000000002554, 0.003490658503988666988 ) ;
#87694 = VECTOR ( 'NONE', #32925, 1000.000000000000000 ) ;
#87695 = ORIENTED_EDGE ( 'NONE', *, *, #83231, .F. ) ;
#87696 = CARTESIAN_POINT ( 'NONE',  ( 8.749999999999953815, 2.500000000000000000, 6.495190528383297135 ) ) ;
#87697 = ORIENTED_EDGE ( 'NONE', *, *, #86954, .T. ) ;
#87698 = VERTEX_POINT ( 'NONE', #114362 ) ;
#87699 = DIRECTION ( 'NONE',  ( 0.000000000000000000, 0.000000000000000000, -1.000000000000000000 ) ) ;
#87700 = FACE_OUTER_BOUND ( 'NONE', #55840, .T. ) ;
#87701 = FACE_BOUND ( 'NONE', #34680, .T. ) ;
#87702 = AXIS2_PLACEMENT_3D ( 'NONE', #61668, #120576, #59748 ) ;
#87703 = CARTESIAN_POINT ( 'NONE',  ( -5.400000000000019895, 2.500000000000000000, -2.276824562219559311E-15 ) ) ;
#87704 = DIRECTION ( 'NONE',  ( 0.000000000000000000, 0.000000000000000000, 1.000000000000000000 ) ) ;
#87705 = DIRECTION ( 'NONE',  ( 0.000000000000000000, 1.000000000000000000, 0.000000000000000000 ) ) ;
#87706 = AXIS2_PLACEMENT_3D ( 'NONE', #108787, #106851, #68869 ) ;
#87707 = ORIENTED_EDGE ( 'NONE', *, *, #98179, .F. ) ;
#87708 = CARTESIAN_POINT ( 'NONE',  ( -16.50000000000000000, 2.500000000000000000, 1.734723475976807094E-15 ) ) ;
#87709 = DIRECTION ( 'NONE',  ( -0.000000000000000000, 1.000000000000000000, -0.000000000000000000 ) ) ;
#87710 = CARTESIAN_POINT ( 'NONE',  ( -6.450000000000016165, 12.50000000000000000, 6.841600689897072485 ) ) ;
#87711 = CARTESIAN_POINT ( 'NONE',  ( 6.049999999999932321, 12.50000000000000000, 6.906693963081109722 ) ) ;
#87712 = ORIENTED_EDGE ( 'NONE', *, *, #11830, .F. ) ;
#87713 = CARTESIAN_POINT ( 'NONE',  ( 3.749999999999938716, 2.500000000000000000, 7.188010851410848723 ) ) ;
#87714 = DIRECTION ( 'NONE',  ( 0.000000000000000000, -0.9999939076577903929, 0.003490651415223739937 ) ) ;
#87715 = CIRCLE ( 'NONE', #129615, 0.06509327318403745899 ) ;
#87716 = VERTEX_POINT ( 'NONE', #63338 ) ;
#87717 = ORIENTED_EDGE ( 'NONE', *, *, #84258, .F. ) ;
#87718 = CARTESIAN_POINT ( 'NONE',  ( -5.650000000000023448, 2.500000000000000000, -1.818653347947326138 ) ) ;
#87719 = CARTESIAN_POINT ( 'NONE',  ( 12.89999999999990266, 2.500000000000000000, -5.022947341949754119 ) ) ;
#87720 = FACE_BOUND ( 'NONE', #2493, .T. ) ;
#87721 = DIRECTION ( 'NONE',  ( 0.000000000000000000, 1.000000000000000000, 0.000000000000000000 ) ) ;
#87722 = ADVANCED_FACE ( 'NONE', ( #103270 ), #127, .T. ) ;
#87723 = ORIENTED_EDGE ( 'NONE', *, *, #58613, .F. ) ;
#87724 = DIRECTION ( 'NONE',  ( 0.000000000000000000, 0.000000000000000000, 1.000000000000000000 ) ) ;
#87725 = ADVANCED_FACE ( 'NONE', ( #34545 ), #62843, .T. ) ;
#87726 = ORIENTED_EDGE ( 'NONE', *, *, #81293, .F. ) ;
#87727 = ORIENTED_EDGE ( 'NONE', *, *, #64001, .F. ) ;
#87728 = FACE_OUTER_BOUND ( 'NONE', #4725, .T. ) ;
#87729 = CARTESIAN_POINT ( 'NONE',  ( 187.5000000000000000, 0.000000000000000000, 7.700000000000000178 ) ) ;
#87730 = ORIENTED_EDGE ( 'NONE', *, *, #47624, .F. ) ;
#87731 = CARTESIAN_POINT ( 'NONE',  ( -12.89999999999999147, 12.50000000000000000, -0.7579135962115874925 ) ) ;
#87732 = CARTESIAN_POINT ( 'NONE',  ( 9.999999999999916511, 2.500000000000000000, -0.6928203230275541413 ) ) ;
#87733 = EDGE_CURVE ( 'NONE', #47201, #98668, #113008, .T. ) ;
#87734 = CARTESIAN_POINT ( 'NONE',  ( 3.749999999999975131, 2.500000000000000000, 6.495190528383297135 ) ) ;
#87735 = AXIS2_PLACEMENT_3D ( 'NONE', #31944, #33243, #92126 ) ;
#87736 = LINE ( 'NONE', #59612, #17523 ) ;
#87737 = ORIENTED_EDGE ( 'NONE', *, *, #120909, .F. ) ;
#87738 = CARTESIAN_POINT ( 'NONE',  ( 9.999999999999912959, 12.50000000000000000, 3.572213422710607489 ) ) ;
#87740 = CONICAL_SURFACE ( 'NONE', #60595, 0.1000000000000002554, 0.003490658503988666988 ) ;
#87739 = CONICAL_SURFACE ( 'NONE', #50126, 0.1000000000000002554, 0.003490658503988666988 ) ;
#87741 = CARTESIAN_POINT ( 'NONE',  ( 12.29999999999990479, 2.500000000000000000, 4.676537180435972552 ) ) ;
#87742 = CARTESIAN_POINT ( 'NONE',  ( -11.44999999999999751, 12.50000000000000000, -6.906693963081111498 ) ) ;
#87743 = DIRECTION ( 'NONE',  ( -0.000000000000000000, 1.000000000000000000, -0.000000000000000000 ) ) ;
#87744 = VECTOR ( 'NONE', #107567, 1000.000000000000000 ) ;
#87745 = ORIENTED_EDGE ( 'NONE', *, *, #28870, .T. ) ;
#87746 = LINE ( 'NONE', #20799, #35015 ) ;
#87747 = ORIENTED_EDGE ( 'NONE', *, *, #38543, .T. ) ;
#87748 = DIRECTION ( 'NONE',  ( 0.000000000000000000, 0.000000000000000000, 1.000000000000000000 ) ) ;
#87749 = ORIENTED_EDGE ( 'NONE', *, *, #59949, .F. ) ;
#87750 = DIRECTION ( 'NONE',  ( 0.000000000000000000, 1.000000000000000000, 0.000000000000000000 ) ) ;
#87753 = CARTESIAN_POINT ( 'NONE',  ( 17.50000000000000000, -2.499999999999999556, 2.666666666666670515 ) ) ;
#87752 = AXIS2_PLACEMENT_3D ( 'NONE', #128958, #26865, #58908 ) ;
#87751 = AXIS2_PLACEMENT_3D ( 'NONE', #2835, #42793, #82703 ) ;
#87754 = DIRECTION ( 'NONE',  ( 0.000000000000000000, 0.000000000000000000, 1.000000000000000000 ) ) ;
#87755 = DIRECTION ( 'NONE',  ( 0.000000000000000000, -0.000000000000000000, 1.000000000000000000 ) ) ;
#87756 = EDGE_LOOP ( 'NONE', ( #99547, #24154, #68998, #46844 ) ) ;
#87757 = LINE ( 'NONE', #9209, #18227 ) ;
#87758 = CARTESIAN_POINT ( 'NONE',  ( 10.79999999999991012, 2.500000000000000000, -4.330127018922201643 ) ) ;
#87759 = DIRECTION ( 'NONE',  ( 0.000000000000000000, 0.000000000000000000, 1.000000000000000000 ) ) ;
#87760 = CARTESIAN_POINT ( 'NONE',  ( 0.8499999999999557909, 12.50000000000000000, -7.188010851410854052 ) ) ;
#87761 = LINE ( 'NONE', #48498, #112194 ) ;
#87762 = EDGE_CURVE ( 'NONE', #58821, #58767, #116285, .T. ) ;
#87763 = ORIENTED_EDGE ( 'NONE', *, *, #100698, .T. ) ;
#87764 = ORIENTED_EDGE ( 'NONE', *, *, #43979, .F. ) ;
#87765 = DIRECTION ( 'NONE',  ( 0.000000000000000000, 0.000000000000000000, -1.000000000000000000 ) ) ;
#87766 = ORIENTED_EDGE ( 'NONE', *, *, #24840, .T. ) ;
#87767 = DIRECTION ( 'NONE',  ( 0.000000000000000000, -0.9999939076577903929, 0.003490651415223739937 ) ) ;
#87769 = ORIENTED_EDGE ( 'NONE', *, *, #39887, .F. ) ;
#87768 = VERTEX_POINT ( 'NONE', #96018 ) ;
#87770 = ORIENTED_EDGE ( 'NONE', *, *, #123422, .T. ) ;
#87771 = DIRECTION ( 'NONE',  ( 0.000000000000000000, -0.000000000000000000, 1.000000000000000000 ) ) ;
#87772 = CONICAL_SURFACE ( 'NONE', #106556, 0.1000000000000000056, 0.003490658503988666988 ) ;
#87773 = DIRECTION ( 'NONE',  ( 0.000000000000000000, 1.000000000000000000, 0.000000000000000000 ) ) ;
#87774 = CIRCLE ( 'NONE', #33514, 0.06509327318403745899 ) ;
#87775 = CARTESIAN_POINT ( 'NONE',  ( 3.749999999999978684, 12.50000000000000000, -2.165063509461101710 ) ) ;
#87776 = CARTESIAN_POINT ( 'NONE',  ( -7.300000000000018474, 2.500000000000000000, -3.983716857408426293 ) ) ;
#87777 = DIRECTION ( 'NONE',  ( 0.000000000000000000, -0.9999939076577903929, 0.003490651415223739937 ) ) ;
#87778 = EDGE_CURVE ( 'NONE', #59465, #125538, #65248, .T. ) ;
#87779 = CARTESIAN_POINT ( 'NONE',  ( 14.19999999999989626, 2.500000000000000000, -2.276824562219559311E-15 ) ) ;
#87780 = LINE ( 'NONE', #4867, #36370 ) ;
#87781 = ADVANCED_FACE ( 'NONE', ( #65904 ), #85806, .T. ) ;
#87783 = AXIS2_PLACEMENT_3D ( 'NONE', #85606, #125529, #35872 ) ;
#87782 = DIRECTION ( 'NONE',  ( 0.000000000000000000, 0.000000000000000000, 1.000000000000000000 ) ) ;
#87784 = ORIENTED_EDGE ( 'NONE', *, *, #5693, .F. ) ;
#87785 = ORIENTED_EDGE ( 'NONE', *, *, #8627, .T. ) ;
#87786 = VERTEX_POINT ( 'NONE', #26000 ) ;
#87787 = ORIENTED_EDGE ( 'NONE', *, *, #81441, .F. ) ;
#87788 = DIRECTION ( 'NONE',  ( -0.000000000000000000, -1.000000000000000000, -0.000000000000000000 ) ) ;
#87789 = ORIENTED_EDGE ( 'NONE', *, *, #116613, .T. ) ;
#87790 = ADVANCED_FACE ( 'NONE', ( #105187 ), #88098, .T. ) ;
#87791 = EDGE_LOOP ( 'NONE', ( #38663, #112908, #123107, #6402 ) ) ;
#87792 = VECTOR ( 'NONE', #120274, 1000.000000000000000 ) ;
#87793 = CIRCLE ( 'NONE', #16674, 0.1000000000000000472 ) ;
#87794 = DIRECTION ( 'NONE',  ( 0.000000000000000000, 1.000000000000000000, 0.000000000000000000 ) ) ;
#87795 = DIRECTION ( 'NONE',  ( 0.000000000000000000, 0.000000000000000000, -1.000000000000000000 ) ) ;
#87796 = CIRCLE ( 'NONE', #31395, 0.1000000000000000472 ) ;
#87797 = CARTESIAN_POINT ( 'NONE',  ( -10.00000000000000355, 2.500000000000000000, -0.5928203230275541635 ) ) ;
#87798 = DIRECTION ( 'NONE',  ( -0.000000000000000000, -1.000000000000000000, -0.000000000000000000 ) ) ;
#87799 = DIRECTION ( 'NONE',  ( 0.000000000000000000, 0.000000000000000000, -1.000000000000000000 ) ) ;
#87800 = ORIENTED_EDGE ( 'NONE', *, *, #48262, .F. ) ;
#87801 = CARTESIAN_POINT ( 'NONE',  ( -0.6500000000000394351, 2.500000000000000000, 2.611473670974873151 ) ) ;
#87802 = AXIS2_PLACEMENT_3D ( 'NONE', #75307, #7199, #115203 ) ;
#87803 = VERTEX_POINT ( 'NONE', #27921 ) ;
#87804 = DIRECTION ( 'NONE',  ( -0.000000000000000000, 1.000000000000000000, -0.000000000000000000 ) ) ;
#87805 = ORIENTED_EDGE ( 'NONE', *, *, #106790, .F. ) ;
#87806 = CARTESIAN_POINT ( 'NONE',  ( 10.84999999999990905, 2.500000000000000000, 1.572243186433545548 ) ) ;
#87807 = CIRCLE ( 'NONE', #104551, 0.1000000000000000472 ) ;
#87808 = VERTEX_POINT ( 'NONE', #115643 ) ;
#87809 = VERTEX_POINT ( 'NONE', #8269 ) ;
#87810 = PLANE ( 'NONE',  #56562 ) ;
#87811 = DIRECTION ( 'NONE',  ( -0.000000000000000000, -1.000000000000000000, -0.000000000000000000 ) ) ;
#87812 = ADVANCED_FACE ( 'NONE', ( #16141 ), #126774, .T. ) ;
#87813 = CARTESIAN_POINT ( 'NONE',  ( -13.34999999999999076, 12.50000000000000000, 2.165063509461101265 ) ) ;
#87814 = DIRECTION ( 'NONE',  ( -4.274815082592931898E-19, -0.9999939076577903929, -0.003490651415223739937 ) ) ;
#87815 = DIRECTION ( 'NONE',  ( 0.000000000000000000, 0.000000000000000000, 1.000000000000000000 ) ) ;
#87816 = EDGE_LOOP ( 'NONE', ( #65312, #12630 ) ) ;
#87817 = CARTESIAN_POINT ( 'NONE',  ( 0.8499999999999553468, 2.500000000000000000, -2.165063509461101710 ) ) ;
#87818 = DIRECTION ( 'NONE',  ( 0.000000000000000000, -0.000000000000000000, 1.000000000000000000 ) ) ;
#87819 = ADVANCED_FACE ( 'NONE', ( #55450 ), #16831, .T. ) ;
#87820 = DIRECTION ( 'NONE',  ( 0.000000000000000000, -0.9999939076577903929, 0.003490651415223739937 ) ) ;
#87821 = CARTESIAN_POINT ( 'NONE',  ( -0.8500000000000382805, 12.50000000000000000, -7.188010851410854052 ) ) ;
#87822 = EDGE_CURVE ( 'NONE', #35339, #10073, #27266, .T. ) ;
#87823 = DIRECTION ( 'NONE',  ( 0.000000000000000000, 1.000000000000000000, 0.000000000000000000 ) ) ;
#87824 = VERTEX_POINT ( 'NONE', #128059 ) ;
#87825 = ORIENTED_EDGE ( 'NONE', *, *, #88281, .T. ) ;
#87826 = EDGE_CURVE ( 'NONE', #101170, #59036, #220, .T. ) ;
#87827 = CIRCLE ( 'NONE', #31417, 0.06509327318403743123 ) ;
#87828 = EDGE_CURVE ( 'NONE', #117628, #80777, #37799, .T. ) ;
#87829 = FACE_OUTER_BOUND ( 'NONE', #14569, .T. ) ;
#87830 = VECTOR ( 'NONE', #116277, 1000.000000000000000 ) ;
#87831 = EDGE_CURVE ( 'NONE', #78070, #74183, #67097, .T. ) ;
#87832 = ORIENTED_EDGE ( 'NONE', *, *, #87112, .F. ) ;
#87833 = DIRECTION ( 'NONE',  ( -0.000000000000000000, -1.000000000000000000, -0.000000000000000000 ) ) ;
#87834 = FACE_OUTER_BOUND ( 'NONE', #63510, .T. ) ;
#87837 = EDGE_CURVE ( 'NONE', #49637, #69423, #23213, .T. ) ;
#87836 = CIRCLE ( 'NONE', #8418, 0.1000000000000002554 ) ;
#87835 = AXIS2_PLACEMENT_3D ( 'NONE', #70311, #2193, #59216 ) ;
#87838 = ORIENTED_EDGE ( 'NONE', *, *, #15453, .T. ) ;
#87839 = CARTESIAN_POINT ( 'NONE',  ( 186.2500000000000000, 9.429780353434619030E-16, -7.700000000000000178 ) ) ;
#87840 = CARTESIAN_POINT ( 'NONE',  ( 9.149999999999920419, 12.50000000000000000, 2.922977105672686982 ) ) ;
#87841 = EDGE_CURVE ( 'NONE', #116200, #76636, #39953, .T. ) ;
#87842 = CARTESIAN_POINT ( 'NONE',  ( -15.39999999999997904, 12.50000000000000000, 0.000000000000000000 ) ) ;
#87843 = CARTESIAN_POINT ( 'NONE',  ( -6.050000000000020250, 12.50000000000000000, -6.841600689897078702 ) ) ;
#87844 = ORIENTED_EDGE ( 'NONE', *, *, #78238, .T. ) ;
#87845 = EDGE_CURVE ( 'NONE', #59380, #37927, #98419, .T. ) ;
#87846 = DIRECTION ( 'NONE',  ( 0.000000000000000000, -0.000000000000000000, 1.000000000000000000 ) ) ;
#87847 = DIRECTION ( 'NONE',  ( 0.000000000000000000, 0.000000000000000000, 1.000000000000000000 ) ) ;
#87848 = EDGE_LOOP ( 'NONE', ( #53061, #116412, #111910, #32092 ) ) ;
#87849 = CARTESIAN_POINT ( 'NONE',  ( 2.899999999999946620, 2.500000000000000000, -0.6928203230275542523 ) ) ;
#87850 = DIRECTION ( 'NONE',  ( -0.000000000000000000, 1.000000000000000000, -0.000000000000000000 ) ) ;
#87851 = CARTESIAN_POINT ( 'NONE',  ( 11.89999999999990798, 2.500000000000000000, -4.676537180435977881 ) ) ;
#87852 = ORIENTED_EDGE ( 'NONE', *, *, #104492, .T. ) ;
#87853 = CARTESIAN_POINT ( 'NONE',  ( 4.999999999999933387, 12.50000000000000000, 5.022947341949748790 ) ) ;
#87854 = VERTEX_POINT ( 'NONE', #37747 ) ;
#87855 = DIRECTION ( 'NONE',  ( 0.000000000000000000, 0.000000000000000000, -1.000000000000000000 ) ) ;
#87856 = DIRECTION ( 'NONE',  ( 0.000000000000000000, 1.000000000000000000, 0.000000000000000000 ) ) ;
#87857 = DIRECTION ( 'NONE',  ( -0.000000000000000000, -1.000000000000000000, -0.000000000000000000 ) ) ;
#87858 = EDGE_LOOP ( 'NONE', ( #32826, #14962, #109191, #117251 ) ) ;
#87859 = DIRECTION ( 'NONE',  ( 0.000000000000000000, 0.000000000000000000, -1.000000000000000000 ) ) ;
#87860 = CONICAL_SURFACE ( 'NONE', #12650, 0.09999999999999982514, 0.003490658503988666988 ) ;
#87861 = CARTESIAN_POINT ( 'NONE',  ( 0.1999999999999562961, 2.500000000000000000, 4.676537180435972552 ) ) ;
#87862 = VERTEX_POINT ( 'NONE', #96635 ) ;
#87863 = DIRECTION ( 'NONE',  ( -0.000000000000000000, 1.000000000000000000, -0.000000000000000000 ) ) ;
#87864 = VERTEX_POINT ( 'NONE', #46937 ) ;
#87865 = CONICAL_SURFACE ( 'NONE', #54430, 0.1000000000000002554, 0.003490658503988666988 ) ;
#87866 = DIRECTION ( 'NONE',  ( 0.000000000000000000, 0.000000000000000000, 1.000000000000000000 ) ) ;
#87867 = ADVANCED_FACE ( 'NONE', ( #107109 ), #16921, .T. ) ;
#87868 = ORIENTED_EDGE ( 'NONE', *, *, #120752, .F. ) ;
#87869 = DIRECTION ( 'NONE',  ( 0.000000000000000000, -0.000000000000000000, 1.000000000000000000 ) ) ;
#87870 = DIRECTION ( 'NONE',  ( 0.000000000000000000, 0.000000000000000000, 1.000000000000000000 ) ) ;
#87871 = EDGE_CURVE ( 'NONE', #47911, #27024, #35744, .T. ) ;
#87872 = VERTEX_POINT ( 'NONE', #127416 ) ;
#87873 = EDGE_LOOP ( 'NONE', ( #92413, #567, #90140, #95068 ) ) ;
#87874 = CARTESIAN_POINT ( 'NONE',  ( 5.599999999999934808, 2.500000000000000000, -4.676537180435978769 ) ) ;
#87875 = DIRECTION ( 'NONE',  ( 0.000000000000000000, 0.000000000000000000, 1.000000000000000000 ) ) ;
#87876 = ORIENTED_EDGE ( 'NONE', *, *, #812, .F. ) ;
#87878 = FACE_OUTER_BOUND ( 'NONE', #112170, .T. ) ;
#87877 = CIRCLE ( 'NONE', #79502, 0.06509327318403745899 ) ;
#87879 = DIRECTION ( 'NONE',  ( 0.000000000000000000, 0.000000000000000000, -1.000000000000000000 ) ) ;
#87880 = AXIS2_PLACEMENT_3D ( 'NONE', #5749, #84973, #96086 ) ;
#87881 = DIRECTION ( 'NONE',  ( 0.000000000000000000, 0.000000000000000000, 1.000000000000000000 ) ) ;
#87882 = DIRECTION ( 'NONE',  ( 0.000000000000000000, 0.000000000000000000, 1.000000000000000000 ) ) ;
#87883 = CARTESIAN_POINT ( 'NONE',  ( 0.000000000000000000, 0.000000000000000000, -5.000000000000004441 ) ) ;
#87884 = DIRECTION ( 'NONE',  ( -0.000000000000000000, 1.000000000000000000, -0.000000000000000000 ) ) ;
#87885 = CIRCLE ( 'NONE', #71179, 0.06509327318403745899 ) ;
#87886 = VERTEX_POINT ( 'NONE', #71070 ) ;
#87887 = VERTEX_POINT ( 'NONE', #61258 ) ;
#87888 = ORIENTED_EDGE ( 'NONE', *, *, #10373, .F. ) ;
#87889 = ORIENTED_EDGE ( 'NONE', *, *, #64689, .T. ) ;
#87890 = AXIS2_PLACEMENT_3D ( 'NONE', #107043, #47502, #17364 ) ;
#87891 = LINE ( 'NONE', #19147, #110171 ) ;
#87892 = CARTESIAN_POINT ( 'NONE',  ( -6.650000000000018119, 2.500000000000000000, -2.065063509461102065 ) ) ;
#87893 = FACE_OUTER_BOUND ( 'NONE', #97218, .T. ) ;
#87894 = EDGE_LOOP ( 'NONE', ( #47636, #96519, #110506, #58427 ) ) ;
#87895 = FACE_BOUND ( 'NONE', #95982, .T. ) ;
#87896 = ORIENTED_EDGE ( 'NONE', *, *, #99973, .T. ) ;
#87897 = CARTESIAN_POINT ( 'NONE',  ( 6.699999999999930012, 12.50000000000000000, -4.330127018922201643 ) ) ;
#87898 = CARTESIAN_POINT ( 'NONE',  ( 6.899999999999926636, 2.500000000000000000, -0.3464101615137782364 ) ) ;
#87899 = FACE_OUTER_BOUND ( 'NONE', #48552, .T. ) ;
#87900 = DIRECTION ( 'NONE',  ( 0.000000000000000000, 0.000000000000000000, 1.000000000000000000 ) ) ;
#87901 = DIRECTION ( 'NONE',  ( -0.000000000000000000, 1.000000000000000000, -0.000000000000000000 ) ) ;
#87902 = CARTESIAN_POINT ( 'NONE',  ( 9.599999999999914380, 2.500000000000000000, 4.230127018922196669 ) ) ;
#87903 = EDGE_LOOP ( 'NONE', ( #56060, #67382 ) ) ;
#87904 = CARTESIAN_POINT ( 'NONE',  ( -12.89999999999999147, 12.50000000000000000, 4.265033745738159077 ) ) ;
#87905 = CARTESIAN_POINT ( 'NONE',  ( 4.199999999999939782, 2.500000000000000000, 0.09999999999999772959 ) ) ;
#87906 = FACE_OUTER_BOUND ( 'NONE', #71032, .T. ) ;
#87907 = ADVANCED_FACE ( 'NONE', ( #371 ), #104682, .T. ) ;
#87908 = ORIENTED_EDGE ( 'NONE', *, *, #36147, .T. ) ;
#87909 = ORIENTED_EDGE ( 'NONE', *, *, #47485, .T. ) ;
#87910 = ORIENTED_EDGE ( 'NONE', *, *, #5794, .T. ) ;
#87911 = EDGE_LOOP ( 'NONE', ( #60163, #85222, #23897, #33037 ) ) ;
#87912 = CARTESIAN_POINT ( 'NONE',  ( 16.96615051717151701, -1.026750547570780547, -5.590381354654383017 ) ) ;
#87913 = VECTOR ( 'NONE', #65741, 1000.000000000000000 ) ;
#87914 = CARTESIAN_POINT ( 'NONE',  ( 4.149999999999941735, 12.50000000000000000, -1.472243186433550122 ) ) ;
#87915 = VECTOR ( 'NONE', #88087, 1000.000000000000000 ) ;
#87917 = ORIENTED_EDGE ( 'NONE', *, *, #114046, .T. ) ;
#87916 = ORIENTED_EDGE ( 'NONE', *, *, #41582, .F. ) ;
#87918 = VERTEX_POINT ( 'NONE', #120812 ) ;
#87919 = DIRECTION ( 'NONE',  ( 0.000000000000000000, 0.000000000000000000, -1.000000000000000000 ) ) ;
#87920 = EDGE_CURVE ( 'NONE', #89608, #49421, #14773, .T. ) ;
#87921 = DIRECTION ( 'NONE',  ( 0.000000000000000000, 1.000000000000000000, 0.000000000000000000 ) ) ;
#87922 = CARTESIAN_POINT ( 'NONE',  ( -5.600000000000020073, 2.500000000000000000, 0.2464101615137736789 ) ) ;
#87923 = FACE_OUTER_BOUND ( 'NONE', #84165, .T. ) ;
#87924 = DIRECTION ( 'NONE',  ( 0.000000000000000000, 0.000000000000000000, -1.000000000000000000 ) ) ;
#87925 = CARTESIAN_POINT ( 'NONE',  ( 1.249999999999952482, 2.500000000000000000, -5.802370205355749988 ) ) ;
#87927 = EDGE_CURVE ( 'NONE', #126243, #1900, #87948, .T. ) ;
#87926 = CIRCLE ( 'NONE', #104653, 0.09999999999999982514 ) ;
#87928 = CARTESIAN_POINT ( 'NONE',  ( 8.099999999999921485, 12.50000000000000000, -0.3464101615137783474 ) ) ;
#87929 = EDGE_CURVE ( 'NONE', #39515, #49457, #29858, .T. ) ;
#87930 = ORIENTED_EDGE ( 'NONE', *, *, #72533, .T. ) ;
#87931 = DIRECTION ( 'NONE',  ( 0.000000000000000000, 0.000000000000000000, -1.000000000000000000 ) ) ;
#87932 = ORIENTED_EDGE ( 'NONE', *, *, #103478, .T. ) ;
#87933 = EDGE_LOOP ( 'NONE', ( #79042, #99186 ) ) ;
#87934 = ORIENTED_EDGE ( 'NONE', *, *, #79108, .F. ) ;
#87935 = EDGE_CURVE ( 'NONE', #87786, #118224, #4408, .T. ) ;
#87936 = FACE_OUTER_BOUND ( 'NONE', #62019, .T. ) ;
#87937 = ORIENTED_EDGE ( 'NONE', *, *, #109543, .F. ) ;
#87938 = EDGE_CURVE ( 'NONE', #40642, #129526, #52458, .T. ) ;
#87939 = ORIENTED_EDGE ( 'NONE', *, *, #64327, .T. ) ;
#87940 = LINE ( 'NONE', #96472, #96643 ) ;
#87941 = DIRECTION ( 'NONE',  ( 0.000000000000000000, 0.000000000000000000, 1.000000000000000000 ) ) ;
#87942 = LINE ( 'NONE', #56557, #20673 ) ;
#87943 = DIRECTION ( 'NONE',  ( -0.000000000000000000, -1.000000000000000000, -0.000000000000000000 ) ) ;
#87944 = FACE_OUTER_BOUND ( 'NONE', #31582, .T. ) ;
#87945 = VERTEX_POINT ( 'NONE', #20048 ) ;
#87946 = CARTESIAN_POINT ( 'NONE',  ( -0.2000000000000408673, 2.500000000000000000, -3.983716857408426293 ) ) ;
#87947 = CONICAL_SURFACE ( 'NONE', #110939, 0.09999999999999982514, 0.003490658503988666988 ) ;
#87948 = CIRCLE ( 'NONE', #94229, 0.1000000000000000472 ) ;
#87949 = EDGE_LOOP ( 'NONE', ( #94799, #102039, #39564, #14831 ) ) ;
#87950 = CARTESIAN_POINT ( 'NONE',  ( -1.050000000000037792, 12.50000000000000000, 6.148780366869520009 ) ) ;
#87951 = ORIENTED_EDGE ( 'NONE', *, *, #63810, .T. ) ;
#87952 = CARTESIAN_POINT ( 'NONE',  ( 111.7561744588909676, 8.047232822298814980, -3.315531987436182604 ) ) ;
#87953 = DIRECTION ( 'NONE',  ( -0.000000000000000000, -1.000000000000000000, -0.000000000000000000 ) ) ;
#87954 = EDGE_LOOP ( 'NONE', ( #3166, #42107 ) ) ;
#87955 = LINE ( 'NONE', #99102, #105175 ) ;
#87956 = CARTESIAN_POINT ( 'NONE',  ( 1.449999999999951772, 2.500000000000000000, -6.148780366869526226 ) ) ;
#87957 = ORIENTED_EDGE ( 'NONE', *, *, #1690, .F. ) ;
#87958 = AXIS2_PLACEMENT_3D ( 'NONE', #128119, #7026, #28635 ) ;
#87959 = CIRCLE ( 'NONE', #37809, 0.06509327318403745899 ) ;
#87960 = EDGE_CURVE ( 'NONE', #53806, #101537, #56645, .T. ) ;
#87961 = DIRECTION ( 'NONE',  ( 0.000000000000000000, 0.000000000000000000, 1.000000000000000000 ) ) ;
#87962 = ORIENTED_EDGE ( 'NONE', *, *, #107036, .F. ) ;
#87963 = ORIENTED_EDGE ( 'NONE', *, *, #30771, .T. ) ;
#87964 = CARTESIAN_POINT ( 'NONE',  ( -5.200000000000025935, 12.50000000000000000, -3.918623584224389056 ) ) ;
#87965 = DIRECTION ( 'NONE',  ( -0.000000000000000000, -1.000000000000000000, -0.000000000000000000 ) ) ;
#87966 = ADVANCED_FACE ( 'NONE', ( #99893 ), #115130, .T. ) ;
#87967 = CARTESIAN_POINT ( 'NONE',  ( 185.3802083336747160, 4.367472073101515306, 7.564683531250000925 ) ) ;
#87968 = FACE_OUTER_BOUND ( 'NONE', #30503, .T. ) ;
#87969 = EDGE_CURVE ( 'NONE', #127557, #103729, #110940, .T. ) ;
#87970 = AXIS2_PLACEMENT_3D ( 'NONE', #83678, #32019, #82410 ) ;
#87971 = CIRCLE ( 'NONE', #100508, 0.1000000000000002554 ) ;
#87972 = DIRECTION ( 'NONE',  ( 0.000000000000000000, -0.000000000000000000, 1.000000000000000000 ) ) ;
#87973 = DIRECTION ( 'NONE',  ( 0.000000000000000000, 1.000000000000000000, 0.000000000000000000 ) ) ;
#87974 = EDGE_CURVE ( 'NONE', #117851, #110872, #127673, .T. ) ;
#87975 = EDGE_CURVE ( 'NONE', #108330, #71667, #62930, .T. ) ;
#87976 = ADVANCED_FACE ( 'NONE', ( #59342 ), #21159, .T. ) ;
#87978 = EDGE_CURVE ( 'NONE', #85590, #17533, #32635, .T. ) ;
#87977 = CONICAL_SURFACE ( 'NONE', #33630, 0.09999999999999982514, 0.003490658503988666988 ) ;
#87979 = VERTEX_POINT ( 'NONE', #129372 ) ;
#87980 = DIRECTION ( 'NONE',  ( 0.000000000000000000, 0.000000000000000000, 1.000000000000000000 ) ) ;
#87981 = CARTESIAN_POINT ( 'NONE',  ( 13.34999999999989662, 2.500000000000000000, -1.572243186433550211 ) ) ;
#87982 = ORIENTED_EDGE ( 'NONE', *, *, #84271, .F. ) ;
#87983 = ADVANCED_FACE ( 'NONE', ( #11503 ), #2278, .T. ) ;
#87984 = DIRECTION ( 'NONE',  ( 0.000000000000000000, 1.000000000000000000, 0.000000000000000000 ) ) ;
#87985 = LINE ( 'NONE', #36980, #115758 ) ;
#87986 = CARTESIAN_POINT ( 'NONE',  ( -8.150000000000009237, 12.50000000000000000, 6.148780366869520009 ) ) ;
#87987 = DIRECTION ( 'NONE',  ( 0.000000000000000000, 0.000000000000000000, 1.000000000000000000 ) ) ;
#87988 = CARTESIAN_POINT ( 'NONE',  ( 14.34999999999989662, 2.500000000000000000, 1.918653347947321564 ) ) ;
#87989 = ORIENTED_EDGE ( 'NONE', *, *, #63688, .T. ) ;
#87990 = EDGE_CURVE ( 'NONE', #110679, #55365, #64974, .T. ) ;
#87991 = ADVANCED_FACE ( 'NONE', ( #60623 ), #81634, .T. ) ;
#87992 = FACE_OUTER_BOUND ( 'NONE', #56399, .T. ) ;
#87993 =( LENGTH_UNIT ( ) NAMED_UNIT ( * ) SI_UNIT ( .MILLI., .METRE. ) );
#87994 = ORIENTED_EDGE ( 'NONE', *, *, #18216, .F. ) ;
#87995 = FACE_OUTER_BOUND ( 'NONE', #129485, .T. ) ;
#87996 = ORIENTED_EDGE ( 'NONE', *, *, #125569, .T. ) ;
#87997 = ORIENTED_EDGE ( 'NONE', *, *, #59596, .T. ) ;
#87998 = FACE_OUTER_BOUND ( 'NONE', #39487, .T. ) ;
#87999 = AXIS2_PLACEMENT_3D ( 'NONE', #38904, #87943, #78814 ) ;
#88000 = EDGE_LOOP ( 'NONE', ( #42999, #54419, #56933, #35723 ) ) ;
#88001 = PLANE ( 'NONE',  #27671 ) ;
#88002 = DIRECTION ( 'NONE',  ( 0.000000000000000000, 1.000000000000000000, 0.000000000000000000 ) ) ;
#88003 = CARTESIAN_POINT ( 'NONE',  ( -15.79999999999998117, 12.50000000000000000, 0.06509327318403743123 ) ) ;
#88004 = ORIENTED_EDGE ( 'NONE', *, *, #85274, .F. ) ;
#88005 = DIRECTION ( 'NONE',  ( -0.000000000000000000, 1.000000000000000000, -0.000000000000000000 ) ) ;
#88007 = ORIENTED_EDGE ( 'NONE', *, *, #97448, .T. ) ;
#88006 = DIRECTION ( 'NONE',  ( 0.000000000000000000, 0.000000000000000000, -1.000000000000000000 ) ) ;
#88008 = CIRCLE ( 'NONE', #119413, 0.06509327318403745899 ) ;
#88009 = PLANE ( 'NONE',  #10951 ) ;
#88010 = LINE ( 'NONE', #88686, #4882 ) ;
#88011 = ORIENTED_EDGE ( 'NONE', *, *, #13563, .T. ) ;
#88013 = VERTEX_POINT ( 'NONE', #93931 ) ;
#88012 = ADVANCED_FACE ( 'NONE', ( #53371 ), #25253, .T. ) ;
#88014 = ORIENTED_EDGE ( 'NONE', *, *, #115763, .T. ) ;
#88015 = CARTESIAN_POINT ( 'NONE',  ( -11.44999999999999929, 2.500000000000000000, -6.248780366869523206 ) ) ;
#88016 = LINE ( 'NONE', #78242, #125281 ) ;
#88017 = LINE ( 'NONE', #58599, #111148 ) ;
#88018 = FACE_BOUND ( 'NONE', #12691, .T. ) ;
#88019 = ORIENTED_EDGE ( 'NONE', *, *, #102173, .F. ) ;
#88020 = CARTESIAN_POINT ( 'NONE',  ( 12.89999999999990266, 12.50000000000000000, 3.702399969078682407 ) ) ;
#88021 = DIRECTION ( 'NONE',  ( 0.000000000000000000, 0.000000000000000000, 1.000000000000000000 ) ) ;
#88022 = EDGE_LOOP ( 'NONE', ( #84199, #123978 ) ) ;
#88023 = EDGE_CURVE ( 'NONE', #84019, #54932, #32468, .T. ) ;
#88024 = CARTESIAN_POINT ( 'NONE',  ( 10.84999999999991260, 12.50000000000000000, -1.407149913249512663 ) ) ;
#88025 = AXIS2_PLACEMENT_3D ( 'NONE', #116417, #7106, #47706 ) ;
#88026 = DIRECTION ( 'NONE',  ( 0.000000000000000000, -0.9999939076577903929, 0.003490651415223739937 ) ) ;
#88027 = CARTESIAN_POINT ( 'NONE',  ( -11.25000000000000000, 12.50000000000000000, -7.188010851410850499 ) ) ;
#88028 = CARTESIAN_POINT ( 'NONE',  ( 12.49999999999990230, 12.50000000000000000, -0.7579135962115916003 ) ) ;
#88029 = DIRECTION ( 'NONE',  ( 0.000000000000000000, 1.000000000000000000, 0.000000000000000000 ) ) ;
#88030 = CARTESIAN_POINT ( 'NONE',  ( 4.999999999999936939, 2.500000000000000000, -3.537306695894649966 ) ) ;
#88031 = CIRCLE ( 'NONE', #94308, 0.1000000000000002554 ) ;
#88032 = CIRCLE ( 'NONE', #44231, 0.1000000000000002554 ) ;
#88033 = ORIENTED_EDGE ( 'NONE', *, *, #9581, .F. ) ;
#88034 = ORIENTED_EDGE ( 'NONE', *, *, #88239, .F. ) ;
#88035 = VERTEX_POINT ( 'NONE', #23242 ) ;
#88036 = ORIENTED_EDGE ( 'NONE', *, *, #17581, .T. ) ;
#88037 = ORIENTED_EDGE ( 'NONE', *, *, #30070, .F. ) ;
#88038 = DIRECTION ( 'NONE',  ( 0.000000000000000000, 0.000000000000000000, 1.000000000000000000 ) ) ;
#88039 = CARTESIAN_POINT ( 'NONE',  ( -9.400000000000007461, 2.500000000000000000, -0.4464101615137783252 ) ) ;
#88040 = ORIENTED_EDGE ( 'NONE', *, *, #55924, .T. ) ;
#88041 = FACE_BOUND ( 'NONE', #13714, .T. ) ;
#88042 = DIRECTION ( 'NONE',  ( 0.000000000000000000, 0.000000000000000000, -1.000000000000000000 ) ) ;
#88043 = CIRCLE ( 'NONE', #2363, 0.06509327318403745899 ) ;
#88044 = CARTESIAN_POINT ( 'NONE',  ( 13.14999999999990088, 2.500000000000000000, 1.818653347947321475 ) ) ;
#88045 = CARTESIAN_POINT ( 'NONE',  ( 13.74999999999989519, 2.500000000000000000, -2.857883832488653741 ) ) ;
#88046 = DIRECTION ( 'NONE',  ( -0.000000000000000000, 1.000000000000000000, -0.000000000000000000 ) ) ;
#88047 = DIRECTION ( 'NONE',  ( 0.000000000000000000, 0.000000000000000000, 1.000000000000000000 ) ) ;
#88048 = VERTEX_POINT ( 'NONE', #112291 ) ;
#88049 = DIRECTION ( 'NONE',  ( 0.000000000000000000, 0.000000000000000000, 1.000000000000000000 ) ) ;
#88050 = AXIS2_PLACEMENT_3D ( 'NONE', #94134, #84314, #115046 ) ;
#88051 = EDGE_LOOP ( 'NONE', ( #88864, #51538, #49310, #16250 ) ) ;
#88052 = CIRCLE ( 'NONE', #79676, 0.1000000000000002554 ) ;
#88053 = VERTEX_POINT ( 'NONE', #123383 ) ;
#88054 = ORIENTED_EDGE ( 'NONE', *, *, #114602, .F. ) ;
#88055 = AXIS2_PLACEMENT_3D ( 'NONE', #7660, #58080, #10258 ) ;
#88056 = DIRECTION ( 'NONE',  ( 0.000000000000000000, 0.000000000000000000, 1.000000000000000000 ) ) ;
#88057 = CARTESIAN_POINT ( 'NONE',  ( -0.8500000000000386136, 12.50000000000000000, 5.737276932171707422 ) ) ;
#88058 = DIRECTION ( 'NONE',  ( -0.000000000000000000, 1.000000000000000000, -0.000000000000000000 ) ) ;
#88059 = ORIENTED_EDGE ( 'NONE', *, *, #33874, .T. ) ;
#88060 = DIRECTION ( 'NONE',  ( 0.000000000000000000, 0.000000000000000000, 1.000000000000000000 ) ) ;
#88061 = AXIS2_PLACEMENT_3D ( 'NONE', #41699, #72437, #111711 ) ;
#88062 = EDGE_CURVE ( 'NONE', #112816, #21177, #18995, .T. ) ;
#88063 = CARTESIAN_POINT ( 'NONE',  ( -12.89999999999999147, 2.500000000000000000, -4.330127018922198978 ) ) ;
#88064 = CARTESIAN_POINT ( 'NONE',  ( -11.44999999999999929, 12.50000000000000000, -6.148780366869522673 ) ) ;
#88065 = AXIS2_PLACEMENT_3D ( 'NONE', #20462, #18518, #58464 ) ;
#88066 = CIRCLE ( 'NONE', #8651, 0.1000000000000000056 ) ;
#88067 = CARTESIAN_POINT ( 'NONE',  ( 186.1093750003413732, 9.264065473108010111E-16, -7.564683531250000925 ) ) ;
#88068 = DIRECTION ( 'NONE',  ( 0.000000000000000000, 0.000000000000000000, -1.000000000000000000 ) ) ;
#88069 = DIRECTION ( 'NONE',  ( 0.000000000000000000, 1.000000000000000000, 0.000000000000000000 ) ) ;
#88070 = ADVANCED_FACE ( 'NONE', ( #71710 ), #69172, .T. ) ;
#88071 = DIRECTION ( 'NONE',  ( -0.000000000000000000, 1.000000000000000000, -0.000000000000000000 ) ) ;
#88072 = ADVANCED_FACE ( 'NONE', ( #113572 ), #43559, .T. ) ;
#88073 = ORIENTED_EDGE ( 'NONE', *, *, #22512, .T. ) ;
#88074 = CARTESIAN_POINT ( 'NONE',  ( -9.400000000000009237, 12.50000000000000000, -4.611443907251936203 ) ) ;
#88075 = EDGE_LOOP ( 'NONE', ( #38453, #23093, #5732, #38538 ) ) ;
#88076 = EDGE_LOOP ( 'NONE', ( #8769, #90342, #73144, #123599 ) ) ;
#88077 = DIRECTION ( 'NONE',  ( 0.000000000000000000, 0.000000000000000000, 1.000000000000000000 ) ) ;
#88078 = ADVANCED_FACE ( 'NONE', ( #82841 ), #46200, .T. ) ;
#88079 = CARTESIAN_POINT ( 'NONE',  ( -7.700000000000014388, 12.50000000000000000, -0.3464101615137782364 ) ) ;
#88080 = DIRECTION ( 'NONE',  ( 0.000000000000000000, 0.000000000000000000, 1.000000000000000000 ) ) ;
#88081 = ADVANCED_FACE ( 'NONE', ( #101822 ), #2977, .F. ) ;
#88082 = ORIENTED_EDGE ( 'NONE', *, *, #32122, .F. ) ;
#88083 = VERTEX_POINT ( 'NONE', #124687 ) ;
#88084 = CARTESIAN_POINT ( 'NONE',  ( 184.9062500006828031, -8.891194145520236347, -1.633285867636356299E-15 ) ) ;
#88085 = CARTESIAN_POINT ( 'NONE',  ( -5.850000000000021849, 12.50000000000000000, -2.857883832488653741 ) ) ;
#88087 = DIRECTION ( 'NONE',  ( -4.274815082592931898E-19, -0.9999939076577903929, -0.003490651415223739937 ) ) ;
#88086 = AXIS2_PLACEMENT_3D ( 'NONE', #53607, #52961, #15591 ) ;
#88088 = ORIENTED_EDGE ( 'NONE', *, *, #30240, .T. ) ;
#88089 = ORIENTED_EDGE ( 'NONE', *, *, #37034, .F. ) ;
#88090 = VECTOR ( 'NONE', #60646, 1000.000000000000000 ) ;
#88091 = AXIS2_PLACEMENT_3D ( 'NONE', #33572, #63020, #113405 ) ;
#88092 = PLANE ( 'NONE',  #66990 ) ;
#88093 = ORIENTED_EDGE ( 'NONE', *, *, #94823, .F. ) ;
#88094 = DIRECTION ( 'NONE',  ( -0.000000000000000000, 1.000000000000000000, -0.000000000000000000 ) ) ;
#88095 = CONICAL_SURFACE ( 'NONE', #104835, 0.09999999999999982514, 0.003490658503988666988 ) ;
#88096 = CARTESIAN_POINT ( 'NONE',  ( -6.249999999999981348, 2.500000000000000000, 2.165063509461097713 ) ) ;
#88097 = ORIENTED_EDGE ( 'NONE', *, *, #63257, .T. ) ;
#88098 = PLANE ( 'NONE',  #69091 ) ;
#88099 = VECTOR ( 'NONE', #47545, 1000.000000000000000 ) ;
#88100 = PLANE ( 'NONE',  #98539 ) ;
#88101 = DIRECTION ( 'NONE',  ( 0.000000000000000000, 1.000000000000000000, 0.000000000000000000 ) ) ;
#88102 = CONICAL_SURFACE ( 'NONE', #31703, 0.09999999999999982514, 0.003490658503988666988 ) ;
#88103 = DIRECTION ( 'NONE',  ( 0.000000000000000000, 1.000000000000000000, 0.000000000000000000 ) ) ;
#88104 = EDGE_LOOP ( 'NONE', ( #65836, #43324 ) ) ;
#88105 = CONICAL_SURFACE ( 'NONE', #46358, 0.09999999999999999167, 0.003490658503988666988 ) ;
#88106 = CARTESIAN_POINT ( 'NONE',  ( 6.049999999999932321, 2.500000000000000000, 1.818653347947321475 ) ) ;
#88107 = ORIENTED_EDGE ( 'NONE', *, *, #55461, .F. ) ;
#88108 = ORIENTED_EDGE ( 'NONE', *, *, #23123, .F. ) ;
#88109 = DIRECTION ( 'NONE',  ( 0.000000000000000000, 0.000000000000000000, -1.000000000000000000 ) ) ;
#88110 = CARTESIAN_POINT ( 'NONE',  ( -7.050000000000013145, 12.50000000000000000, 6.495190528383297135 ) ) ;
#88111 = CARTESIAN_POINT ( 'NONE',  ( 13.14999999999990088, 12.50000000000000000, 1.818653347947321475 ) ) ;
#88112 = CARTESIAN_POINT ( 'NONE',  ( -9.350000000000006750, 2.500000000000000000, -1.818653347947325916 ) ) ;
#88113 = DIRECTION ( 'NONE',  ( 0.000000000000000000, 0.000000000000000000, 1.000000000000000000 ) ) ;
#88114 = CARTESIAN_POINT ( 'NONE',  ( 14.99999999999989164, 12.50000000000000000, 0.6277270498435120194 ) ) ;
#88115 = FACE_OUTER_BOUND ( 'NONE', #68728, .T. ) ;
#88116 = CARTESIAN_POINT ( 'NONE',  ( -8.749999999999976907, 2.500000000000000000, -6.495190528383297135 ) ) ;
#88117 = FACE_OUTER_BOUND ( 'NONE', #93052, .T. ) ;
#88118 = EDGE_CURVE ( 'NONE', #69422, #109159, #79651, .T. ) ;
#88119 = EDGE_CURVE ( 'NONE', #107424, #39659, #21248, .T. ) ;
#88120 = EDGE_CURVE ( 'NONE', #125152, #92801, #54599, .T. ) ;
#88121 = CARTESIAN_POINT ( 'NONE',  ( 9.599999999999917932, 2.500000000000000000, -0.6928203230275541413 ) ) ;
#88122 = AXIS2_PLACEMENT_3D ( 'NONE', #103303, #5719, #92844 ) ;
#88123 = CONICAL_SURFACE ( 'NONE', #113281, 0.1000000000000002554, 0.003490658503988666988 ) ;
#88124 = VERTEX_POINT ( 'NONE', #65091 ) ;
#88125 = EDGE_CURVE ( 'NONE', #64242, #97332, #73476, .T. ) ;
#88126 = CARTESIAN_POINT ( 'NONE',  ( 5.849999999999931255, 2.500000000000000000, 2.857883832488649301 ) ) ;
#88127 = CARTESIAN_POINT ( 'NONE',  ( 8.349999999999919709, 2.500000000000000000, -1.572243186433550211 ) ) ;
#88128 = CARTESIAN_POINT ( 'NONE',  ( 12.94999999999990337, 2.500000000000000000, 2.065063509461097624 ) ) ;
#88129 = DIRECTION ( 'NONE',  ( 0.000000000000000000, 1.000000000000000000, 0.000000000000000000 ) ) ;
#88130 = FACE_OUTER_BOUND ( 'NONE', #26211, .T. ) ;
#88131 = CIRCLE ( 'NONE', #6551, 0.06509327318403745899 ) ;
#88132 = VECTOR ( 'NONE', #22621, 1000.000000000000000 ) ;
#88133 = ORIENTED_EDGE ( 'NONE', *, *, #33585, .F. ) ;
#88134 = EDGE_CURVE ( 'NONE', #74283, #22803, #19083, .T. ) ;
#88135 = CARTESIAN_POINT ( 'NONE',  ( 10.19999999999991225, 2.500000000000000000, -4.576537180435978236 ) ) ;
#88136 = AXIS2_PLACEMENT_3D ( 'NONE', #101413, #83066, #122985 ) ;
#88137 = EDGE_CURVE ( 'NONE', #38386, #100714, #50968, .T. ) ;
#88138 = AXIS2_PLACEMENT_3D ( 'NONE', #99921, #400, #30555 ) ;
#88139 = CARTESIAN_POINT ( 'NONE',  ( 185.3750000000000000, 8.891194145520236347, 5.444286225454521982E-16 ) ) ;
#88141 = EDGE_LOOP ( 'NONE', ( #76585, #103619, #114009, #43849 ) ) ;
#88140 = CARTESIAN_POINT ( 'NONE',  ( -1.650000000000034772, 2.500000000000000000, 2.165063509461097713 ) ) ;
#88142 = EDGE_CURVE ( 'NONE', #115638, #97971, #37979, .T. ) ;
#88143 = VECTOR ( 'NONE', #122802, 1000.000000000000000 ) ;
#88144 = EDGE_LOOP ( 'NONE', ( #118678, #124938, #83340, #108050 ) ) ;
#88146 = VECTOR ( 'NONE', #116057, 1000.000000000000000 ) ;
#88145 = DIRECTION ( 'NONE',  ( 1.000000000000000000, -0.000000000000000000, -0.000000000000000000 ) ) ;
#88147 = VERTEX_POINT ( 'NONE', #46117 ) ;
#88148 = ORIENTED_EDGE ( 'NONE', *, *, #48253, .F. ) ;
#88149 = CIRCLE ( 'NONE', #31759, 0.1000000000000000472 ) ;
#88150 = ORIENTED_EDGE ( 'NONE', *, *, #120422, .T. ) ;
#88151 = AXIS2_PLACEMENT_3D ( 'NONE', #43041, #13537, #63942 ) ;
#88152 = CARTESIAN_POINT ( 'NONE',  ( 13.74999999999989875, 12.50000000000000000, 1.472243186433545459 ) ) ;
#88153 = CIRCLE ( 'NONE', #121626, 0.09999999999999982514 ) ;
#88154 = DIRECTION ( 'NONE',  ( 0.000000000000000000, 0.000000000000000000, 1.000000000000000000 ) ) ;
#88155 = DIRECTION ( 'NONE',  ( 0.000000000000000000, 0.000000000000000000, 1.000000000000000000 ) ) ;
#88156 = CARTESIAN_POINT ( 'NONE',  ( 4.599999999999937472, 2.500000000000000000, 0.6928203230275494784 ) ) ;
#88157 = ORIENTED_EDGE ( 'NONE', *, *, #124397, .F. ) ;
#88158 = AXIS2_PLACEMENT_3D ( 'NONE', #125719, #65526, #105464 ) ;
#88159 = FACE_OUTER_BOUND ( 'NONE', #96266, .T. ) ;
#88160 = ORIENTED_EDGE ( 'NONE', *, *, #13821, .T. ) ;
#88161 = CARTESIAN_POINT ( 'NONE',  ( 14.39999999999989555, 2.500000000000000000, 0.3464101615137736845 ) ) ;
#88162 = CARTESIAN_POINT ( 'NONE',  ( 16.04820284965659027, -1.499999999999968026, -6.585610464672694064 ) ) ;
#88163 = CARTESIAN_POINT ( 'NONE',  ( 17.33812564108900389, 2.538896947917175684, 5.379288978442783531 ) ) ;
#88164 = CARTESIAN_POINT ( 'NONE',  ( -1.650000000000034328, 2.500000000000000000, -7.188010851410854052 ) ) ;
#88165 = CARTESIAN_POINT ( 'NONE',  ( 9.399999999999918643, 2.500000000000000000, -0.4464101615137782142 ) ) ;
#88166 = VERTEX_POINT ( 'NONE', #46774 ) ;
#88167 = ORIENTED_EDGE ( 'NONE', *, *, #16568, .T. ) ;
#88168 = ORIENTED_EDGE ( 'NONE', *, *, #83892, .T. ) ;
#88169 = ORIENTED_EDGE ( 'NONE', *, *, #93050, .F. ) ;
#88170 = EDGE_LOOP ( 'NONE', ( #8884, #36467 ) ) ;
#88171 = DIRECTION ( 'NONE',  ( 0.000000000000000000, -0.000000000000000000, 1.000000000000000000 ) ) ;
#88172 = DIRECTION ( 'NONE',  ( 0.000000000000000000, 0.000000000000000000, 1.000000000000000000 ) ) ;
#88173 = FACE_OUTER_BOUND ( 'NONE', #105389, .T. ) ;
#88174 = FACE_BOUND ( 'NONE', #7486, .T. ) ;
#88175 = DIRECTION ( 'NONE',  ( 0.000000000000000000, 1.000000000000000000, 0.000000000000000000 ) ) ;
#88176 = DIRECTION ( 'NONE',  ( -0.000000000000000000, 1.000000000000000000, -0.000000000000000000 ) ) ;
#88177 = CARTESIAN_POINT ( 'NONE',  ( 0.8499999999999536815, 12.50000000000000000, 6.495190528383297135 ) ) ;
#88178 = CARTESIAN_POINT ( 'NONE',  ( 11.84999999999990727, 2.500000000000000000, -1.818653347947326138 ) ) ;
#88179 = EDGE_CURVE ( 'NONE', #127460, #10341, #97154, .T. ) ;
#88180 = CIRCLE ( 'NONE', #48503, 0.06509327318403745899 ) ;
#88182 = CIRCLE ( 'NONE', #56887, 0.06509327318403745899 ) ;
#88181 = CARTESIAN_POINT ( 'NONE',  ( -10.60000000000000142, 2.500000000000000000, -0.4464101615137782142 ) ) ;
#88183 = LINE ( 'NONE', #59427, #32212 ) ;
#88184 = DIRECTION ( 'NONE',  ( 0.000000000000000000, 0.000000000000000000, -1.000000000000000000 ) ) ;
#88185 = AXIS2_PLACEMENT_3D ( 'NONE', #123923, #94461, #34289 ) ;
#88187 = DIRECTION ( 'NONE',  ( 0.000000000000000000, 0.000000000000000000, 1.000000000000000000 ) ) ;
#88186 = AXIS2_PLACEMENT_3D ( 'NONE', #37935, #77847, #7168 ) ;
#88188 = ORIENTED_EDGE ( 'NONE', *, *, #56967, .F. ) ;
#88189 = ORIENTED_EDGE ( 'NONE', *, *, #92894, .F. ) ;
#88190 = ORIENTED_EDGE ( 'NONE', *, *, #29178, .F. ) ;
#88191 = ORIENTED_EDGE ( 'NONE', *, *, #10807, .F. ) ;
#88192 = CIRCLE ( 'NONE', #84004, 0.06509327318403745899 ) ;
#88193 = AXIS2_PLACEMENT_3D ( 'NONE', #36841, #116028, #76759 ) ;
#88194 = LINE ( 'NONE', #29314, #69484 ) ;
#88195 = FACE_BOUND ( 'NONE', #20172, .T. ) ;
#88196 = AXIS2_PLACEMENT_3D ( 'NONE', #67780, #59280, #37691 ) ;
#88197 = CARTESIAN_POINT ( 'NONE',  ( 1.899999999999951283, 2.500000000000000000, -0.2464101615137782308 ) ) ;
#88198 = VERTEX_POINT ( 'NONE', #37599 ) ;
#88199 = DIRECTION ( 'NONE',  ( -0.000000000000000000, -1.000000000000000000, -0.000000000000000000 ) ) ;
#88200 = DIRECTION ( 'NONE',  ( 0.000000000000000000, 0.000000000000000000, 1.000000000000000000 ) ) ;
#88201 = DIRECTION ( 'NONE',  ( -0.000000000000000000, -1.000000000000000000, -0.000000000000000000 ) ) ;
#88202 = DIRECTION ( 'NONE',  ( -0.000000000000000000, -1.000000000000000000, -0.000000000000000000 ) ) ;
#88203 = ORIENTED_EDGE ( 'NONE', *, *, #87389, .T. ) ;
#88204 = DIRECTION ( 'NONE',  ( -1.000000000000000000, -0.000000000000000000, -0.000000000000000000 ) ) ;
#88205 = PLANE ( 'NONE',  #9487 ) ;
#88206 = EDGE_LOOP ( 'NONE', ( #128320, #71202, #36049, #51998 ) ) ;
#88207 = ORIENTED_EDGE ( 'NONE', *, *, #115752, .T. ) ;
#88208 = DIRECTION ( 'NONE',  ( -0.000000000000000000, -1.000000000000000000, -0.000000000000000000 ) ) ;
#88209 = DIRECTION ( 'NONE',  ( 0.000000000000000000, 1.000000000000000000, 0.000000000000000000 ) ) ;
#88210 = ADVANCED_FACE ( 'NONE', ( #15345 ), #37890, .T. ) ;
#88211 = ORIENTED_EDGE ( 'NONE', *, *, #16900, .F. ) ;
#88212 = CONICAL_SURFACE ( 'NONE', #31819, 0.1000000000000002554, 0.003490658503988666988 ) ;
#88213 = ADVANCED_FACE ( 'NONE', ( #116778 ), #117369, .T. ) ;
#88214 = LINE ( 'NONE', #129492, #44665 ) ;
#88215 = DIRECTION ( 'NONE',  ( 0.000000000000000000, -0.000000000000000000, 1.000000000000000000 ) ) ;
#88216 = VERTEX_POINT ( 'NONE', #36320 ) ;
#88217 = CARTESIAN_POINT ( 'NONE',  ( -5.200000000000020606, 12.50000000000000000, 3.983716857408420964 ) ) ;
#88218 = ORIENTED_EDGE ( 'NONE', *, *, #85728, .T. ) ;
#88219 = ADVANCED_FACE ( 'NONE', ( #17943 ), #57885, .T. ) ;
#88220 = DIRECTION ( 'NONE',  ( -0.000000000000000000, 1.000000000000000000, -0.000000000000000000 ) ) ;
#88221 = ADVANCED_FACE ( 'NONE', ( #74936 ), #111023, .T. ) ;
#88222 = ORIENTED_EDGE ( 'NONE', *, *, #12712, .T. ) ;
#88223 = DIRECTION ( 'NONE',  ( 0.000000000000000000, 1.000000000000000000, 0.000000000000000000 ) ) ;
#88224 = CONICAL_SURFACE ( 'NONE', #79938, 0.1000000000000002554, 0.003490658503988666988 ) ;
#88225 = FACE_BOUND ( 'NONE', #4157, .T. ) ;
#88226 = CONICAL_SURFACE ( 'NONE', #23404, 0.09999999999999999167, 0.003490658503988666988 ) ;
#88227 = ORIENTED_EDGE ( 'NONE', *, *, #81361, .T. ) ;
#88228 = AXIS2_PLACEMENT_3D ( 'NONE', #15373, #26513, #87980 ) ;
#88229 = CARTESIAN_POINT ( 'NONE',  ( 112.8336731274835643, 7.592877920657278068, 1.321915336562208276 ) ) ;
#88230 = ORIENTED_EDGE ( 'NONE', *, *, #114338, .T. ) ;
#88231 = DIRECTION ( 'NONE',  ( -0.000000000000000000, -1.000000000000000000, -0.000000000000000000 ) ) ;
#88232 = LINE ( 'NONE', #7758, #36182 ) ;
#88233 = ADVANCED_FACE ( 'NONE', ( #116138 ), #100662, .T. ) ;
#88234 = ADVANCED_FACE ( 'NONE', ( #26487 ), #71321, .T. ) ;
#88235 = DIRECTION ( 'NONE',  ( 0.000000000000000000, 0.000000000000000000, -1.000000000000000000 ) ) ;
#88236 = ADVANCED_FACE ( 'NONE', ( #75567 ), #31638, .T. ) ;
#88237 = CARTESIAN_POINT ( 'NONE',  ( 127.5000000000000000, 5.000000000000000000, 5.000000000000001776 ) ) ;
#88238 = EDGE_CURVE ( 'NONE', #78195, #87945, #88032, .T. ) ;
#88239 = EDGE_CURVE ( 'NONE', #89132, #105744, #23299, .T. ) ;
#88240 = DIRECTION ( 'NONE',  ( 0.000000000000000000, 0.000000000000000000, -1.000000000000000000 ) ) ;
#88241 = CONICAL_SURFACE ( 'NONE', #94519, 0.09999999999999982514, 0.003490658503988666988 ) ;
#88242 = ORIENTED_EDGE ( 'NONE', *, *, #28281, .T. ) ;
#88243 = EDGE_LOOP ( 'NONE', ( #44409, #64455 ) ) ;
#88244 = TOROIDAL_SURFACE ( 'NONE', #123752, 4.000000000000000000, 1.000000000000000000 ) ;
#88245 = ORIENTED_EDGE ( 'NONE', *, *, #4889, .T. ) ;
#88246 = DIRECTION ( 'NONE',  ( 0.000000000000000000, 0.000000000000000000, 1.000000000000000000 ) ) ;
#88247 = LINE ( 'NONE', #100653, #13864 ) ;
#88248 = CONICAL_SURFACE ( 'NONE', #115437, 0.09999999999999999167, 0.003490658503988666988 ) ;
#88249 = FACE_OUTER_BOUND ( 'NONE', #92008, .T. ) ;
#88251 = EDGE_LOOP ( 'NONE', ( #85746, #69812, #101833, #7405 ) ) ;
#88250 = EDGE_LOOP ( 'NONE', ( #39330, #84213, #18309, #48642 ) ) ;
#88252 = ORIENTED_EDGE ( 'NONE', *, *, #43777, .F. ) ;
#88253 = EDGE_CURVE ( 'NONE', #32556, #10759, #108969, .T. ) ;
#88254 = FACE_OUTER_BOUND ( 'NONE', #61865, .T. ) ;
#88255 = CIRCLE ( 'NONE', #31849, 0.06509327318403745899 ) ;
#88256 = FACE_OUTER_BOUND ( 'NONE', #97373, .T. ) ;
#88257 = PRODUCT_CONTEXT ( 'NONE', #31330, 'mechanical' ) ;
#88258 = CARTESIAN_POINT ( 'NONE',  ( 9.149999999999918643, 2.500000000000000000, 2.065063509461097624 ) ) ;
#88259 = AXIS2_PLACEMENT_3D ( 'NONE', #85009, #124946, #73910 ) ;
#88260 = CARTESIAN_POINT ( 'NONE',  ( 13.14999999999990088, 12.50000000000000000, 2.511473670974873507 ) ) ;
#88261 = CARTESIAN_POINT ( 'NONE',  ( -11.69999999999999574, 12.50000000000000000, 4.395220292106234439 ) ) ;
#88262 = DIRECTION ( 'NONE',  ( 0.000000000000000000, 0.000000000000000000, 1.000000000000000000 ) ) ;
#88263 = DIRECTION ( 'NONE',  ( 0.000000000000000000, 0.000000000000000000, 1.000000000000000000 ) ) ;
#88264 = DIRECTION ( 'NONE',  ( 1.000000000000000000, -0.000000000000000000, -0.000000000000000000 ) ) ;
#88265 = VERTEX_POINT ( 'NONE', #70278 ) ;
#88266 = ORIENTED_EDGE ( 'NONE', *, *, #99350, .F. ) ;
#88267 = CARTESIAN_POINT ( 'NONE',  ( -3.350000000000029399, 2.500000000000000000, 6.395190528383296602 ) ) ;
#88268 = DIRECTION ( 'NONE',  ( -0.000000000000000000, 1.000000000000000000, -0.000000000000000000 ) ) ;
#88269 = ORIENTED_EDGE ( 'NONE', *, *, #86142, .F. ) ;
#88270 = ORIENTED_EDGE ( 'NONE', *, *, #8617, .T. ) ;
#88271 = CARTESIAN_POINT ( 'NONE',  ( 186.0260416670080588, -6.551208109652273848, -3.782341765625003571 ) ) ;
#88272 = CARTESIAN_POINT ( 'NONE',  ( 7.049999999999926992, 2.500000000000000000, 2.165063509461097713 ) ) ;
#88273 = CARTESIAN_POINT ( 'NONE',  ( 4.999999999999971578, 12.50000000000000000, -2.276824562219559311E-15 ) ) ;
#88274 = DIRECTION ( 'NONE',  ( 0.000000000000000000, -0.9999939076577903929, 0.003490651415223739937 ) ) ;
#88275 = DIRECTION ( 'NONE',  ( 0.000000000000000000, 0.000000000000000000, 1.000000000000000000 ) ) ;
#88276 = AXIS2_PLACEMENT_3D ( 'NONE', #50710, #297, #89979 ) ;
#88277 = CARTESIAN_POINT ( 'NONE',  ( -5.800000000000018474, 2.500000000000000000, 4.230127018922196669 ) ) ;
#88278 = DIRECTION ( 'NONE',  ( -4.274815082592931898E-19, -0.9999939076577903929, -0.003490651415223739937 ) ) ;
#88279 = AXIS2_PLACEMENT_3D ( 'NONE', #87849, #127787, #6065 ) ;
#88280 = CIRCLE ( 'NONE', #11018, 0.06509327318403745899 ) ;
#88281 = EDGE_CURVE ( 'NONE', #39517, #33308, #100377, .T. ) ;
#88282 = EDGE_CURVE ( 'NONE', #52515, #52645, #99743, .T. ) ;
#88283 = DIRECTION ( 'NONE',  ( 0.000000000000000000, 0.000000000000000000, 1.000000000000000000 ) ) ;
#88284 = CIRCLE ( 'NONE', #119692, 0.09999999999999982514 ) ;
#88285 = ORIENTED_EDGE ( 'NONE', *, *, #101355, .F. ) ;
#88286 = CONICAL_SURFACE ( 'NONE', #69517, 0.1000000000000002554, 0.003490658503988666988 ) ;
#88287 = ADVANCED_FACE ( 'NONE', ( #40835 ), #10051, .F. ) ;
#88288 = CONICAL_SURFACE ( 'NONE', #71587, 0.09999999999999982514, 0.003490658503988666988 ) ;
#88289 = EDGE_LOOP ( 'NONE', ( #67155, #74496 ) ) ;
#88290 = AXIS2_PLACEMENT_3D ( 'NONE', #34351, #5494, #33689 ) ;
#88291 = AXIS2_PLACEMENT_3D ( 'NONE', #60136, #97454, #8416 ) ;
#88292 = VERTEX_POINT ( 'NONE', #886 ) ;
#88293 = EDGE_CURVE ( 'NONE', #89801, #76324, #65061, .T. ) ;
#88294 = ORIENTED_EDGE ( 'NONE', *, *, #24584, .F. ) ;
#88295 = CARTESIAN_POINT ( 'NONE',  ( 11.24999999999994316, 12.50000000000000000, -6.430097255199264339 ) ) ;
#88296 = DIRECTION ( 'NONE',  ( 0.000000000000000000, 0.000000000000000000, 1.000000000000000000 ) ) ;
#88297 = AXIS2_PLACEMENT_3D ( 'NONE', #22167, #92162, #101997 ) ;
#88298 = EDGE_CURVE ( 'NONE', #65655, #39561, #96457, .T. ) ;
#88299 = ORIENTED_EDGE ( 'NONE', *, *, #75659, .F. ) ;
#88300 = EDGE_CURVE ( 'NONE', #18873, #21324, #40048, .T. ) ;
#88301 = CARTESIAN_POINT ( 'NONE',  ( -11.84999999999999787, 2.500000000000000000, -6.248780366869523206 ) ) ;
#88302 = CARTESIAN_POINT ( 'NONE',  ( 17.50000000000000000, 0.9166666666666684060, -3.432456362931489036 ) ) ;
#88303 = ADVANCED_FACE ( 'NONE', ( #19891 ), #10063, .T. ) ;
#88304 = CARTESIAN_POINT ( 'NONE',  ( 4.199999999999941558, 2.500000000000000000, -4.230127018922201998 ) ) ;
#88306 = ORIENTED_EDGE ( 'NONE', *, *, #68210, .T. ) ;
#88305 = FACE_OUTER_BOUND ( 'NONE', #69700, .T. ) ;
#88307 = CARTESIAN_POINT ( 'NONE',  ( 7.699999999999923794, 2.500000000000000000, -3.883716857408426648 ) ) ;
#88308 = EDGE_CURVE ( 'NONE', #106514, #88607, #52557, .T. ) ;
#88310 = DIRECTION ( 'NONE',  ( 0.000000000000000000, -0.9999939076577903929, 0.003490651415223739937 ) ) ;
#88309 = AXIS2_PLACEMENT_3D ( 'NONE', #69167, #116342, #48918 ) ;
#88311 = ORIENTED_EDGE ( 'NONE', *, *, #107055, .F. ) ;
#88312 = EDGE_LOOP ( 'NONE', ( #55649, #112630, #102998, #18831 ) ) ;
#88313 = ORIENTED_EDGE ( 'NONE', *, *, #44667, .F. ) ;
#88314 = DIRECTION ( 'NONE',  ( 0.000000000000000000, 1.000000000000000000, 0.000000000000000000 ) ) ;
#88315 = CONICAL_SURFACE ( 'NONE', #75804, 0.09999999999999982514, 0.003490658503988666988 ) ;
#88316 = DIRECTION ( 'NONE',  ( 0.000000000000000000, 0.000000000000000000, 1.000000000000000000 ) ) ;
#88317 = MECHANICAL_DESIGN_GEOMETRIC_PRESENTATION_REPRESENTATION (  '', ( #10944 ), #36121 ) ;
#88318 = ORIENTED_EDGE ( 'NONE', *, *, #21182, .F. ) ;
#88319 = CARTESIAN_POINT ( 'NONE',  ( -10.45000000000000462, 12.50000000000000000, -6.560283801567336148 ) ) ;
#88320 = DIRECTION ( 'NONE',  ( -0.000000000000000000, -1.000000000000000000, -0.000000000000000000 ) ) ;
#88321 = LINE ( 'NONE', #109932, #121561 ) ;
#88322 = DIRECTION ( 'NONE',  ( 0.000000000000000000, 0.000000000000000000, 1.000000000000000000 ) ) ;
#88323 = ADVANCED_FACE ( 'NONE', ( #40176 ), #83938, .T. ) ;
#88324 = CIRCLE ( 'NONE', #119638, 0.1000000000000002554 ) ;
#88325 = ORIENTED_EDGE ( 'NONE', *, *, #118237, .F. ) ;
#88326 = CARTESIAN_POINT ( 'NONE',  ( -12.89999999999999325, 12.50000000000000000, 0.6928203230275535862 ) ) ;
#88327 = ORIENTED_EDGE ( 'NONE', *, *, #119805, .F. ) ;
#88328 = ORIENTED_EDGE ( 'NONE', *, *, #102585, .T. ) ;
#88329 = DIRECTION ( 'NONE',  ( -0.000000000000000000, 1.000000000000000000, -0.000000000000000000 ) ) ;
#88330 = FACE_OUTER_BOUND ( 'NONE', #97621, .T. ) ;
#88331 = FACE_BOUND ( 'NONE', #110558, .T. ) ;
#88332 = CARTESIAN_POINT ( 'NONE',  ( -15.79999999999998117, 2.500000000000000000, 0.000000000000000000 ) ) ;
#88334 = DIRECTION ( 'NONE',  ( -0.000000000000000000, 1.000000000000000000, -0.000000000000000000 ) ) ;
#88333 = CIRCLE ( 'NONE', #46589, 0.1000000000000002554 ) ;
#88336 = CARTESIAN_POINT ( 'NONE',  ( -12.89999999999999147, 12.50000000000000000, 4.330127018922196314 ) ) ;
#88335 = CIRCLE ( 'NONE', #100869, 0.09999999999999982514 ) ;
#88337 = ADVANCED_FACE ( 'NONE', ( #80095 ), #127902, .T. ) ;
#88338 = AXIS2_PLACEMENT_3D ( 'NONE', #43871, #102758, #73300 ) ;
#88339 = AXIS2_PLACEMENT_3D ( 'NONE', #122750, #128893, #103760 ) ;
#88340 = AXIS2_PLACEMENT_3D ( 'NONE', #76519, #116419, #45775 ) ;
#88341 = VERTEX_POINT ( 'NONE', #49365 ) ;
#88342 = DIRECTION ( 'NONE',  ( 0.000000000000000000, 0.000000000000000000, 1.000000000000000000 ) ) ;
#88343 = PLANE ( 'NONE',  #88699 ) ;
#88344 = CARTESIAN_POINT ( 'NONE',  ( 15.59999999999988951, 2.500000000000000000, 0.3464101615137735735 ) ) ;
#88345 = AXIS2_PLACEMENT_3D ( 'NONE', #97395, #47667, #86926 ) ;
#88346 = DIRECTION ( 'NONE',  ( 0.000000000000000000, 0.000000000000000000, -1.000000000000000000 ) ) ;
#88347 = VERTEX_POINT ( 'NONE', #38911 ) ;
#88348 = FACE_OUTER_BOUND ( 'NONE', #101349, .T. ) ;
#88349 = FACE_OUTER_BOUND ( 'NONE', #108603, .T. ) ;
#88350 = CONICAL_SURFACE ( 'NONE', #84252, 0.09999999999999982514, 0.003490658503988666988 ) ;
#88351 = ORIENTED_EDGE ( 'NONE', *, *, #118549, .F. ) ;
#88352 = ORIENTED_EDGE ( 'NONE', *, *, #46155, .F. ) ;
#88353 = DIRECTION ( 'NONE',  ( 0.000000000000000000, -0.000000000000000000, 1.000000000000000000 ) ) ;
#88354 = EDGE_CURVE ( 'NONE', #24335, #97955, #113181, .T. ) ;
#88355 = CARTESIAN_POINT ( 'NONE',  ( -6.650000000000014566, 2.500000000000000000, 1.472243186433545459 ) ) ;
#88356 = FACE_BOUND ( 'NONE', #19939, .T. ) ;
#88357 = CARTESIAN_POINT ( 'NONE',  ( -13.74999999999995381, 2.500000000000000000, -2.165063509461099489 ) ) ;
#88358 = ORIENTED_EDGE ( 'NONE', *, *, #118446, .T. ) ;
#88359 = DIRECTION ( 'NONE',  ( 0.000000000000000000, -0.000000000000000000, 1.000000000000000000 ) ) ;
#88360 = VERTEX_POINT ( 'NONE', #119360 ) ;
#88362 = ORIENTED_EDGE ( 'NONE', *, *, #42204, .T. ) ;
#88361 = AXIS2_PLACEMENT_3D ( 'NONE', #83149, #42586, #102135 ) ;
#88364 = VECTOR ( 'NONE', #64164, 1000.000000000000000 ) ;
#88363 = CARTESIAN_POINT ( 'NONE',  ( 8.749999999999920064, 2.500000000000000000, 5.802370205355744659 ) ) ;
#88365 = CARTESIAN_POINT ( 'NONE',  ( 186.3333333333333144, 6.668395609140177704, -3.849999999999998312 ) ) ;
#88366 = ORIENTED_EDGE ( 'NONE', *, *, #96390, .F. ) ;
#88367 = DIRECTION ( 'NONE',  ( -4.274815082592931898E-19, -0.9999939076577903929, -0.003490651415223739937 ) ) ;
#88368 = FACE_OUTER_BOUND ( 'NONE', #63014, .T. ) ;
#88369 = AXIS2_PLACEMENT_3D ( 'NONE', #18382, #40637, #30808 ) ;
#88370 = AXIS2_PLACEMENT_3D ( 'NONE', #105704, #63842, #85408 ) ;
#88371 = CARTESIAN_POINT ( 'NONE',  ( -12.69999999999999041, 12.50000000000000000, 3.983716857408420964 ) ) ;
#88372 = CARTESIAN_POINT ( 'NONE',  ( -1.250000000000035749, 2.500000000000000000, -2.757883832488654097 ) ) ;
#88373 = CIRCLE ( 'NONE', #48705, 0.06509327318403745899 ) ;
#88375 = EDGE_LOOP ( 'NONE', ( #95277, #2532, #94953, #112382 ) ) ;
#88374 = CIRCLE ( 'NONE', #90545, 0.06509327318403745899 ) ;
#88377 = ADVANCED_FACE ( 'NONE', ( #29703 ), #56732, .T. ) ;
#88376 = VECTOR ( 'NONE', #93313, 1000.000000000000000 ) ;
#88378 = CARTESIAN_POINT ( 'NONE',  ( 12.89999999999990266, 12.50000000000000000, -3.637306695894650055 ) ) ;
#88379 = CARTESIAN_POINT ( 'NONE',  ( -14.14999999999998614, 2.500000000000000000, 2.165063509461101265 ) ) ;
#88380 = DIRECTION ( 'NONE',  ( 0.000000000000000000, 0.000000000000000000, -1.000000000000000000 ) ) ;
#88381 = VECTOR ( 'NONE', #30654, 1000.000000000000000 ) ;
#88382 = CARTESIAN_POINT ( 'NONE',  ( -11.84999999999999787, 12.50000000000000000, -6.148780366869522673 ) ) ;
#88384 = ORIENTED_EDGE ( 'NONE', *, *, #8145, .F. ) ;
#88383 = AXIS2_PLACEMENT_3D ( 'NONE', #127977, #61174, #29154 ) ;
#88385 = DIRECTION ( 'NONE',  ( 0.000000000000000000, 1.000000000000000000, 0.000000000000000000 ) ) ;
#88386 = EDGE_LOOP ( 'NONE', ( #64812, #86124 ) ) ;
#88387 = CARTESIAN_POINT ( 'NONE',  ( -12.29999999999999538, 12.50000000000000000, -0.3464101615137741841 ) ) ;
#88388 = AXIS2_PLACEMENT_3D ( 'NONE', #29876, #29247, #8925 ) ;
#88389 = ORIENTED_EDGE ( 'NONE', *, *, #1494, .T. ) ;
#88390 = DIRECTION ( 'NONE',  ( 0.000000000000000000, 0.000000000000000000, 1.000000000000000000 ) ) ;
#88391 = CARTESIAN_POINT ( 'NONE',  ( 87.50000000000002842, -6.099025433955696407, 4.412011999988003197 ) ) ;
#88392 = DIRECTION ( 'NONE',  ( 0.000000000000000000, 0.000000000000000000, -1.000000000000000000 ) ) ;
#88393 = DIRECTION ( 'NONE',  ( 0.000000000000000000, 0.000000000000000000, 1.000000000000000000 ) ) ;
#88394 = VERTEX_POINT ( 'NONE', #32313 ) ;
#88395 = DIRECTION ( 'NONE',  ( 0.000000000000000000, 0.000000000000000000, 1.000000000000000000 ) ) ;
#88396 = LINE ( 'NONE', #129019, #73153 ) ;
#88397 = CARTESIAN_POINT ( 'NONE',  ( 87.50000000000001421, 3.974992050023852475, -6.359987280038158275 ) ) ;
#88398 = EDGE_CURVE ( 'NONE', #8342, #94677, #119442, .T. ) ;
#88399 = EDGE_CURVE ( 'NONE', #113969, #39135, #46289, .T. ) ;
#88400 = FACE_OUTER_BOUND ( 'NONE', #29140, .T. ) ;
#88401 = CARTESIAN_POINT ( 'NONE',  ( 10.19999999999991047, 12.50000000000000000, -4.048810130592463530 ) ) ;
#88402 = ADVANCED_FACE ( 'NONE', ( #13912 ), #27491, .T. ) ;
#88403 = EDGE_CURVE ( 'NONE', #88678, #99143, #72218, .T. ) ;
#88404 = FACE_OUTER_BOUND ( 'NONE', #101933, .T. ) ;
#88405 = CONICAL_SURFACE ( 'NONE', #25622, 0.1000000000000002554, 0.003490658503988666988 ) ;
#88406 = ORIENTED_EDGE ( 'NONE', *, *, #5469, .T. ) ;
#88407 = ORIENTED_EDGE ( 'NONE', *, *, #11623, .F. ) ;
#88408 = FACE_OUTER_BOUND ( 'NONE', #106837, .T. ) ;
#88410 = VERTEX_POINT ( 'NONE', #123244 ) ;
#88409 = ADVANCED_FACE ( 'NONE', ( #102317 ), #102946, .T. ) ;
#88411 = DIRECTION ( 'NONE',  ( 0.000000000000000000, 0.000000000000000000, 1.000000000000000000 ) ) ;
#88413 = ORIENTED_EDGE ( 'NONE', *, *, #65041, .F. ) ;
#88412 = VERTEX_POINT ( 'NONE', #112137 ) ;
#88414 = ORIENTED_EDGE ( 'NONE', *, *, #54698, .F. ) ;
#88415 = ADVANCED_FACE ( 'NONE', ( #73478 ), #122600, .T. ) ;
#88416 = CARTESIAN_POINT ( 'NONE',  ( 139.9358549477330200, 0.5000000000000000000, -1.098523788719517169 ) ) ;
#88417 = AXIS2_PLACEMENT_3D ( 'NONE', #2849, #73514, #23789 ) ;
#88419 = EDGE_CURVE ( 'NONE', #112572, #1361, #29671, .T. ) ;
#88418 = AXIS2_PLACEMENT_3D ( 'NONE', #13354, #80830, #41559 ) ;
#88420 = LINE ( 'NONE', #49181, #21405 ) ;
#88421 = CIRCLE ( 'NONE', #4787, 0.06509327318403743123 ) ;
#88422 = EDGE_CURVE ( 'NONE', #51142, #62518, #83326, .T. ) ;
#88423 = DIRECTION ( 'NONE',  ( 0.000000000000000000, -0.9999939076577903929, 0.003490651415223739937 ) ) ;
#88424 = CARTESIAN_POINT ( 'NONE',  ( -4.800000000000026468, 12.50000000000000000, -4.741630453620016006 ) ) ;
#88425 = DIRECTION ( 'NONE',  ( 0.000000000000000000, 1.000000000000000000, 0.000000000000000000 ) ) ;
#88426 = CARTESIAN_POINT ( 'NONE',  ( -6.900000000000015454, 12.50000000000000000, 4.676537180435972552 ) ) ;
#88427 = DIRECTION ( 'NONE',  ( -0.000000000000000000, -1.000000000000000000, -0.000000000000000000 ) ) ;
#88428 = PRODUCT_DEFINITION ( 'UNKNOWN', '', #25460, #116111 ) ;
#88429 = EDGE_CURVE ( 'NONE', #31342, #96613, #113416, .T. ) ;
#88430 = AXIS2_PLACEMENT_3D ( 'NONE', #114055, #122586, #25028 ) ;
#88431 = CARTESIAN_POINT ( 'NONE',  ( 8.749999999999921840, 2.500000000000000000, 2.757883832488649656 ) ) ;
#88432 = VERTEX_POINT ( 'NONE', #72851 ) ;
#88433 = AXIS2_PLACEMENT_3D ( 'NONE', #1313, #26, #9207 ) ;
#88434 = VERTEX_POINT ( 'NONE', #52559 ) ;
#88435 = CIRCLE ( 'NONE', #54989, 0.09999999999999982514 ) ;
#88436 = ORIENTED_EDGE ( 'NONE', *, *, #90029, .T. ) ;
#88437 = DIRECTION ( 'NONE',  ( -0.000000000000000000, -1.000000000000000000, -0.000000000000000000 ) ) ;
#88438 = ORIENTED_EDGE ( 'NONE', *, *, #88179, .T. ) ;
#88439 = ORIENTED_EDGE ( 'NONE', *, *, #77075, .F. ) ;
#88440 = CARTESIAN_POINT ( 'NONE',  ( -1.850000000000033840, 2.500000000000000000, 1.818653347947321475 ) ) ;
#88441 = DIRECTION ( 'NONE',  ( 0.000000000000000000, 0.000000000000000000, 1.000000000000000000 ) ) ;
#88442 = CARTESIAN_POINT ( 'NONE',  ( -1.250000000000001110, 2.500000000000000000, -2.265063509461101798 ) ) ;
#88443 = VECTOR ( 'NONE', #31320, 1000.000000000000000 ) ;
#88444 = FACE_OUTER_BOUND ( 'NONE', #11514, .T. ) ;
#88445 = CIRCLE ( 'NONE', #50903, 0.1000000000000002554 ) ;
#88446 = CIRCLE ( 'NONE', #105176, 0.06509327318403745899 ) ;
#88447 = DIRECTION ( 'NONE',  ( 0.000000000000000000, 1.000000000000000000, 0.000000000000000000 ) ) ;
#88448 = ORIENTED_EDGE ( 'NONE', *, *, #49356, .T. ) ;
#88449 = DIRECTION ( 'NONE',  ( 0.000000000000000000, 1.000000000000000000, 0.000000000000000000 ) ) ;
#88450 = ORIENTED_EDGE ( 'NONE', *, *, #53880, .T. ) ;
#88451 = CARTESIAN_POINT ( 'NONE',  ( 0.6499999999999561684, 2.500000000000000000, 2.511473670974873507 ) ) ;
#88452 = EDGE_LOOP ( 'NONE', ( #123433, #118432 ) ) ;
#88453 = CIRCLE ( 'NONE', #32054, 0.1000000000000002554 ) ;
#88454 = DIRECTION ( 'NONE',  ( 0.000000000000000000, 0.000000000000000000, -1.000000000000000000 ) ) ;
#88455 = ORIENTED_EDGE ( 'NONE', *, *, #114042, .T. ) ;
#88456 = ORIENTED_EDGE ( 'NONE', *, *, #94317, .T. ) ;
#88457 = CARTESIAN_POINT ( 'NONE',  ( 4.349999999999936584, 2.500000000000000000, 6.148780366869520009 ) ) ;
#88458 = CARTESIAN_POINT ( 'NONE',  ( 59.86274543073836440, -3.775833904478944181, -4.995381933851996692 ) ) ;
#88459 = EDGE_CURVE ( 'NONE', #47201, #10577, #53858, .T. ) ;
#88460 = CARTESIAN_POINT ( 'NONE',  ( 6.899999999999928413, 2.500000000000000000, 3.883716857408421319 ) ) ;
#88461 = PLANE ( 'NONE',  #547 ) ;
#88462 = EDGE_CURVE ( 'NONE', #108826, #28226, #38078, .T. ) ;
#88463 = DIRECTION ( 'NONE',  ( -4.274815082592931898E-19, -0.9999939076577903929, -0.003490651415223739937 ) ) ;
#88464 = ORIENTED_EDGE ( 'NONE', *, *, #37237, .T. ) ;
#88465 = CARTESIAN_POINT ( 'NONE',  ( 3.349999999999945466, 12.50000000000000000, -2.857883832488653741 ) ) ;
#88467 = AXIS2_PLACEMENT_3D ( 'NONE', #127570, #57545, #17600 ) ;
#88466 = CARTESIAN_POINT ( 'NONE',  ( 8.549999999999924327, 2.500000000000000000, -6.941600689897077459 ) ) ;
#88468 = VECTOR ( 'NONE', #112563, 1000.000000000000000 ) ;
#88469 = PLANE ( 'NONE',  #16453 ) ;
#88470 = DIRECTION ( 'NONE',  ( -0.000000000000000000, 1.000000000000000000, -0.000000000000000000 ) ) ;
#88471 = ADVANCED_FACE ( 'NONE', ( #123866 ), #88123, .T. ) ;
#88472 = DIRECTION ( 'NONE',  ( 0.000000000000000000, -0.000000000000000000, 1.000000000000000000 ) ) ;
#88473 = EDGE_LOOP ( 'NONE', ( #45025, #9693 ) ) ;
#88474 = CIRCLE ( 'NONE', #32071, 0.1000000000000002554 ) ;
#88475 = CIRCLE ( 'NONE', #117705, 0.06509327318403745899 ) ;
#88476 = ORIENTED_EDGE ( 'NONE', *, *, #62198, .F. ) ;
#88477 = AXIS2_PLACEMENT_3D ( 'NONE', #24834, #15636, #55584 ) ;
#88478 = VECTOR ( 'NONE', #121963, 1000.000000000000000 ) ;
#88479 = LINE ( 'NONE', #49876, #73822 ) ;
#88480 = ORIENTED_EDGE ( 'NONE', *, *, #11658, .T. ) ;
#88481 = CARTESIAN_POINT ( 'NONE',  ( 16.73738517751860755, -0.6985710796761546160, 5.899868569706077537 ) ) ;
#88482 = DIRECTION ( 'NONE',  ( 0.000000000000000000, 0.000000000000000000, 1.000000000000000000 ) ) ;
#88483 = VECTOR ( 'NONE', #6511, 1000.000000000000000 ) ;
#88484 = AXIS2_PLACEMENT_3D ( 'NONE', #41024, #103139, #111003 ) ;
#88485 = VECTOR ( 'NONE', #70300, 1000.000000000000000 ) ;
#88486 = B_SPLINE_CURVE_WITH_KNOTS ( 'NONE', 3,
 ( #42990, #112349, #10890, #82896, #101235, #80318, #12191, #122811, #53435, #102520, #52141, #93351, #22046, #11553, #70482, #73067, #110403, #101883 ),
 .UNSPECIFIED., .F., .F.,
 ( 4, 2, 2, 2, 2, 2, 2, 2, 4 ),
 ( -1.046607274944176980E-05, 0.0004931538261971517897, 0.0009967737251437452407, 0.002004013523036937781, 0.002507633421983534484, 0.002759443371456834354, 0.003011253320930134657, 0.003514873219876733096, 0.004018493118823331968 ),
 .UNSPECIFIED. ) ;
#88487 = AXIS2_PLACEMENT_3D ( 'NONE', #52215, #63313, #22130 ) ;
#88488 = AXIS2_PLACEMENT_3D ( 'NONE', #76068, #127736, #38074 ) ;
#88489 = EDGE_LOOP ( 'NONE', ( #80005, #10462, #106919, #66960 ) ) ;
#88490 = CARTESIAN_POINT ( 'NONE',  ( 184.4166666666666856, 6.668395609140176816, 3.850000000000000977 ) ) ;
#88491 = LINE ( 'NONE', #128450, #22383 ) ;
#88492 = CARTESIAN_POINT ( 'NONE',  ( 8.149999999999920419, 12.50000000000000000, 6.148780366869520897 ) ) ;
#88493 = DIRECTION ( 'NONE',  ( -0.000000000000000000, 1.000000000000000000, -0.000000000000000000 ) ) ;
#88494 = ORIENTED_EDGE ( 'NONE', *, *, #480, .F. ) ;
#88495 = AXIS2_PLACEMENT_3D ( 'NONE', #106811, #28271, #6034 ) ;
#88496 = DIRECTION ( 'NONE',  ( 0.000000000000000000, -0.000000000000000000, 1.000000000000000000 ) ) ;
#88497 = ORIENTED_EDGE ( 'NONE', *, *, #29746, .F. ) ;
#88498 = CARTESIAN_POINT ( 'NONE',  ( 48.67918707175899584, 3.179367830269037132, -5.083100937075674786 ) ) ;
#88499 = PLANE ( 'NONE',  #129285 ) ;
#88500 = DIRECTION ( 'NONE',  ( -0.000000000000000000, 1.000000000000000000, -0.000000000000000000 ) ) ;
#88501 = AXIS2_PLACEMENT_3D ( 'NONE', #15900, #55835, #6075 ) ;
#88502 = ORIENTED_EDGE ( 'NONE', *, *, #64494, .F. ) ;
#88503 = CARTESIAN_POINT ( 'NONE',  ( -5.850000000000019185, 2.500000000000000000, 2.265063509461097357 ) ) ;
#88504 = ORIENTED_EDGE ( 'NONE', *, *, #32600, .F. ) ;
#88505 = CARTESIAN_POINT ( 'NONE',  ( 5.799999999999934985, 12.50000000000000000, -4.330127018922201643 ) ) ;
#88506 = CARTESIAN_POINT ( 'NONE',  ( 10.79999999999991012, 12.50000000000000000, -4.265033745738164406 ) ) ;
#88507 = DIRECTION ( 'NONE',  ( 0.000000000000000000, -0.000000000000000000, 1.000000000000000000 ) ) ;
#88508 = AXIS2_PLACEMENT_3D ( 'NONE', #105891, #33930, #52928 ) ;
#88509 = ORIENTED_EDGE ( 'NONE', *, *, #68407, .F. ) ;
#88510 = CONICAL_SURFACE ( 'NONE', #69743, 0.1000000000000000472, 0.003490658503988666988 ) ;
#88511 = CARTESIAN_POINT ( 'NONE',  ( -2.500000000000032419, 12.50000000000000000, 0.6928203230275494784 ) ) ;
#88512 = CARTESIAN_POINT ( 'NONE',  ( 185.2812500006828031, 0.000000000000000000, 7.700000000000000178 ) ) ;
#88513 = EDGE_CURVE ( 'NONE', #48914, #1889, #101015, .T. ) ;
#88514 = ORIENTED_EDGE ( 'NONE', *, *, #32433, .T. ) ;
#88515 = CARTESIAN_POINT ( 'NONE',  ( -0.6500000000000403233, 12.50000000000000000, 1.818653347947321475 ) ) ;
#88516 = EDGE_CURVE ( 'NONE', #120717, #44822, #127865, .T. ) ;
#88517 = AXIS2_PLACEMENT_3D ( 'NONE', #33964, #73883, #103994 ) ;
#88518 = ORIENTED_EDGE ( 'NONE', *, *, #110702, .F. ) ;
#88519 = AXIS2_PLACEMENT_3D ( 'NONE', #51606, #22800, #123538 ) ;
#88520 = DIRECTION ( 'NONE',  ( 0.000000000000000000, 0.000000000000000000, -1.000000000000000000 ) ) ;
#88521 = VECTOR ( 'NONE', #46897, 1000.000000000000000 ) ;
#88522 = AXIS2_PLACEMENT_3D ( 'NONE', #54364, #2670, #93016 ) ;
#88523 = ORIENTED_EDGE ( 'NONE', *, *, #39975, .F. ) ;
#88524 = DIRECTION ( 'NONE',  ( -4.274815082592931898E-19, -0.9999939076577903929, -0.003490651415223739937 ) ) ;
#88525 = CARTESIAN_POINT ( 'NONE',  ( 10.44999999999991402, 12.50000000000000000, -2.165063509461101710 ) ) ;
#88526 = ORIENTED_EDGE ( 'NONE', *, *, #55259, .T. ) ;
#88527 = ADVANCED_FACE ( 'NONE', ( #53222 ), #119536, .T. ) ;
#88528 = ORIENTED_EDGE ( 'NONE', *, *, #39541, .F. ) ;
#88529 = CIRCLE ( 'NONE', #27905, 0.06509327318403745899 ) ;
#88530 = LINE ( 'NONE', #96408, #86493 ) ;
#88531 = DIRECTION ( 'NONE',  ( -0.000000000000000000, -1.000000000000000000, -0.000000000000000000 ) ) ;
#88532 = ORIENTED_EDGE ( 'NONE', *, *, #43252, .T. ) ;
#88533 = DIRECTION ( 'NONE',  ( -0.000000000000000000, 1.000000000000000000, -0.000000000000000000 ) ) ;
#88534 = CARTESIAN_POINT ( 'NONE',  ( 21.24754738303277435, 0.7337760880902381988, 4.182111650399361835 ) ) ;
#88535 = AXIS2_PLACEMENT_3D ( 'NONE', #89959, #103668, #13969 ) ;
#88537 = AXIS2_PLACEMENT_3D ( 'NONE', #76877, #54016, #84763 ) ;
#88536 = DIRECTION ( 'NONE',  ( -0.000000000000000000, 1.000000000000000000, -0.000000000000000000 ) ) ;
#88538 = VECTOR ( 'NONE', #81661, 1000.000000000000000 ) ;
#88539 = CARTESIAN_POINT ( 'NONE',  ( 104.0382667140819990, 8.146203828384356527, -3.067605667726266194 ) ) ;
#88540 = DIRECTION ( 'NONE',  ( 0.000000000000000000, 0.000000000000000000, 1.000000000000000000 ) ) ;
#88541 = CARTESIAN_POINT ( 'NONE',  ( 6.249999999999930722, 2.500000000000000000, 1.472243186433545459 ) ) ;
#88542 = VECTOR ( 'NONE', #105782, 1000.000000000000000 ) ;
#88543 = DIRECTION ( 'NONE',  ( 0.000000000000000000, 1.000000000000000000, 0.000000000000000000 ) ) ;
#88544 = AXIS2_PLACEMENT_3D ( 'NONE', #13983, #5453, #4803 ) ;
#88545 = ORIENTED_EDGE ( 'NONE', *, *, #98026, .F. ) ;
#88547 = ORIENTED_EDGE ( 'NONE', *, *, #82078, .F. ) ;
#88546 = EDGE_CURVE ( 'NONE', #91772, #108234, #23394, .T. ) ;
#88548 = EDGE_LOOP ( 'NONE', ( #116973, #99162 ) ) ;
#88549 = EDGE_LOOP ( 'NONE', ( #50675, #40801, #111033, #1218 ) ) ;
#88550 = CARTESIAN_POINT ( 'NONE',  ( -8.350000000000013856, 2.500000000000000000, 2.165063509461097713 ) ) ;
#88551 = CARTESIAN_POINT ( 'NONE',  ( 5.849999999999933920, 12.50000000000000000, -2.857883832488653741 ) ) ;
#88552 = DIRECTION ( 'NONE',  ( -4.274815082592931898E-19, -0.9999939076577903929, -0.003490651415223739937 ) ) ;
#88553 = ORIENTED_EDGE ( 'NONE', *, *, #65098, .F. ) ;
#88554 = FACE_BOUND ( 'NONE', #52429, .T. ) ;
#88555 = ORIENTED_EDGE ( 'NONE', *, *, #119478, .T. ) ;
#88556 = DIRECTION ( 'NONE',  ( 0.000000000000000000, 0.000000000000000000, -1.000000000000000000 ) ) ;
#88557 = CARTESIAN_POINT ( 'NONE',  ( -4.200000000000025935, 2.500000000000000000, -2.385244779468109755E-15 ) ) ;
#88559 = EDGE_CURVE ( 'NONE', #91737, #33523, #79835, .T. ) ;
#88558 = CARTESIAN_POINT ( 'NONE',  ( -8.100000000000013856, 12.50000000000000000, -0.2813168883297408329 ) ) ;
#88560 = CARTESIAN_POINT ( 'NONE',  ( -6.250000000000015987, 2.500000000000000000, 5.802370205355744659 ) ) ;
#88561 = LINE ( 'NONE', #60427, #98803 ) ;
#88562 = DIRECTION ( 'NONE',  ( -0.000000000000000000, -1.000000000000000000, -0.000000000000000000 ) ) ;
#88563 = DIRECTION ( 'NONE',  ( 0.000000000000000000, 0.000000000000000000, 1.000000000000000000 ) ) ;
#88564 = CARTESIAN_POINT ( 'NONE',  ( 14.99999999999989342, 12.50000000000000000, -0.6928203230275541413 ) ) ;
#88565 = CIRCLE ( 'NONE', #25875, 0.1000000000000002554 ) ;
#88566 = EDGE_CURVE ( 'NONE', #127598, #92529, #66881, .T. ) ;
#88567 = CIRCLE ( 'NONE', #101089, 0.1000000000000002554 ) ;
#88568 = EDGE_CURVE ( 'NONE', #66767, #74569, #107007, .T. ) ;
#88569 = DIRECTION ( 'NONE',  ( 0.000000000000000000, 0.000000000000000000, 1.000000000000000000 ) ) ;
#88570 = ADVANCED_FACE ( 'NONE', ( #37447 ), #74789, .T. ) ;
#88571 = EDGE_CURVE ( 'NONE', #119467, #101350, #15189, .T. ) ;
#88572 = DIRECTION ( 'NONE',  ( -0.000000000000000000, -1.000000000000000000, -0.000000000000000000 ) ) ;
#88573 = CONICAL_SURFACE ( 'NONE', #71865, 0.1000000000000002554, 0.003490658503988666988 ) ;
#88574 = EDGE_LOOP ( 'NONE', ( #87664, #98872 ) ) ;
#88575 = ORIENTED_EDGE ( 'NONE', *, *, #117108, .F. ) ;
#88576 = ORIENTED_EDGE ( 'NONE', *, *, #13238, .T. ) ;
#88577 = AXIS2_PLACEMENT_3D ( 'NONE', #40444, #19483, #101276 ) ;
#88578 = ORIENTED_EDGE ( 'NONE', *, *, #68646, .T. ) ;
#88579 = CARTESIAN_POINT ( 'NONE',  ( 17.41715230668671310, -1.872943439149598710, -4.643388583737356079 ) ) ;
#88580 = EDGE_CURVE ( 'NONE', #113146, #117732, #12918, .T. ) ;
#88581 = AXIS2_PLACEMENT_3D ( 'NONE', #110838, #11359, #111487 ) ;
#88582 = CARTESIAN_POINT ( 'NONE',  ( 9.149999999999920419, 12.50000000000000000, -5.802370205355749988 ) ) ;
#88585 = ORIENTED_EDGE ( 'NONE', *, *, #14129, .T. ) ;
#88584 = ORIENTED_EDGE ( 'NONE', *, *, #19427, .F. ) ;
#88583 = ADVANCED_FACE ( 'NONE', ( #54488 ), #6637, .T. ) ;
#88586 = ORIENTED_EDGE ( 'NONE', *, *, #28589, .T. ) ;
#88587 = CARTESIAN_POINT ( 'NONE',  ( 185.0833333333333144, -6.668395609140180369, 3.849999999999994760 ) ) ;
#88588 = AXIS2_PLACEMENT_3D ( 'NONE', #1881, #92863, #62755 ) ;
#88589 = ADVANCED_FACE ( 'NONE', ( #5388 ), #96996, .T. ) ;
#88590 = AXIS2_PLACEMENT_3D ( 'NONE', #115284, #14383, #124366 ) ;
#88591 = CIRCLE ( 'NONE', #94847, 0.1000000000000002554 ) ;
#88592 = EDGE_CURVE ( 'NONE', #80576, #53022, #94407, .T. ) ;
#88593 = DIRECTION ( 'NONE',  ( 0.000000000000000000, 1.000000000000000000, 0.000000000000000000 ) ) ;
#88594 = CARTESIAN_POINT ( 'NONE',  ( -4.150000000000027889, 2.500000000000000000, -6.495190528383302464 ) ) ;
#88595 = CARTESIAN_POINT ( 'NONE',  ( -7.950000000000012612, 12.50000000000000000, -2.099970236277064473 ) ) ;
#88596 = LINE ( 'NONE', #28394, #26266 ) ;
#88597 = DIRECTION ( 'NONE',  ( 0.000000000000000000, 0.000000000000000000, 1.000000000000000000 ) ) ;
#88598 = AXIS2_PLACEMENT_3D ( 'NONE', #25499, #62872, #65433 ) ;
#88599 = DIRECTION ( 'NONE',  ( 0.000000000000000000, 0.000000000000000000, -1.000000000000000000 ) ) ;
#88600 = ORIENTED_EDGE ( 'NONE', *, *, #41795, .F. ) ;
#88601 = ADVANCED_FACE ( 'NONE', ( #56419 ), #125173, .T. ) ;
#88602 = DIRECTION ( 'NONE',  ( 0.000000000000000000, 0.000000000000000000, 1.000000000000000000 ) ) ;
#88603 = ORIENTED_EDGE ( 'NONE', *, *, #3868, .T. ) ;
#88604 = ORIENTED_EDGE ( 'NONE', *, *, #88546, .T. ) ;
#88605 = VERTEX_POINT ( 'NONE', #4724 ) ;
#88606 = DIRECTION ( 'NONE',  ( 0.000000000000000000, 0.000000000000000000, 1.000000000000000000 ) ) ;
#88607 = VERTEX_POINT ( 'NONE', #7313 ) ;
#88608 = ORIENTED_EDGE ( 'NONE', *, *, #45608, .F. ) ;
#88609 = CIRCLE ( 'NONE', #9092, 0.1000000000000002554 ) ;
#88610 = DIRECTION ( 'NONE',  ( 0.000000000000000000, 0.000000000000000000, 1.000000000000000000 ) ) ;
#88611 = FACE_OUTER_BOUND ( 'NONE', #122838, .T. ) ;
#88612 = CARTESIAN_POINT ( 'NONE',  ( -10.00000000000000533, 12.50000000000000000, -5.088040615133786915 ) ) ;
#88613 = DIRECTION ( 'NONE',  ( 0.000000000000000000, 0.000000000000000000, 1.000000000000000000 ) ) ;
#88614 = DIRECTION ( 'NONE',  ( 0.000000000000000000, 1.000000000000000000, 0.000000000000000000 ) ) ;
#88616 = ORIENTED_EDGE ( 'NONE', *, *, #74885, .F. ) ;
#88615 = VECTOR ( 'NONE', #85444, 1000.000000000000000 ) ;
#88617 = FACE_OUTER_BOUND ( 'NONE', #102010, .T. ) ;
#88618 = AXIS2_PLACEMENT_3D ( 'NONE', #43330, #124456, #44605 ) ;
#88619 = VECTOR ( 'NONE', #104143, 1000.000000000000000 ) ;
#88620 = ORIENTED_EDGE ( 'NONE', *, *, #9037, .F. ) ;
#88621 = CARTESIAN_POINT ( 'NONE',  ( 21.25104915410168971, -0.2454763298545039607, 4.189301388122809833 ) ) ;
#88622 = EDGE_LOOP ( 'NONE', ( #68824, #5569 ) ) ;
#88623 = CARTESIAN_POINT ( 'NONE',  ( 111.0559149355470936, 7.743809555462367378, 3.970544583781440373 ) ) ;
#88624 = FACE_OUTER_BOUND ( 'NONE', #97062, .T. ) ;
#88625 = EDGE_LOOP ( 'NONE', ( #96631, #70963, #128240, #26064 ) ) ;
#88626 = DIRECTION ( 'NONE',  ( 0.000000000000000000, 1.000000000000000000, 0.000000000000000000 ) ) ;
#88627 = CARTESIAN_POINT ( 'NONE',  ( 108.0000000000000142, 8.500000000000000000, -4.500000000000003553 ) ) ;
#88628 = ORIENTED_EDGE ( 'NONE', *, *, #120342, .F. ) ;
#88629 = AXIS2_PLACEMENT_3D ( 'NONE', #85990, #86656, #95840 ) ;
#88630 = CIRCLE ( 'NONE', #99107, 0.06509327318403745899 ) ;
#88631 = EDGE_CURVE ( 'NONE', #58954, #128192, #73561, .T. ) ;
#88632 = DIRECTION ( 'NONE',  ( -0.000000000000000000, 1.000000000000000000, -0.000000000000000000 ) ) ;
#88633 = EDGE_CURVE ( 'NONE', #71810, #4409, #10854, .T. ) ;
#88634 = EDGE_LOOP ( 'NONE', ( #107835, #14714, #57092, #68173 ) ) ;
#88635 = ORIENTED_EDGE ( 'NONE', *, *, #11478, .T. ) ;
#88636 = DIRECTION ( 'NONE',  ( 0.000000000000000000, 0.000000000000000000, 1.000000000000000000 ) ) ;
#88637 = DIRECTION ( 'NONE',  ( 0.000000000000000000, 0.000000000000000000, 1.000000000000000000 ) ) ;
#88638 = DIRECTION ( 'NONE',  ( -0.000000000000000000, -1.000000000000000000, -0.000000000000000000 ) ) ;
#88639 = CARTESIAN_POINT ( 'NONE',  ( 6.649999999999930189, 2.500000000000000000, -2.857883832488653741 ) ) ;
#88640 = PLANE ( 'NONE',  #43726 ) ;
#88641 = ORIENTED_EDGE ( 'NONE', *, *, #109988, .T. ) ;
#88642 = AXIS2_PLACEMENT_3D ( 'NONE', #67579, #107522, #78059 ) ;
#88643 = AXIS2_PLACEMENT_3D ( 'NONE', #91616, #13033, #41892 ) ;
#88644 = AXIS2_PLACEMENT_3D ( 'NONE', #50139, #41612, #90025 ) ;
#88645 = CARTESIAN_POINT ( 'NONE',  ( 8.549999999999920774, 12.50000000000000000, -2.446380397790840266 ) ) ;
#88646 = AXIS2_PLACEMENT_3D ( 'NONE', #34329, #104954, #46067 ) ;
#88647 = EDGE_LOOP ( 'NONE', ( #77273, #11924 ) ) ;
#88648 = CONICAL_SURFACE ( 'NONE', #38499, 0.09999999999999982514, 0.003490658503988666988 ) ;
#88649 = LINE ( 'NONE', #29104, #111311 ) ;
#88650 = DIRECTION ( 'NONE',  ( 0.000000000000000000, 0.000000000000000000, -1.000000000000000000 ) ) ;
#88651 = ORIENTED_EDGE ( 'NONE', *, *, #102290, .T. ) ;
#88652 = DIRECTION ( 'NONE',  ( 0.000000000000000000, -0.000000000000000000, 1.000000000000000000 ) ) ;
#88653 = CARTESIAN_POINT ( 'NONE',  ( 127.5000000000000000, 1.500000000000000000, 6.000000000000000000 ) ) ;
#88654 = PLANE ( 'NONE',  #67367 ) ;
#88655 = DIRECTION ( 'NONE',  ( 0.000000000000000000, 0.000000000000000000, 1.000000000000000000 ) ) ;
#88656 = CARTESIAN_POINT ( 'NONE',  ( 14.59999999999989484, 2.500000000000000000, 0.7928203230275495672 ) ) ;
#88657 = VERTEX_POINT ( 'NONE', #115316 ) ;
#88658 = CARTESIAN_POINT ( 'NONE',  ( 11.04999999999991012, 2.500000000000000000, -1.918653347947326004 ) ) ;
#88659 = CARTESIAN_POINT ( 'NONE',  ( -5.400000000000019895, 2.500000000000000000, 0.09999999999999772959 ) ) ;
#88660 = DIRECTION ( 'NONE',  ( 0.000000000000000000, 0.000000000000000000, 1.000000000000000000 ) ) ;
#88661 = CIRCLE ( 'NONE', #126321, 0.06509327318403745899 ) ;
#88662 = VECTOR ( 'NONE', #71072, 1000.000000000000000 ) ;
#88663 = AXIS2_PLACEMENT_3D ( 'NONE', #121560, #52837, #61376 ) ;
#88664 = ORIENTED_EDGE ( 'NONE', *, *, #4672, .T. ) ;
#88665 = CARTESIAN_POINT ( 'NONE',  ( -2.300000000000032685, 2.500000000000000000, -0.2464101615137783419 ) ) ;
#88666 = ADVANCED_FACE ( 'NONE', ( #25039 ), #14955, .T. ) ;
#88667 = AXIS2_PLACEMENT_3D ( 'NONE', #57116, #106229, #46663 ) ;
#88668 = AXIS2_PLACEMENT_3D ( 'NONE', #71091, #110989, #20706 ) ;
#88669 = VERTEX_POINT ( 'NONE', #127117 ) ;
#88670 = CIRCLE ( 'NONE', #111667, 0.1000000000000000472 ) ;
#88671 = ORIENTED_EDGE ( 'NONE', *, *, #15461, .F. ) ;
#88672 = CARTESIAN_POINT ( 'NONE',  ( -13.09999999999999076, 2.500000000000000000, 4.776537180435972196 ) ) ;
#88673 = CONICAL_SURFACE ( 'NONE', #92798, 0.1000000000000002554, 0.003490658503988666988 ) ;
#88674 = VERTEX_POINT ( 'NONE', #15847 ) ;
#88675 = DIRECTION ( 'NONE',  ( 1.000000000000000000, 0.000000000000000000, 0.000000000000000000 ) ) ;
#88676 = FACE_OUTER_BOUND ( 'NONE', #98553, .T. ) ;
#88678 = VERTEX_POINT ( 'NONE', #25673 ) ;
#88677 = AXIS2_PLACEMENT_3D ( 'NONE', #67211, #8318, #46982 ) ;
#88679 = AXIS2_PLACEMENT_3D ( 'NONE', #22805, #70596, #12939 ) ;
#88680 = CARTESIAN_POINT ( 'NONE',  ( -8.750000000000010658, 2.500000000000000000, -7.188010851410848723 ) ) ;
#88682 = ORIENTED_EDGE ( 'NONE', *, *, #53824, .F. ) ;
#88681 = DIRECTION ( 'NONE',  ( 0.000000000000000000, 1.000000000000000000, 0.000000000000000000 ) ) ;
#88683 = AXIS2_PLACEMENT_3D ( 'NONE', #69292, #111824, #99433 ) ;
#88684 = EDGE_CURVE ( 'NONE', #93998, #118854, #36803, .T. ) ;
#88685 = DIRECTION ( 'NONE',  ( 0.000000000000000000, 1.000000000000000000, 0.000000000000000000 ) ) ;
#88686 = CARTESIAN_POINT ( 'NONE',  ( -2.300000000000032685, 2.500000000000000000, -4.576537180435978236 ) ) ;
#88687 = EDGE_CURVE ( 'NONE', #78285, #93896, #86072, .T. ) ;
#88688 = VERTEX_POINT ( 'NONE', #124536 ) ;
#88689 = ORIENTED_EDGE ( 'NONE', *, *, #127338, .F. ) ;
#88690 = VERTEX_POINT ( 'NONE', #55785 ) ;
#88691 = FACE_OUTER_BOUND ( 'NONE', #114179, .T. ) ;
#88692 = DIRECTION ( 'NONE',  ( -0.000000000000000000, -1.000000000000000000, -0.000000000000000000 ) ) ;
#88693 = DIRECTION ( 'NONE',  ( -0.000000000000000000, -1.000000000000000000, -0.000000000000000000 ) ) ;
#88694 = ADVANCED_FACE ( 'NONE', ( #45979 ), #85867, .T. ) ;
#88695 = FACE_BOUND ( 'NONE', #80758, .T. ) ;
#88696 = ORIENTED_EDGE ( 'NONE', *, *, #107874, .F. ) ;
#88697 = DIRECTION ( 'NONE',  ( -4.274815082592931898E-19, -0.9999939076577903929, -0.003490651415223739937 ) ) ;
#88698 = CARTESIAN_POINT ( 'NONE',  ( -9.350000000000006750, 2.500000000000000000, -1.718653347947325827 ) ) ;
#88699 = AXIS2_PLACEMENT_3D ( 'NONE', #70024, #128309, #79829 ) ;
#88700 = VERTEX_POINT ( 'NONE', #129060 ) ;
#88701 = DIRECTION ( 'NONE',  ( 0.000000000000000000, -0.9999939076577903929, 0.003490651415223739937 ) ) ;
#88702 = DIRECTION ( 'NONE',  ( 0.000000000000000000, 1.000000000000000000, 0.000000000000000000 ) ) ;
#88703 = DIRECTION ( 'NONE',  ( 0.000000000000000000, 0.000000000000000000, 1.000000000000000000 ) ) ;
#88704 = CARTESIAN_POINT ( 'NONE',  ( 5.449999999999936229, 12.50000000000000000, 6.495190528383297135 ) ) ;
#88705 = DIRECTION ( 'NONE',  ( 0.000000000000000000, 0.000000000000000000, 1.000000000000000000 ) ) ;
#88706 = CARTESIAN_POINT ( 'NONE',  ( 3.149999999999942624, 2.500000000000000000, 6.148780366869520897 ) ) ;
#88707 = CARTESIAN_POINT ( 'NONE',  ( -6.083778633910298187E-15, 2.500000000000000000, -4.430127018922202176 ) ) ;
#88708 = CIRCLE ( 'NONE', #34354, 0.1000000000000000472 ) ;
#88709 = AXIS2_PLACEMENT_3D ( 'NONE', #41862, #81759, #121686 ) ;
#88710 = VERTEX_POINT ( 'NONE', #118561 ) ;
#88711 = ORIENTED_EDGE ( 'NONE', *, *, #41935, .T. ) ;
#88712 = ORIENTED_EDGE ( 'NONE', *, *, #83322, .F. ) ;
#88713 = VERTEX_POINT ( 'NONE', #90377 ) ;
#88714 = ORIENTED_EDGE ( 'NONE', *, *, #76440, .F. ) ;
#88715 = CARTESIAN_POINT ( 'NONE',  ( -1.450000000000035927, 2.500000000000000000, -6.148780366869526226 ) ) ;
#88716 = DIRECTION ( 'NONE',  ( 0.000000000000000000, 1.000000000000000000, 0.000000000000000000 ) ) ;
#88717 = EDGE_LOOP ( 'NONE', ( #8505, #45248, #63745 ) ) ;
#88718 = FACE_BOUND ( 'NONE', #129047, .T. ) ;
#88719 = FACE_OUTER_BOUND ( 'NONE', #47565, .T. ) ;
#88720 = VECTOR ( 'NONE', #121341, 1000.000000000000000 ) ;
#88721 = ADVANCED_FACE ( 'NONE', ( #110044 ), #77, .T. ) ;
#88722 = CARTESIAN_POINT ( 'NONE',  ( 11.89999999999990443, 12.50000000000000000, 0.4115034346978110880 ) ) ;
#88723 = DIRECTION ( 'NONE',  ( 0.000000000000000000, -0.9999939076577903929, 0.003490651415223739937 ) ) ;
#88724 = DIRECTION ( 'NONE',  ( 0.000000000000000000, 0.000000000000000000, -1.000000000000000000 ) ) ;
#88725 = EDGE_CURVE ( 'NONE', #95323, #69394, #42192, .T. ) ;
#88726 = FACE_OUTER_BOUND ( 'NONE', #20738, .T. ) ;
#88727 = ORIENTED_EDGE ( 'NONE', *, *, #111728, .T. ) ;
#88728 = EDGE_CURVE ( 'NONE', #52632, #58166, #17105, .T. ) ;
#88729 = ORIENTED_EDGE ( 'NONE', *, *, #41881, .T. ) ;
#88730 = AXIS2_PLACEMENT_3D ( 'NONE', #96241, #83848, #84509 ) ;
#88731 = ORIENTED_EDGE ( 'NONE', *, *, #52775, .T. ) ;
#88732 = ORIENTED_EDGE ( 'NONE', *, *, #53995, .T. ) ;
#88733 = ADVANCED_FACE ( 'NONE', ( #107461 ), #19179, .T. ) ;
#88734 = CARTESIAN_POINT ( 'NONE',  ( 6.899999999999928413, 2.500000000000000000, -4.083716857408426826 ) ) ;
#88736 = EDGE_CURVE ( 'NONE', #61895, #63523, #63109, .T. ) ;
#88735 = CARTESIAN_POINT ( 'NONE',  ( 3.677302434130802933, 2.500000000000000444, 9.000000000000007105 ) ) ;
#88738 = AXIS2_PLACEMENT_3D ( 'NONE', #32243, #42712, #80029 ) ;
#88737 = FACE_OUTER_BOUND ( 'NONE', #24042, .T. ) ;
#88740 = EDGE_LOOP ( 'NONE', ( #20255, #10449 ) ) ;
#88739 = EDGE_CURVE ( 'NONE', #82776, #44898, #2458, .T. ) ;
#88741 = FACE_OUTER_BOUND ( 'NONE', #14636, .T. ) ;
#88742 = AXIS2_PLACEMENT_3D ( 'NONE', #74367, #77570, #107027 ) ;
#88743 = CARTESIAN_POINT ( 'NONE',  ( 12.89999999999990088, 12.50000000000000000, -4.265033745738164406 ) ) ;
#88745 = EDGE_CURVE ( 'NONE', #92207, #45669, #35920, .T. ) ;
#88744 = DIRECTION ( 'NONE',  ( -0.000000000000000000, -1.000000000000000000, -0.000000000000000000 ) ) ;
#88746 = CARTESIAN_POINT ( 'NONE',  ( 184.4843750003414016, -8.734944146203032389, -1.604583208406768146E-15 ) ) ;
#88747 = DIRECTION ( 'NONE',  ( 0.000000000000000000, 1.000000000000000000, 0.000000000000000000 ) ) ;
#88748 = CARTESIAN_POINT ( 'NONE',  ( 11.24999999999991118, 12.50000000000000000, 5.802370205355744659 ) ) ;
#88749 = PLANE ( 'NONE',  #116558 ) ;
#88750 = VERTEX_POINT ( 'NONE', #30211 ) ;
#88751 = DIRECTION ( 'NONE',  ( 0.000000000000000000, 1.000000000000000000, 0.000000000000000000 ) ) ;
#88752 = ADVANCED_FACE ( 'NONE', ( #70126 ), #52982, .T. ) ;
#88753 = ORIENTED_EDGE ( 'NONE', *, *, #6841, .T. ) ;
#88755 = ORIENTED_EDGE ( 'NONE', *, *, #19733, .T. ) ;
#88754 = CIRCLE ( 'NONE', #80639, 0.1000000000000002554 ) ;
#88756 = DIRECTION ( 'NONE',  ( -0.000000000000000000, 1.000000000000000000, -0.000000000000000000 ) ) ;
#88757 = CIRCLE ( 'NONE', #49064, 0.06509327318403745899 ) ;
#88758 = CARTESIAN_POINT ( 'NONE',  ( 0.1999999999999562961, 2.500000000000000000, 4.776537180435972196 ) ) ;
#88759 = CONICAL_SURFACE ( 'NONE', #21876, 0.1000000000000000472, 0.003490658503988666988 ) ;
#88760 = PLANE ( 'NONE',  #10648 ) ;
#88761 = ORIENTED_EDGE ( 'NONE', *, *, #67449, .T. ) ;
#88762 = EDGE_LOOP ( 'NONE', ( #10179, #79224, #85333, #18520 ) ) ;
#88763 = CARTESIAN_POINT ( 'NONE',  ( 184.8229166673494888, -4.445597072760063107, 7.700000000000102318 ) ) ;
#88764 = VECTOR ( 'NONE', #26148, 1000.000000000000000 ) ;
#88765 = AXIS2_PLACEMENT_3D ( 'NONE', #127058, #37392, #115260 ) ;
#88766 = CIRCLE ( 'NONE', #105498, 0.1000000000000002554 ) ;
#88767 = CARTESIAN_POINT ( 'NONE',  ( 8.349999999999919709, 2.500000000000000000, 6.395190528383296602 ) ) ;
#88768 = CARTESIAN_POINT ( 'NONE',  ( 1.049999999999952083, 2.500000000000000000, 6.741600689897071952 ) ) ;
#88769 = ORIENTED_EDGE ( 'NONE', *, *, #103066, .T. ) ;
#88770 = ORIENTED_EDGE ( 'NONE', *, *, #30240, .F. ) ;
#88771 = CONICAL_SURFACE ( 'NONE', #28426, 0.1000000000000002554, 0.003490658503988666988 ) ;
#88772 = DIRECTION ( 'NONE',  ( 0.000000000000000000, 1.000000000000000000, 0.000000000000000000 ) ) ;
#88773 = ORIENTED_EDGE ( 'NONE', *, *, #77914, .T. ) ;
#88774 = DIRECTION ( 'NONE',  ( 0.000000000000000000, 1.000000000000000000, 0.000000000000000000 ) ) ;
#88775 = AXIS2_PLACEMENT_3D ( 'NONE', #46278, #76399, #6975 ) ;
#88776 = CIRCLE ( 'NONE', #28139, 0.06509327318403745899 ) ;
#88777 = ORIENTED_EDGE ( 'NONE', *, *, #102232, .F. ) ;
#88778 = CARTESIAN_POINT ( 'NONE',  ( 0.3999999999999619971, 2.500000000000000000, -1.084202172485504434E-16 ) ) ;
#88779 = DIRECTION ( 'NONE',  ( 0.000000000000000000, -0.9999939076577903929, 0.003490651415223739937 ) ) ;
#88780 = DIRECTION ( 'NONE',  ( -0.000000000000000000, -1.000000000000000000, -0.000000000000000000 ) ) ;
#88781 = CONICAL_SURFACE ( 'NONE', #84575, 0.1000000000000002554, 0.003490658503988666988 ) ;
#88782 = DIRECTION ( 'NONE',  ( 0.000000000000000000, 0.000000000000000000, -1.000000000000000000 ) ) ;
#88783 = VERTEX_POINT ( 'NONE', #68170 ) ;
#88784 = FACE_OUTER_BOUND ( 'NONE', #64191, .T. ) ;
#88785 = ADVANCED_FACE ( 'NONE', ( #10533 ), #71866, .T. ) ;
#88786 = VERTEX_POINT ( 'NONE', #50469 ) ;
#88787 = ORIENTED_EDGE ( 'NONE', *, *, #97812, .F. ) ;
#88788 = CARTESIAN_POINT ( 'NONE',  ( 0.5999999999999551248, 2.500000000000000000, -4.776537180435978414 ) ) ;
#88789 = DIRECTION ( 'NONE',  ( 0.000000000000000000, 1.000000000000000000, 0.000000000000000000 ) ) ;
#88790 = CARTESIAN_POINT ( 'NONE',  ( 12.89999999999990266, 12.50000000000000000, 3.637306695894644726 ) ) ;
#88791 = DIRECTION ( 'NONE',  ( -0.000000000000000000, 1.000000000000000000, -0.000000000000000000 ) ) ;
#88792 = CIRCLE ( 'NONE', #107575, 0.06509327318403745899 ) ;
#88793 = DIRECTION ( 'NONE',  ( -0.000000000000000000, -1.000000000000000000, -0.000000000000000000 ) ) ;
#88794 = PLANE ( 'NONE',  #115488 ) ;
#88795 = EDGE_CURVE ( 'NONE', #124254, #1046, #21690, .T. ) ;
#88796 = FACE_OUTER_BOUND ( 'NONE', #68650, .T. ) ;
#88797 = DIRECTION ( 'NONE',  ( 0.000000000000000000, 0.000000000000000000, -1.000000000000000000 ) ) ;
#88798 = DIRECTION ( 'NONE',  ( -0.000000000000000000, -1.000000000000000000, -0.000000000000000000 ) ) ;
#88799 = VECTOR ( 'NONE', #77600, 1000.000000000000000 ) ;
#88800 = AXIS2_PLACEMENT_3D ( 'NONE', #122833, #43643, #80978 ) ;
#88801 = ORIENTED_EDGE ( 'NONE', *, *, #122307, .F. ) ;
#88802 = CARTESIAN_POINT ( 'NONE',  ( 1.049999999999954081, 12.50000000000000000, -6.148780366869526226 ) ) ;
#88803 = DIRECTION ( 'NONE',  ( 0.000000000000000000, 0.000000000000000000, -1.000000000000000000 ) ) ;
#88804 = CARTESIAN_POINT ( 'NONE',  ( 3.749999999999978684, 2.500000000000000000, -6.595190528383302109 ) ) ;
#88805 = CARTESIAN_POINT ( 'NONE',  ( -14.99999999999994671, 2.500000000000000000, 0.1000000000000000056 ) ) ;
#88806 = DIRECTION ( 'NONE',  ( 0.000000000000000000, 0.000000000000000000, 1.000000000000000000 ) ) ;
#88807 = EDGE_LOOP ( 'NONE', ( #74720, #23476, #83510, #115922 ) ) ;
#88808 = DIRECTION ( 'NONE',  ( 0.000000000000000000, 0.000000000000000000, 1.000000000000000000 ) ) ;
#88809 = AXIS2_PLACEMENT_3D ( 'NONE', #6068, #25719, #85287 ) ;
#88810 = AXIS2_PLACEMENT_3D ( 'NONE', #12399, #61529, #22889 ) ;
#88811 = DIRECTION ( 'NONE',  ( 0.000000000000000000, 1.000000000000000000, 0.000000000000000000 ) ) ;
#88813 = ORIENTED_EDGE ( 'NONE', *, *, #39050, .T. ) ;
#88812 = DIRECTION ( 'NONE',  ( 0.000000000000000000, 0.000000000000000000, -1.000000000000000000 ) ) ;
#88814 = EDGE_LOOP ( 'NONE', ( #106228, #41769 ) ) ;
#88815 = CARTESIAN_POINT ( 'NONE',  ( -13.94999999999998685, 2.500000000000000000, 1.718653347947325383 ) ) ;
#88816 = EDGE_CURVE ( 'NONE', #101430, #110184, #59358, .T. ) ;
#88817 = CIRCLE ( 'NONE', #17704, 0.06509327318403745899 ) ;
#88818 = ORIENTED_EDGE ( 'NONE', *, *, #2929, .F. ) ;
#88819 = VERTEX_POINT ( 'NONE', #40682 ) ;
#88820 = ORIENTED_EDGE ( 'NONE', *, *, #121284, .T. ) ;
#88821 = CARTESIAN_POINT ( 'NONE',  ( -6.505213034913026604E-15, 2.500000000000000000, 4.330127018922196314 ) ) ;
#88822 = DIRECTION ( 'NONE',  ( 0.000000000000000000, 0.000000000000000000, 1.000000000000000000 ) ) ;
#88823 = DIRECTION ( 'NONE',  ( 0.000000000000000000, -0.000000000000000000, 1.000000000000000000 ) ) ;
#88824 = AXIS2_PLACEMENT_3D ( 'NONE', #40247, #101092, #120098 ) ;
#88825 = CARTESIAN_POINT ( 'NONE',  ( -0.6000000000000323963, 12.50000000000000000, -0.3464101615137759604 ) ) ;
#88826 = EDGE_CURVE ( 'NONE', #22678, #111655, #28916, .T. ) ;
#88827 = EDGE_LOOP ( 'NONE', ( #72583, #80404, #96969, #126191 ) ) ;
#88828 = DIRECTION ( 'NONE',  ( 0.000000000000000000, -0.000000000000000000, 1.000000000000000000 ) ) ;
#88829 = VERTEX_POINT ( 'NONE', #17781 ) ;
#88830 = DIRECTION ( 'NONE',  ( 0.000000000000000000, 0.000000000000000000, -1.000000000000000000 ) ) ;
#88831 = DIRECTION ( 'NONE',  ( -0.000000000000000000, -1.000000000000000000, -0.000000000000000000 ) ) ;
#88832 = ADVANCED_FACE ( 'NONE', ( #57731 ), #119880, .T. ) ;
#88833 = CARTESIAN_POINT ( 'NONE',  ( 17.17161331427190873, 0.4678040054246561663, 5.513957101009332007 ) ) ;
#88834 = DIRECTION ( 'NONE',  ( -0.000000000000000000, 1.000000000000000000, -0.000000000000000000 ) ) ;
#88835 = CARTESIAN_POINT ( 'NONE',  ( -3.300000000000027800, 2.500000000000000000, -4.230127018922201998 ) ) ;
#88836 = EDGE_CURVE ( 'NONE', #76998, #11828, #109415, .T. ) ;
#88837 = ORIENTED_EDGE ( 'NONE', *, *, #19730, .T. ) ;
#88838 = AXIS2_PLACEMENT_3D ( 'NONE', #60158, #58847, #51615 ) ;
#88839 = EDGE_LOOP ( 'NONE', ( #119235, #79683 ) ) ;
#88841 = ORIENTED_EDGE ( 'NONE', *, *, #49430, .F. ) ;
#88840 = EDGE_CURVE ( 'NONE', #60021, #46396, #38080, .T. ) ;
#88842 = EDGE_LOOP ( 'NONE', ( #96255, #86923 ) ) ;
#88843 = VERTEX_POINT ( 'NONE', #38754 ) ;
#88844 = DIRECTION ( 'NONE',  ( -0.000000000000000000, -1.000000000000000000, -0.000000000000000000 ) ) ;
#88845 = DIRECTION ( 'NONE',  ( -0.000000000000000000, 1.000000000000000000, -0.000000000000000000 ) ) ;
#88846 = CIRCLE ( 'NONE', #105578, 0.09999999999999982514 ) ;
#88847 = CARTESIAN_POINT ( 'NONE',  ( 2.949999999999946887, 2.500000000000000000, -2.165063509461101710 ) ) ;
#88848 = ADVANCED_FACE ( 'NONE', ( #68822 ), #36274, .T. ) ;
#88849 = FACE_BOUND ( 'NONE', #117785, .T. ) ;
#88850 = CARTESIAN_POINT ( 'NONE',  ( -11.64999999999999680, 2.500000000000000000, 2.857883832488649301 ) ) ;
#88851 = CARTESIAN_POINT ( 'NONE',  ( 186.3645833340161175, -6.668395609140180369, 3.849999999999994760 ) ) ;
#88852 = CARTESIAN_POINT ( 'NONE',  ( -0.8500000000000382805, 2.500000000000000000, -5.802370205355749988 ) ) ;
#88853 = FACE_OUTER_BOUND ( 'NONE', #99209, .T. ) ;
#88854 = AXIS2_PLACEMENT_3D ( 'NONE', #77018, #17432, #86832 ) ;
#88855 = AXIS2_PLACEMENT_3D ( 'NONE', #13702, #53642, #31435 ) ;
#88856 = CIRCLE ( 'NONE', #47013, 0.06509327318403745899 ) ;
#88857 = CARTESIAN_POINT ( 'NONE',  ( 2.499999999999947153, 2.500000000000000000, 0.6928203230275494784 ) ) ;
#88858 = TOROIDAL_SURFACE ( 'NONE', #26172, 4.000000000000000000, 1.000000000000000000 ) ;
#88859 = CARTESIAN_POINT ( 'NONE',  ( -7.900000000000014566, 2.500000000000000000, 0.7928203230275495672 ) ) ;
#88860 = DIRECTION ( 'NONE',  ( 0.000000000000000000, 0.000000000000000000, 1.000000000000000000 ) ) ;
#88861 = AXIS2_PLACEMENT_3D ( 'NONE', #105039, #33116, #103774 ) ;
#88862 = CIRCLE ( 'NONE', #128607, 0.06509327318403745899 ) ;
#88863 = CARTESIAN_POINT ( 'NONE',  ( 14.54999999999989235, 2.500000000000000000, -2.165063509461101710 ) ) ;
#88864 = ORIENTED_EDGE ( 'NONE', *, *, #85323, .F. ) ;
#88865 = ORIENTED_EDGE ( 'NONE', *, *, #102803, .T. ) ;
#88866 = ORIENTED_EDGE ( 'NONE', *, *, #104968, .T. ) ;
#88867 = ORIENTED_EDGE ( 'NONE', *, *, #81745, .T. ) ;
#88868 = CIRCLE ( 'NONE', #57582, 0.1000000000000000472 ) ;
#88869 = DIRECTION ( 'NONE',  ( 0.000000000000000000, 0.000000000000000000, 1.000000000000000000 ) ) ;
#88870 = CARTESIAN_POINT ( 'NONE',  ( -4.150000000000025224, 12.50000000000000000, 2.857883832488649301 ) ) ;
#88871 = FACE_BOUND ( 'NONE', #85872, .T. ) ;
#88872 = CARTESIAN_POINT ( 'NONE',  ( -7.900000000000014566, 12.50000000000000000, -5.022947341949754119 ) ) ;
#88873 = ORIENTED_EDGE ( 'NONE', *, *, #14597, .T. ) ;
#88874 = DIRECTION ( 'NONE',  ( -0.000000000000000000, -1.000000000000000000, -0.000000000000000000 ) ) ;
#88875 = CARTESIAN_POINT ( 'NONE',  ( -11.04999999999999893, 2.500000000000000000, 6.048780366869520364 ) ) ;
#88876 = DIRECTION ( 'NONE',  ( 0.000000000000000000, -0.9999939076577903929, 0.003490651415223739937 ) ) ;
#88877 = CARTESIAN_POINT ( 'NONE',  ( 1.049999999999952971, 12.50000000000000000, 6.148780366869520897 ) ) ;
#88878 = DIRECTION ( 'NONE',  ( 0.000000000000000000, 1.000000000000000000, 0.000000000000000000 ) ) ;
#88880 = ORIENTED_EDGE ( 'NONE', *, *, #119921, .F. ) ;
#88879 = CIRCLE ( 'NONE', #61711, 0.06509327318403745899 ) ;
#88881 = CARTESIAN_POINT ( 'NONE',  ( -8.350000000000012079, 2.500000000000000000, -2.957883832488653830 ) ) ;
#88882 = ADVANCED_FACE ( 'NONE', ( #110674 ), #35201, .T. ) ;
#88883 = PRODUCT_DEFINITION_SHAPE ( 'NONE', 'NONE',  #28456 ) ;
#88884 = VERTEX_POINT ( 'NONE', #123548 ) ;
#88885 = EDGE_CURVE ( 'NONE', #23570, #93873, #78122, .T. ) ;
#88886 = ORIENTED_EDGE ( 'NONE', *, *, #3691, .T. ) ;
#88887 = EDGE_CURVE ( 'NONE', #98236, #21944, #2905, .T. ) ;
#88888 = CARTESIAN_POINT ( 'NONE',  ( -4.600000000000028955, 2.500000000000000000, -4.430127018922202176 ) ) ;
#88889 = DIRECTION ( 'NONE',  ( -0.000000000000000000, -1.000000000000000000, -0.000000000000000000 ) ) ;
#88890 = CONICAL_SURFACE ( 'NONE', #107763, 0.09999999999999982514, 0.003490658503988666988 ) ;
#88892 = ORIENTED_EDGE ( 'NONE', *, *, #59551, .F. ) ;
#88891 = EDGE_CURVE ( 'NONE', #126455, #39511, #57180, .T. ) ;
#88893 = AXIS2_PLACEMENT_3D ( 'NONE', #28522, #58636, #88724 ) ;
#88894 = EDGE_CURVE ( 'NONE', #65565, #79722, #124075, .T. ) ;
#88895 = CIRCLE ( 'NONE', #17870, 0.06509327318403741736 ) ;
#88896 = DIRECTION ( 'NONE',  ( 0.000000000000000000, 0.000000000000000000, 1.000000000000000000 ) ) ;
#88897 = DIRECTION ( 'NONE',  ( 0.000000000000000000, 0.000000000000000000, -1.000000000000000000 ) ) ;
#88898 = ORIENTED_EDGE ( 'NONE', *, *, #13664, .F. ) ;
#88900 = EDGE_CURVE ( 'NONE', #105738, #92137, #23748, .T. ) ;
#88899 = LINE ( 'NONE', #71182, #13834 ) ;
#88901 = ORIENTED_EDGE ( 'NONE', *, *, #71151, .F. ) ;
#88902 = DIRECTION ( 'NONE',  ( -0.000000000000000000, -1.000000000000000000, -0.000000000000000000 ) ) ;
#88903 = EDGE_LOOP ( 'NONE', ( #25558, #72130, #3718, #108996, #122837, #9891, #56455, #124091 ) ) ;
#88904 = CARTESIAN_POINT ( 'NONE',  ( -5.400000000000019895, 12.50000000000000000, -0.7579135962115916003 ) ) ;
#88905 = FACE_BOUND ( 'NONE', #58362, .T. ) ;
#88906 = EDGE_CURVE ( 'NONE', #33814, #97603, #19526, .T. ) ;
#88907 = CIRCLE ( 'NONE', #34552, 0.1000000000000002554 ) ;
#88908 = EDGE_CURVE ( 'NONE', #94097, #58339, #84926, .T. ) ;
#88909 = ORIENTED_EDGE ( 'NONE', *, *, #10967, .T. ) ;
#88911 = CARTESIAN_POINT ( 'NONE',  ( 112.8293778049783924, 7.590139747709709006, -1.337168253467446277 ) ) ;
#88910 = VECTOR ( 'NONE', #62013, 1000.000000000000000 ) ;
#88912 = EDGE_LOOP ( 'NONE', ( #5660, #101496, #20994, #22076 ) ) ;
#88913 = DIRECTION ( 'NONE',  ( 0.000000000000000000, 0.000000000000000000, -1.000000000000000000 ) ) ;
#88914 = CARTESIAN_POINT ( 'NONE',  ( -5.850000000000021849, 2.500000000000000000, -2.857883832488653741 ) ) ;
#88915 = DIRECTION ( 'NONE',  ( 0.000000000000000000, 0.000000000000000000, 1.000000000000000000 ) ) ;
#88916 = CARTESIAN_POINT ( 'NONE',  ( -4.600000000000024514, 12.50000000000000000, 0.7579135962115869374 ) ) ;
#88917 = DIRECTION ( 'NONE',  ( -0.000000000000000000, -1.000000000000000000, -0.000000000000000000 ) ) ;
#88918 = ORIENTED_EDGE ( 'NONE', *, *, #120326, .T. ) ;
#88919 = EDGE_LOOP ( 'NONE', ( #122826, #69037 ) ) ;
#88920 = ORIENTED_EDGE ( 'NONE', *, *, #2888, .T. ) ;
#88921 = DIRECTION ( 'NONE',  ( 0.000000000000000000, 0.000000000000000000, 1.000000000000000000 ) ) ;
#88922 = CIRCLE ( 'NONE', #101439, 0.06509327318403745899 ) ;
#88923 = CIRCLE ( 'NONE', #65923, 0.09999999999999982514 ) ;
#88924 = DIRECTION ( 'NONE',  ( 0.000000000000000000, -0.000000000000000000, 1.000000000000000000 ) ) ;
#88925 = DIRECTION ( 'NONE',  ( 1.000000000000000000, -0.000000000000000000, -0.000000000000000000 ) ) ;
#88927 = ORIENTED_EDGE ( 'NONE', *, *, #35470, .T. ) ;
#88926 = VERTEX_POINT ( 'NONE', #94105 ) ;
#88928 = ORIENTED_EDGE ( 'NONE', *, *, #75105, .T. ) ;
#88929 = CARTESIAN_POINT ( 'NONE',  ( 5.849999999999933920, 12.50000000000000000, -2.165063509461101710 ) ) ;
#88930 = DIRECTION ( 'NONE',  ( -0.000000000000000000, -1.000000000000000000, -0.000000000000000000 ) ) ;
#88931 = APPLICATION_PROTOCOL_DEFINITION ( 'draft international standard', 'automotive_design', 1998, #16189 ) ;
#88932 = DIRECTION ( 'NONE',  ( -0.000000000000000000, 1.000000000000000000, -0.000000000000000000 ) ) ;
#88933 = CARTESIAN_POINT ( 'NONE',  ( 7.499999999999923617, 12.50000000000000000, 0.6277270498435120194 ) ) ;
#88934 = CONICAL_SURFACE ( 'NONE', #42986, 0.1000000000000002554, 0.003490658503988666988 ) ;
#88935 = DIRECTION ( 'NONE',  ( 0.000000000000000000, 0.000000000000000000, 1.000000000000000000 ) ) ;
#88936 = DIRECTION ( 'NONE',  ( -0.000000000000000000, -1.000000000000000000, -0.000000000000000000 ) ) ;
#88937 = CARTESIAN_POINT ( 'NONE',  ( 1.649999999999950617, 12.50000000000000000, 2.165063509461097713 ) ) ;
#88938 = AXIS2_PLACEMENT_3D ( 'NONE', #28082, #26789, #47729 ) ;
#88939 = FACE_OUTER_BOUND ( 'NONE', #13972, .T. ) ;
#88940 = VERTEX_POINT ( 'NONE', #24724 ) ;
#88941 = ORIENTED_EDGE ( 'NONE', *, *, #12912, .F. ) ;
#88942 = CARTESIAN_POINT ( 'NONE',  ( 2.899999999999946620, 2.500000000000000000, -5.022947341949754119 ) ) ;
#88943 = VECTOR ( 'NONE', #24082, 1000.000000000000000 ) ;
#88944 = AXIS2_PLACEMENT_3D ( 'NONE', #54503, #25690, #55166 ) ;
#88945 = CARTESIAN_POINT ( 'NONE',  ( -8.150000000000014566, 2.500000000000000000, -6.048780366869521252 ) ) ;
#88946 = ORIENTED_EDGE ( 'NONE', *, *, #50464, .T. ) ;
#88947 = EDGE_LOOP ( 'NONE', ( #65075, #45676 ) ) ;
#88948 = DIRECTION ( 'NONE',  ( 0.000000000000000000, 0.000000000000000000, 1.000000000000000000 ) ) ;
#88949 = CARTESIAN_POINT ( 'NONE',  ( -12.49999999999999289, 12.50000000000000000, 4.957854068765711553 ) ) ;
#88950 = CARTESIAN_POINT ( 'NONE',  ( 2.500000000000001776, 2.021986658763282652, -9.892226903609811828 ) ) ;
#88951 = AXIS2_PLACEMENT_3D ( 'NONE', #83319, #73472, #102939 ) ;
#88952 = CARTESIAN_POINT ( 'NONE',  ( -14.34999999999998543, 2.500000000000000000, -2.511473670974875727 ) ) ;
#88953 = EDGE_CURVE ( 'NONE', #88981, #53090, #27939, .T. ) ;
#88954 = VECTOR ( 'NONE', #8588, 1000.000000000000000 ) ;
#88955 = DIRECTION ( 'NONE',  ( 0.000000000000000000, 0.000000000000000000, 1.000000000000000000 ) ) ;
#88956 = FACE_OUTER_BOUND ( 'NONE', #14752, .T. ) ;
#88957 = CARTESIAN_POINT ( 'NONE',  ( 10.84999999999990905, 2.500000000000000000, -7.188010851410854052 ) ) ;
#88958 = VECTOR ( 'NONE', #55965, 1000.000000000000000 ) ;
#88959 = DIRECTION ( 'NONE',  ( -0.000000000000000000, -1.000000000000000000, -0.000000000000000000 ) ) ;
#88960 = CIRCLE ( 'NONE', #26174, 0.06509327318403745899 ) ;
#88961 = AXIS2_PLACEMENT_3D ( 'NONE', #100956, #11287, #38182 ) ;
#88962 = EDGE_LOOP ( 'NONE', ( #117132, #95289 ) ) ;
#88963 = VECTOR ( 'NONE', #37573, 1000.000000000000000 ) ;
#88964 = ORIENTED_EDGE ( 'NONE', *, *, #107949, .F. ) ;
#88965 = CONICAL_SURFACE ( 'NONE', #32551, 0.1000000000000002554, 0.003490658503988666988 ) ;
#88966 = VERTEX_POINT ( 'NONE', #5707 ) ;
#88967 = VERTEX_POINT ( 'NONE', #54190 ) ;
#88968 = LINE ( 'NONE', #69976, #62928 ) ;
#88969 = CARTESIAN_POINT ( 'NONE',  ( -1.850000000000033840, 2.500000000000000000, 1.918653347947321564 ) ) ;
#88970 = ORIENTED_EDGE ( 'NONE', *, *, #68637, .F. ) ;
#88971 = DIRECTION ( 'NONE',  ( -1.000000000000000000, 0.000000000000000000, 0.000000000000000000 ) ) ;
#88972 = CARTESIAN_POINT ( 'NONE',  ( 17.50000000000000000, -0.9166666666666678509, -9.999999999999998224 ) ) ;
#88973 = CARTESIAN_POINT ( 'NONE',  ( -8.750000000000008882, 2.500000000000000000, 1.472243186433545459 ) ) ;
#88975 = ORIENTED_EDGE ( 'NONE', *, *, #36256, .T. ) ;
#88974 = DIRECTION ( 'NONE',  ( 0.000000000000000000, 0.000000000000000000, 1.000000000000000000 ) ) ;
#88976 = CARTESIAN_POINT ( 'NONE',  ( -10.00000000000000533, 12.50000000000000000, 5.022947341949748790 ) ) ;
#88977 = CIRCLE ( 'NONE', #30415, 0.06509327318403745899 ) ;
#88978 = CARTESIAN_POINT ( 'NONE',  ( 7.699999999999923794, 2.500000000000000000, 4.576537180435972019 ) ) ;
#88979 = VERTEX_POINT ( 'NONE', #3159 ) ;
#88980 = ORIENTED_EDGE ( 'NONE', *, *, #113153, .T. ) ;
#88981 = VERTEX_POINT ( 'NONE', #63359 ) ;
#88982 = EDGE_LOOP ( 'NONE', ( #72786, #50925 ) ) ;
#88983 = DIRECTION ( 'NONE',  ( 0.000000000000000000, 0.000000000000000000, 1.000000000000000000 ) ) ;
#88984 = AXIS2_PLACEMENT_3D ( 'NONE', #79247, #119154, #57670 ) ;
#88985 = AXIS2_PLACEMENT_3D ( 'NONE', #88564, #99040, #48655 ) ;
#88986 = CARTESIAN_POINT ( 'NONE',  ( -14.34999999999998543, 12.50000000000000000, -2.576566944158912964 ) ) ;
#88987 = DIRECTION ( 'NONE',  ( 0.000000000000000000, 0.000000000000000000, 1.000000000000000000 ) ) ;
#88988 = VECTOR ( 'NONE', #72302, 1000.000000000000000 ) ;
#88989 = EDGE_CURVE ( 'NONE', #46456, #107304, #99046, .T. ) ;
#88990 = CIRCLE ( 'NONE', #43317, 0.06509327318403745899 ) ;
#88991 = VERTEX_POINT ( 'NONE', #25345 ) ;
#88992 = CARTESIAN_POINT ( 'NONE',  ( 5.399999999999936406, 2.500000000000000000, -3.637306695894650055 ) ) ;
#88993 = DIRECTION ( 'NONE',  ( -0.000000000000000000, 1.000000000000000000, -0.000000000000000000 ) ) ;
#88994 = ADVANCED_FACE ( 'NONE', ( #73179 ), #34565, .T. ) ;
#88995 = DIRECTION ( 'NONE',  ( 0.000000000000000000, 0.000000000000000000, 1.000000000000000000 ) ) ;
#88996 = CARTESIAN_POINT ( 'NONE',  ( -0.4000000000000404898, 12.50000000000000000, 5.022947341949748790 ) ) ;
#88997 = EDGE_CURVE ( 'NONE', #9756, #30789, #53546, .T. ) ;
#88998 = CONICAL_SURFACE ( 'NONE', #78551, 0.1000000000000000056, 0.003490658503988666988 ) ;
#88999 = EDGE_LOOP ( 'NONE', ( #74076, #31600 ) ) ;
#89000 = DIRECTION ( 'NONE',  ( -4.274815082592931898E-19, -0.9999939076577903929, -0.003490651415223739937 ) ) ;
#89002 = AXIS2_PLACEMENT_3D ( 'NONE', #4335, #55405, #93397 ) ;
#89001 = AXIS2_PLACEMENT_3D ( 'NONE', #14358, #123050, #84401 ) ;
#89003 = EDGE_LOOP ( 'NONE', ( #128688, #29663, #34572, #23878 ) ) ;
#89004 = EDGE_CURVE ( 'NONE', #6453, #86025, #115013, .T. ) ;
#89006 = ORIENTED_EDGE ( 'NONE', *, *, #14565, .F. ) ;
#89005 = EDGE_CURVE ( 'NONE', #5867, #121928, #94837, .T. ) ;
#89007 = DIRECTION ( 'NONE',  ( 0.000000000000000000, 1.000000000000000000, 0.000000000000000000 ) ) ;
#89008 = ADVANCED_FACE ( 'NONE', ( #84277 ), #34220, .T. ) ;
#89009 = FACE_OUTER_BOUND ( 'NONE', #116630, .T. ) ;
#89010 = ADVANCED_FACE ( 'NONE', ( #54809 ), #23409, .T. ) ;
#89011 = FACE_BOUND ( 'NONE', #97153, .T. ) ;
#89012 = CARTESIAN_POINT ( 'NONE',  ( -11.24999999999996447, 2.500000000000000000, -6.495190528383298911 ) ) ;
#89013 = DIRECTION ( 'NONE',  ( 0.000000000000000000, 0.000000000000000000, -1.000000000000000000 ) ) ;
#89014 = DIRECTION ( 'NONE',  ( -4.274815082592931898E-19, -0.9999939076577903929, -0.003490651415223739937 ) ) ;
#89015 = VECTOR ( 'NONE', #36879, 1000.000000000000000 ) ;
#89016 = AXIS2_PLACEMENT_3D ( 'NONE', #33532, #25613, #115938 ) ;
#89017 = ORIENTED_EDGE ( 'NONE', *, *, #18254, .T. ) ;
#89018 = DIRECTION ( 'NONE',  ( -0.000000000000000000, 1.000000000000000000, -0.000000000000000000 ) ) ;
#89019 = DIRECTION ( 'NONE',  ( 0.000000000000000000, -0.9999939076577903929, 0.003490651415223739937 ) ) ;
#89020 = EDGE_CURVE ( 'NONE', #90572, #776, #6983, .T. ) ;
#89021 = LINE ( 'NONE', #98824, #17406 ) ;
#89022 = CARTESIAN_POINT ( 'NONE',  ( -0.8500000000000382805, 12.50000000000000000, -1.472243186433550122 ) ) ;
#89023 = ORIENTED_EDGE ( 'NONE', *, *, #118434, .F. ) ;
#89024 = PLANE ( 'NONE',  #120131 ) ;
#89025 = FACE_OUTER_BOUND ( 'NONE', #70032, .T. ) ;
#89026 = ORIENTED_EDGE ( 'NONE', *, *, #6829, .T. ) ;
#89027 = EDGE_LOOP ( 'NONE', ( #64168, #45944 ) ) ;
#89028 = FACE_OUTER_BOUND ( 'NONE', #48045, .T. ) ;
#89029 = LINE ( 'NONE', #121058, #38110 ) ;
#89030 = FACE_BOUND ( 'NONE', #82834, .T. ) ;
#89031 = CARTESIAN_POINT ( 'NONE',  ( 15.40649769635636801, -2.500000000000000000, -5.817321165395405558 ) ) ;
#89032 = AXIS2_PLACEMENT_3D ( 'NONE', #97101, #108199, #26437 ) ;
#89033 = DIRECTION ( 'NONE',  ( 0.000000000000000000, 0.000000000000000000, 1.000000000000000000 ) ) ;
#89034 = CIRCLE ( 'NONE', #74457, 0.1000000000000002554 ) ;
#89035 = ORIENTED_EDGE ( 'NONE', *, *, #81354, .F. ) ;
#89037 = ADVANCED_FACE ( 'NONE', ( #58693 ), #7643, .T. ) ;
#89036 = LINE ( 'NONE', #128333, #128207 ) ;
#89038 = CARTESIAN_POINT ( 'NONE',  ( 184.8750000000000000, 8.891194145520236347, 5.444286225454521982E-16 ) ) ;
#89039 = ORIENTED_EDGE ( 'NONE', *, *, #121583, .F. ) ;
#89040 = DIRECTION ( 'NONE',  ( 0.000000000000000000, 0.000000000000000000, 1.000000000000000000 ) ) ;
#89041 = DIRECTION ( 'NONE',  ( 0.000000000000000000, 0.000000000000000000, 1.000000000000000000 ) ) ;
#89042 = AXIS2_PLACEMENT_3D ( 'NONE', #98459, #11383, #68369 ) ;
#89043 = ADVANCED_FACE ( 'NONE', ( #75741 ), #115664, .T. ) ;
#89044 = FACE_OUTER_BOUND ( 'NONE', #37493, .T. ) ;
#89045 = FACE_OUTER_BOUND ( 'NONE', #680, .T. ) ;
#89046 = ADVANCED_FACE ( 'NONE', ( #126794 ), #67635, .T. ) ;
#89047 = ORIENTED_EDGE ( 'NONE', *, *, #35213, .T. ) ;
#89048 = EDGE_CURVE ( 'NONE', #27272, #21509, #107792, .T. ) ;
#89049 = VECTOR ( 'NONE', #39997, 1000.000000000000000 ) ;
#89050 = DIRECTION ( 'NONE',  ( -0.000000000000000000, -1.000000000000000000, -0.000000000000000000 ) ) ;
#89051 = PLANE ( 'NONE',  #33098 ) ;
#89052 = DIRECTION ( 'NONE',  ( 0.000000000000000000, 1.000000000000000000, 0.000000000000000000 ) ) ;
#89053 = AXIS2_PLACEMENT_3D ( 'NONE', #1230, #102014, #29415 ) ;
#89054 = CARTESIAN_POINT ( 'NONE',  ( 16.56034314470449686, -0.8287381876616503051, -6.090234461610894101 ) ) ;
#89055 = ORIENTED_EDGE ( 'NONE', *, *, #52677, .F. ) ;
#89056 = EDGE_LOOP ( 'NONE', ( #57100, #104713 ) ) ;
#89057 = EDGE_CURVE ( 'NONE', #80664, #71349, #65589, .T. ) ;
#89058 = CARTESIAN_POINT ( 'NONE',  ( 16.98713617295328149, 1.503435538382916326, 5.629434171173037349 ) ) ;
#89060 = ORIENTED_EDGE ( 'NONE', *, *, #45118, .T. ) ;
#89059 = EDGE_CURVE ( 'NONE', #95554, #34514, #46955, .T. ) ;
#89061 = CARTESIAN_POINT ( 'NONE',  ( 8.099999999999921485, 12.50000000000000000, -0.3464101615137783474 ) ) ;
#89062 = FACE_OUTER_BOUND ( 'NONE', #121492, .T. ) ;
#89063 = EDGE_CURVE ( 'NONE', #80857, #95501, #63449, .T. ) ;
#89064 = DIRECTION ( 'NONE',  ( 0.000000000000000000, -0.000000000000000000, 1.000000000000000000 ) ) ;
#89065 = ADVANCED_FACE ( 'NONE', ( #77045 ), #118253, .T. ) ;
#89066 = CARTESIAN_POINT ( 'NONE',  ( -13.94999999999998863, 12.50000000000000000, -1.818653347947323917 ) ) ;
#89067 = ORIENTED_EDGE ( 'NONE', *, *, #80606, .F. ) ;
#89068 = CARTESIAN_POINT ( 'NONE',  ( -13.74999999999998934, 12.50000000000000000, -1.537336459617585360 ) ) ;
#89069 = DIRECTION ( 'NONE',  ( -4.274815082592931898E-19, -0.9999939076577903929, -0.003490651415223739937 ) ) ;
#89070 = CARTESIAN_POINT ( 'NONE',  ( -3.150000000000032330, 2.500000000000000000, -6.048780366869526581 ) ) ;
#89071 = CARTESIAN_POINT ( 'NONE',  ( 185.6093750003413732, 9.264065473108010111E-16, -7.564683531250000925 ) ) ;
#89072 = FACE_OUTER_BOUND ( 'NONE', #19947, .T. ) ;
#89073 = AXIS2_PLACEMENT_3D ( 'NONE', #1941, #121085, #113185 ) ;
#89075 = EDGE_CURVE ( 'NONE', #53805, #31468, #9157, .T. ) ;
#89074 = DIRECTION ( 'NONE',  ( 0.000000000000000000, 1.000000000000000000, 0.000000000000000000 ) ) ;
#89076 = EDGE_LOOP ( 'NONE', ( #79089, #120369 ) ) ;
#89077 = ORIENTED_EDGE ( 'NONE', *, *, #6742, .T. ) ;
#89078 = CARTESIAN_POINT ( 'NONE',  ( 3.349999999999945466, 12.50000000000000000, -6.495190528383302464 ) ) ;
#89079 = ORIENTED_EDGE ( 'NONE', *, *, #64153, .T. ) ;
#89080 = FACE_OUTER_BOUND ( 'NONE', #82165, .T. ) ;
#89082 = ORIENTED_EDGE ( 'NONE', *, *, #223, .F. ) ;
#89081 = ORIENTED_EDGE ( 'NONE', *, *, #107477, .F. ) ;
#89083 = ORIENTED_EDGE ( 'NONE', *, *, #29198, .F. ) ;
#89084 = PLANE ( 'NONE',  #37458 ) ;
#89085 = AXIS2_PLACEMENT_3D ( 'NONE', #15269, #125251, #95150 ) ;
#89086 = CIRCLE ( 'NONE', #32674, 1.388921157871087386 ) ;
#89087 = DIRECTION ( 'NONE',  ( -0.000000000000000000, -1.000000000000000000, -0.000000000000000000 ) ) ;
#89088 = DIRECTION ( 'NONE',  ( 0.000000000000000000, 1.000000000000000000, 0.000000000000000000 ) ) ;
#89089 = CIRCLE ( 'NONE', #39033, 0.06509327318403745899 ) ;
#89090 = FACE_OUTER_BOUND ( 'NONE', #40268, .T. ) ;
#89091 = DIRECTION ( 'NONE',  ( 0.000000000000000000, 0.000000000000000000, 1.000000000000000000 ) ) ;
#89092 = FACE_OUTER_BOUND ( 'NONE', #4850, .T. ) ;
#89093 = CARTESIAN_POINT ( 'NONE',  ( 13.74999999999989697, 2.500000000000000000, 2.757883832488649656 ) ) ;
#89094 = DIRECTION ( 'NONE',  ( 0.000000000000000000, 0.000000000000000000, -1.000000000000000000 ) ) ;
#89095 = ORIENTED_EDGE ( 'NONE', *, *, #83856, .F. ) ;
#89096 = AXIS2_PLACEMENT_3D ( 'NONE', #86253, #36550, #26712 ) ;
#89097 = ORIENTED_EDGE ( 'NONE', *, *, #31540, .F. ) ;
#89099 = AXIS2_PLACEMENT_3D ( 'NONE', #118186, #16735, #96592 ) ;
#89098 = CIRCLE ( 'NONE', #116266, 0.1000000000000002554 ) ;
#89100 = DIRECTION ( 'NONE',  ( 0.000000000000000000, 0.000000000000000000, 1.000000000000000000 ) ) ;
#89101 = VERTEX_POINT ( 'NONE', #18112 ) ;
#89102 = VERTEX_POINT ( 'NONE', #128081 ) ;
#89103 = CARTESIAN_POINT ( 'NONE',  ( 6.649999999999928413, 12.50000000000000000, 1.537336459617582918 ) ) ;
#89104 = CARTESIAN_POINT ( 'NONE',  ( -5.850000000000021849, 12.50000000000000000, -5.867463478539787225 ) ) ;
#89105 = EDGE_CURVE ( 'NONE', #53017, #117711, #116948, .T. ) ;
#89106 = CARTESIAN_POINT ( 'NONE',  ( -13.74999999999995381, 2.500000000000000000, 2.265063509461101354 ) ) ;
#89107 = DIRECTION ( 'NONE',  ( 0.000000000000000000, 0.000000000000000000, 1.000000000000000000 ) ) ;
#89108 = CARTESIAN_POINT ( 'NONE',  ( 12.49999999999990408, 12.50000000000000000, 5.022947341949748790 ) ) ;
#89109 = ORIENTED_EDGE ( 'NONE', *, *, #43106, .F. ) ;
#89110 = EDGE_LOOP ( 'NONE', ( #127997, #114155, #40773, #98328 ) ) ;
#89111 = DIRECTION ( 'NONE',  ( 0.000000000000000000, 0.000000000000000000, 1.000000000000000000 ) ) ;
#89112 = EDGE_LOOP ( 'NONE', ( #56363, #58742, #112417, #85982 ) ) ;
#89113 = DIRECTION ( 'NONE',  ( 0.000000000000000000, 0.000000000000000000, 1.000000000000000000 ) ) ;
#89114 = ORIENTED_EDGE ( 'NONE', *, *, #125996, .F. ) ;
#89115 = EDGE_CURVE ( 'NONE', #110068, #47774, #42633, .T. ) ;
#89116 = EDGE_LOOP ( 'NONE', ( #9448, #126363, #7178, #44458 ) ) ;
#89117 = DIRECTION ( 'NONE',  ( -0.000000000000000000, -1.000000000000000000, -0.000000000000000000 ) ) ;
#89118 = DIRECTION ( 'NONE',  ( 0.000000000000000000, 0.000000000000000000, 1.000000000000000000 ) ) ;
#89119 = AXIS2_PLACEMENT_3D ( 'NONE', #5977, #13221, #114651 ) ;
#89120 = CARTESIAN_POINT ( 'NONE',  ( -13.74999999999995381, 2.500000000000000000, 2.165063509461101265 ) ) ;
#89122 = CARTESIAN_POINT ( 'NONE',  ( -7.300000000000013145, 12.50000000000000000, 4.048810130592458201 ) ) ;
#89121 = CONICAL_SURFACE ( 'NONE', #34861, 0.1000000000000002554, 0.003490658503988666988 ) ;
#89123 = LINE ( 'NONE', #67523, #86808 ) ;
#89124 = ORIENTED_EDGE ( 'NONE', *, *, #79295, .F. ) ;
#89125 = LINE ( 'NONE', #17121, #125107 ) ;
#89126 = DIRECTION ( 'NONE',  ( -4.274815082592931898E-19, -0.9999939076577903929, -0.003490651415223739937 ) ) ;
#89127 = FACE_OUTER_BOUND ( 'NONE', #1799, .T. ) ;
#89128 = DIRECTION ( 'NONE',  ( 0.000000000000000000, 0.000000000000000000, 1.000000000000000000 ) ) ;
#89130 = CONICAL_SURFACE ( 'NONE', #9712, 0.1000000000000002554, 0.003490658503988666988 ) ;
#89129 = CIRCLE ( 'NONE', #32720, 0.1000000000000002554 ) ;
#89131 = DIRECTION ( 'NONE',  ( 0.000000000000000000, 1.000000000000000000, 0.000000000000000000 ) ) ;
#89132 = VERTEX_POINT ( 'NONE', #96038 ) ;
#89133 = ORIENTED_EDGE ( 'NONE', *, *, #98916, .F. ) ;
#89134 = CARTESIAN_POINT ( 'NONE',  ( -3.150000000000029665, 12.50000000000000000, 6.776507416713035248 ) ) ;
#89135 = ORIENTED_EDGE ( 'NONE', *, *, #63929, .F. ) ;
#89136 = AXIS2_PLACEMENT_3D ( 'NONE', #43430, #34894, #123880 ) ;
#89137 = DIRECTION ( 'NONE',  ( -0.000000000000000000, -1.000000000000000000, -0.000000000000000000 ) ) ;
#89138 = CARTESIAN_POINT ( 'NONE',  ( 0.4499999999999573785, 2.500000000000000000, -6.595190528383302109 ) ) ;
#89139 = ADVANCED_FACE ( 'NONE', ( #88115 ), #46820, .T. ) ;
#89140 = ORIENTED_EDGE ( 'NONE', *, *, #114309, .T. ) ;
#89141 = DIRECTION ( 'NONE',  ( 0.000000000000000000, 1.000000000000000000, 0.000000000000000000 ) ) ;
#89142 = CARTESIAN_POINT ( 'NONE',  ( -0.4000000000000339950, 2.500000000000000000, 0.6928203230275518099 ) ) ;
#89143 = DIRECTION ( 'NONE',  ( 0.000000000000000000, 1.000000000000000000, 0.000000000000000000 ) ) ;
#89144 = LINE ( 'NONE', #37488, #124995 ) ;
#89145 = VERTEX_POINT ( 'NONE', #56100 ) ;
#89146 = EDGE_CURVE ( 'NONE', #117684, #102868, #9254, .T. ) ;
#89147 = DIRECTION ( 'NONE',  ( -4.274815082592931898E-19, -0.9999939076577903929, -0.003490651415223739937 ) ) ;
#89148 = ORIENTED_EDGE ( 'NONE', *, *, #18236, .T. ) ;
#89149 = ADVANCED_FACE ( 'NONE', ( #36497 ), #113717, .T. ) ;
#89150 = EDGE_CURVE ( 'NONE', #114153, #104101, #99142, .T. ) ;
#89151 = EDGE_CURVE ( 'NONE', #105503, #111361, #21787, .T. ) ;
#89153 = EDGE_CURVE ( 'NONE', #84568, #29080, #20069, .T. ) ;
#89152 = CARTESIAN_POINT ( 'NONE',  ( 32.27132508960535517, 3.178320084206410545, -3.140934779234540564 ) ) ;
#89154 = AXIS2_PLACEMENT_3D ( 'NONE', #497, #8387, #107882 ) ;
#89155 = EDGE_CURVE ( 'NONE', #22461, #70010, #28035, .T. ) ;
#89156 = LINE ( 'NONE', #1410, #31002 ) ;
#89157 = CARTESIAN_POINT ( 'NONE',  ( -4.350000000000027178, 2.500000000000000000, -6.841600689897077814 ) ) ;
#89158 = ORIENTED_EDGE ( 'NONE', *, *, #14729, .F. ) ;
#89159 = AXIS2_PLACEMENT_3D ( 'NONE', #44233, #44901, #105747 ) ;
#89160 = DIRECTION ( 'NONE',  ( 0.000000000000000000, 0.000000000000000000, -1.000000000000000000 ) ) ;
#89161 = AXIS2_PLACEMENT_3D ( 'NONE', #19507, #30640, #120299 ) ;
#89162 = EDGE_LOOP ( 'NONE', ( #112892, #68605, #99756, #127229 ) ) ;
#89163 = CARTESIAN_POINT ( 'NONE',  ( -11.25000000000000178, 2.500000000000000000, -5.702370205355745902 ) ) ;
#89164 = DIRECTION ( 'NONE',  ( 0.000000000000000000, 0.000000000000000000, -1.000000000000000000 ) ) ;
#89165 = ADVANCED_FACE ( 'NONE', ( #61929 ), #109509, .T. ) ;
#89166 = DIRECTION ( 'NONE',  ( 0.000000000000000000, 0.000000000000000000, 1.000000000000000000 ) ) ;
#89167 = AXIS2_PLACEMENT_3D ( 'NONE', #808, #100932, #40767 ) ;
#89168 = VERTEX_POINT ( 'NONE', #99274 ) ;
#89169 = ADVANCED_FACE ( 'NONE', ( #31816 ), #109052, .T. ) ;
#89171 = EDGE_CURVE ( 'NONE', #41154, #64623, #115852, .T. ) ;
#89170 = DIRECTION ( 'NONE',  ( -0.000000000000000000, 1.000000000000000000, -0.000000000000000000 ) ) ;
#89172 = VECTOR ( 'NONE', #105294, 1000.000000000000000 ) ;
#89173 = CARTESIAN_POINT ( 'NONE',  ( 9.349999999999916156, 2.500000000000000000, -2.611473670974877592 ) ) ;
#89174 = EDGE_LOOP ( 'NONE', ( #100342, #81296 ) ) ;
#89175 = CARTESIAN_POINT ( 'NONE',  ( 2.899999999999946620, 12.50000000000000000, -3.702399969078687292 ) ) ;
#89176 = EDGE_LOOP ( 'NONE', ( #63666, #9497, #55048, #93378 ) ) ;
#89178 = VECTOR ( 'NONE', #124596, 1000.000000000000000 ) ;
#89177 = DIRECTION ( 'NONE',  ( -4.274815082592931898E-19, -0.9999939076577903929, -0.003490651415223739937 ) ) ;
#89180 = CONICAL_SURFACE ( 'NONE', #112174, 0.09999999999999982514, 0.003490658503988666988 ) ;
#89179 = VECTOR ( 'NONE', #71868, 1000.000000000000000 ) ;
#89181 = ORIENTED_EDGE ( 'NONE', *, *, #5843, .F. ) ;
#89182 = CARTESIAN_POINT ( 'NONE',  ( -1.250000000000037970, 12.50000000000000000, 7.122917578226811486 ) ) ;
#89183 = CARTESIAN_POINT ( 'NONE',  ( -1.850000000000033840, 2.500000000000000000, 6.248780366869521430 ) ) ;
#89184 = ORIENTED_EDGE ( 'NONE', *, *, #101850, .T. ) ;
#89185 = ORIENTED_EDGE ( 'NONE', *, *, #107782, .T. ) ;
#89186 = CARTESIAN_POINT ( 'NONE',  ( -10.85000000000000142, 2.500000000000000000, -1.572243186433546214 ) ) ;
#89187 = FACE_OUTER_BOUND ( 'NONE', #83545, .T. ) ;
#89188 = ORIENTED_EDGE ( 'NONE', *, *, #88725, .F. ) ;
#89189 = CARTESIAN_POINT ( 'NONE',  ( 8.299999999999922551, 12.50000000000000000, -4.330127018922201643 ) ) ;
#89190 = DIRECTION ( 'NONE',  ( 0.000000000000000000, 1.000000000000000000, 0.000000000000000000 ) ) ;
#89191 = DIRECTION ( 'NONE',  ( -0.000000000000000000, -1.000000000000000000, -0.000000000000000000 ) ) ;
#89192 = CARTESIAN_POINT ( 'NONE',  ( 105.4784750942634588, 7.548935851765135929, -4.329562946656615452 ) ) ;
#89193 = CARTESIAN_POINT ( 'NONE',  ( -11.25000000000000178, 2.500000000000000000, -5.802370205355746435 ) ) ;
#89194 = CARTESIAN_POINT ( 'NONE',  ( -9.600000000000008527, 2.500000000000000000, -2.385244779468109755E-15 ) ) ;
#89195 = LINE ( 'NONE', #150, #71358 ) ;
#89196 = ORIENTED_EDGE ( 'NONE', *, *, #125777, .F. ) ;
#89197 = ORIENTED_EDGE ( 'NONE', *, *, #20289, .F. ) ;
#89198 = EDGE_LOOP ( 'NONE', ( #104024, #104512 ) ) ;
#89199 = ORIENTED_EDGE ( 'NONE', *, *, #62771, .F. ) ;
#89200 = CARTESIAN_POINT ( 'NONE',  ( -10.20000000000000639, 2.500000000000000000, -3.983716857408421852 ) ) ;
#89201 = DIRECTION ( 'NONE',  ( 1.000000000000000000, 0.000000000000000000, 0.000000000000000000 ) ) ;
#89202 = CARTESIAN_POINT ( 'NONE',  ( -1.450000000000035927, 2.500000000000000000, -1.718653347947326049 ) ) ;
#89203 = ORIENTED_EDGE ( 'NONE', *, *, #98488, .F. ) ;
#89204 = FACE_BOUND ( 'NONE', #28146, .T. ) ;
#89205 = VERTEX_POINT ( 'NONE', #50812 ) ;
#89206 = EDGE_CURVE ( 'NONE', #48509, #90525, #78217, .T. ) ;
#89207 = CARTESIAN_POINT ( 'NONE',  ( 12.49999999999990585, 2.500000000000000000, 3.737306695894644371 ) ) ;
#89208 = DIRECTION ( 'NONE',  ( -4.274815082592931898E-19, -0.9999939076577903929, -0.003490651415223739937 ) ) ;
#89209 = EDGE_CURVE ( 'NONE', #32144, #40462, #3000, .T. ) ;
#89210 = LINE ( 'NONE', #78111, #68022 ) ;
#89211 = AXIS2_PLACEMENT_3D ( 'NONE', #33388, #32746, #73283 ) ;
#89212 = DIRECTION ( 'NONE',  ( -0.000000000000000000, 1.000000000000000000, -0.000000000000000000 ) ) ;
#89213 = AXIS2_PLACEMENT_3D ( 'NONE', #85098, #23605, #104725 ) ;
#89214 = ADVANCED_FACE ( 'NONE', ( #88796 ), #129397, .T. ) ;
#89215 = LINE ( 'NONE', #129170, #38181 ) ;
#89216 = CARTESIAN_POINT ( 'NONE',  ( -7.700000000000014388, 2.500000000000000000, -4.676537180435977881 ) ) ;
#89217 = CARTESIAN_POINT ( 'NONE',  ( 10.84999999999991260, 12.50000000000000000, 6.430097255199259010 ) ) ;
#89218 = DIRECTION ( 'NONE',  ( 0.000000000000000000, 0.000000000000000000, 1.000000000000000000 ) ) ;
#89219 = CARTESIAN_POINT ( 'NONE',  ( -4.150000000000027889, 2.500000000000000000, -6.595190528383302109 ) ) ;
#89221 = ADVANCED_FACE ( 'NONE', ( #128752 ), #36463, .T. ) ;
#89220 = CARTESIAN_POINT ( 'NONE',  ( -6.050000000000017586, 2.500000000000000000, 1.718653347947321386 ) ) ;
#89222 = CIRCLE ( 'NONE', #34953, 0.06509327318403745899 ) ;
#89223 = ORIENTED_EDGE ( 'NONE', *, *, #18288, .F. ) ;
#89224 = ORIENTED_EDGE ( 'NONE', *, *, #122745, .F. ) ;
#89225 = ORIENTED_EDGE ( 'NONE', *, *, #76371, .T. ) ;
#89226 = EDGE_LOOP ( 'NONE', ( #17395, #63621, #59623, #23290 ) ) ;
#89227 = CARTESIAN_POINT ( 'NONE',  ( 17.28959186693577266, -1.567451025696849021, -5.035561754033041737 ) ) ;
#89228 = DIRECTION ( 'NONE',  ( 0.000000000000000000, 1.000000000000000000, 0.000000000000000000 ) ) ;
#89230 = ORIENTED_EDGE ( 'NONE', *, *, #61890, .F. ) ;
#89229 = ORIENTED_EDGE ( 'NONE', *, *, #77801, .F. ) ;
#89231 = VECTOR ( 'NONE', #95662, 1000.000000000000000 ) ;
#89232 = ORIENTED_EDGE ( 'NONE', *, *, #70586, .T. ) ;
#89233 = DIRECTION ( 'NONE',  ( -0.000000000000000000, -1.000000000000000000, -0.000000000000000000 ) ) ;
#89234 = AXIS2_PLACEMENT_3D ( 'NONE', #87072, #18975, #56956 ) ;
#89235 = DIRECTION ( 'NONE',  ( 0.000000000000000000, 0.000000000000000000, 1.000000000000000000 ) ) ;
#89236 = CARTESIAN_POINT ( 'NONE',  ( -5.200000000000022382, 2.500000000000000000, 0.2464101615137735679 ) ) ;
#89237 = DIRECTION ( 'NONE',  ( 0.000000000000000000, -0.9999939076577903929, 0.003490651415223739937 ) ) ;
#89238 = CARTESIAN_POINT ( 'NONE',  ( 10.39999999999991154, 2.500000000000000000, -3.637306695894650055 ) ) ;
#89239 = DIRECTION ( 'NONE',  ( 0.000000000000000000, 1.000000000000000000, 0.000000000000000000 ) ) ;
#89240 = DIRECTION ( 'NONE',  ( -0.000000000000000000, 1.000000000000000000, -0.000000000000000000 ) ) ;
#89241 = EDGE_CURVE ( 'NONE', #118034, #11372, #65673, .T. ) ;
#89242 = VERTEX_POINT ( 'NONE', #69802 ) ;
#89243 = DIRECTION ( 'NONE',  ( -0.000000000000000000, -1.000000000000000000, -0.000000000000000000 ) ) ;
#89244 = ORIENTED_EDGE ( 'NONE', *, *, #62731, .F. ) ;
#89245 = VERTEX_POINT ( 'NONE', #51465 ) ;
#89246 = VERTEX_POINT ( 'NONE', #40357 ) ;
#89247 = CARTESIAN_POINT ( 'NONE',  ( 4.799999999999934097, 12.50000000000000000, 4.676537180435972552 ) ) ;
#89248 = EDGE_LOOP ( 'NONE', ( #125259, #2600 ) ) ;
#89249 = AXIS2_PLACEMENT_3D ( 'NONE', #50127, #78298, #28540 ) ;
#89250 = VERTEX_POINT ( 'NONE', #1691 ) ;
#89251 = AXIS2_PLACEMENT_3D ( 'NONE', #122399, #73279, #34009 ) ;
#89253 = CARTESIAN_POINT ( 'NONE',  ( 10.84999999999990905, 2.500000000000000000, 1.572243186433545548 ) ) ;
#89252 = CIRCLE ( 'NONE', #5603, 0.1000000000000002554 ) ;
#89254 = DIRECTION ( 'NONE',  ( -0.000000000000000000, 1.000000000000000000, -0.000000000000000000 ) ) ;
#89256 = CIRCLE ( 'NONE', #80945, 0.09999999999999999167 ) ;
#89255 = DIRECTION ( 'NONE',  ( 0.000000000000000000, 1.000000000000000000, 0.000000000000000000 ) ) ;
#89257 = EDGE_CURVE ( 'NONE', #78294, #3186, #7078, .T. ) ;
#89258 = CARTESIAN_POINT ( 'NONE',  ( -13.54999999999999005, 12.50000000000000000, 2.511473670974877503 ) ) ;
#89259 = FACE_OUTER_BOUND ( 'NONE', #5560, .T. ) ;
#89260 = CONICAL_SURFACE ( 'NONE', #76647, 0.1000000000000002554, 0.003490658503988666988 ) ;
#89261 = VERTEX_POINT ( 'NONE', #109730 ) ;
#89263 = AXIS2_PLACEMENT_3D ( 'NONE', #15110, #5310, #95002 ) ;
#89262 = DIRECTION ( 'NONE',  ( -4.274815082592931898E-19, -0.9999939076577903929, -0.003490651415223739937 ) ) ;
#89264 = ORIENTED_EDGE ( 'NONE', *, *, #22588, .F. ) ;
#89265 = VECTOR ( 'NONE', #36835, 1000.000000000000000 ) ;
#89266 = DIRECTION ( 'NONE',  ( -4.274815082592931898E-19, -0.9999939076577903929, -0.003490651415223739937 ) ) ;
#89267 = ORIENTED_EDGE ( 'NONE', *, *, #40416, .T. ) ;
#89268 = DIRECTION ( 'NONE',  ( -0.000000000000000000, 1.000000000000000000, -0.000000000000000000 ) ) ;
#89269 = CARTESIAN_POINT ( 'NONE',  ( 8.749999999999921840, 12.50000000000000000, 2.857883832488649301 ) ) ;
#89270 = ORIENTED_EDGE ( 'NONE', *, *, #68797, .F. ) ;
#89271 = DIRECTION ( 'NONE',  ( 0.000000000000000000, 0.000000000000000000, 1.000000000000000000 ) ) ;
#89272 = AXIS2_PLACEMENT_3D ( 'NONE', #124977, #45783, #56851 ) ;
#89273 = EDGE_CURVE ( 'NONE', #118968, #27375, #13348, .T. ) ;
#89274 = DIRECTION ( 'NONE',  ( 0.000000000000000000, 1.000000000000000000, 0.000000000000000000 ) ) ;
#89275 = EDGE_LOOP ( 'NONE', ( #126914, #15381, #88150, #53533 ) ) ;
#89276 = AXIS2_PLACEMENT_3D ( 'NONE', #38824, #116691, #117982 ) ;
#89278 = AXIS2_PLACEMENT_3D ( 'NONE', #56207, #34671, #5170 ) ;
#89277 = CIRCLE ( 'NONE', #80878, 0.09999999999999982514 ) ;
#89279 = DIRECTION ( 'NONE',  ( 0.000000000000000000, 0.000000000000000000, -1.000000000000000000 ) ) ;
#89280 = VERTEX_POINT ( 'NONE', #71737 ) ;
#89282 = VERTEX_POINT ( 'NONE', #122138 ) ;
#89281 = ADVANCED_FACE ( 'NONE', ( #111666 ), #48890, .T. ) ;
#89283 = DIRECTION ( 'NONE',  ( 0.000000000000000000, 0.000000000000000000, 1.000000000000000000 ) ) ;
#89284 = DIRECTION ( 'NONE',  ( 0.000000000000000000, 0.000000000000000000, 1.000000000000000000 ) ) ;
#89285 = CARTESIAN_POINT ( 'NONE',  ( 184.1718750003414016, 9.264065473108010111E-16, -7.564683531250000925 ) ) ;
#89286 = DIRECTION ( 'NONE',  ( 0.000000000000000000, -0.9999939076577903929, 0.003490651415223739937 ) ) ;
#89287 = DIRECTION ( 'NONE',  ( -4.274815082592931898E-19, -0.9999939076577903929, -0.003490651415223739937 ) ) ;
#89288 = VERTEX_POINT ( 'NONE', #34411 ) ;
#89289 = DIRECTION ( 'NONE',  ( -1.000000000000000000, -0.000000000000000000, -0.000000000000000000 ) ) ;
#89290 = CIRCLE ( 'NONE', #32876, 0.1000000000000000472 ) ;
#89291 = ORIENTED_EDGE ( 'NONE', *, *, #90194, .T. ) ;
#89292 = LINE ( 'NONE', #59209, #125898 ) ;
#89293 = CARTESIAN_POINT ( 'NONE',  ( -11.25000000000000000, 2.500000000000000000, -2.857883832488649745 ) ) ;
#89294 = ADVANCED_FACE ( 'NONE', ( #93956 ), #40582, .T. ) ;
#89295 = CARTESIAN_POINT ( 'NONE',  ( 187.0885416670080872, -6.551208109652273848, -3.782341765625003571 ) ) ;
#89296 = DIRECTION ( 'NONE',  ( -0.000000000000000000, 1.000000000000000000, -0.000000000000000000 ) ) ;
#89297 = CARTESIAN_POINT ( 'NONE',  ( -4.150000000000025224, 12.50000000000000000, 6.495190528383297135 ) ) ;
#89298 = DIRECTION ( 'NONE',  ( 0.000000000000000000, 0.000000000000000000, -1.000000000000000000 ) ) ;
#89299 = DIRECTION ( 'NONE',  ( 0.000000000000000000, 0.000000000000000000, 1.000000000000000000 ) ) ;
#89300 = VERTEX_POINT ( 'NONE', #3001 ) ;
#89301 = EDGE_CURVE ( 'NONE', #90185, #101564, #112311, .T. ) ;
#89302 = CIRCLE ( 'NONE', #49614, 0.06509327318403745899 ) ;
#89303 = CARTESIAN_POINT ( 'NONE',  ( 4.199999999999939782, 12.50000000000000000, 0.06509327318403515528 ) ) ;
#89304 = AXIS2_PLACEMENT_3D ( 'NONE', #20883, #60805, #11041 ) ;
#89305 = DIRECTION ( 'NONE',  ( -0.000000000000000000, -1.000000000000000000, -0.000000000000000000 ) ) ;
#89306 = EDGE_CURVE ( 'NONE', #100844, #128715, #70687, .T. ) ;
#89307 = EDGE_CURVE ( 'NONE', #51386, #43124, #14082, .T. ) ;
#89308 = EDGE_CURVE ( 'NONE', #74070, #59844, #119975, .T. ) ;
#89309 = ADVANCED_FACE ( 'NONE', ( #33120 ), #30110, .T. ) ;
#89310 = ORIENTED_EDGE ( 'NONE', *, *, #35060, .T. ) ;
#89312 = AXIS2_PLACEMENT_3D ( 'NONE', #60802, #58240, #28776 ) ;
#89311 = CIRCLE ( 'NONE', #16125, 0.09999999999999999167 ) ;
#89313 = DIRECTION ( 'NONE',  ( 0.000000000000000000, 0.000000000000000000, 1.000000000000000000 ) ) ;
#89314 = ORIENTED_EDGE ( 'NONE', *, *, #82134, .T. ) ;
#89315 = VERTEX_POINT ( 'NONE', #44865 ) ;
#89316 = PLANE ( 'NONE',  #122035 ) ;
#89317 = EDGE_CURVE ( 'NONE', #22678, #97846, #63544, .T. ) ;
#89318 = EDGE_CURVE ( 'NONE', #2346, #46559, #52101, .T. ) ;
#89319 = EDGE_LOOP ( 'NONE', ( #30207, #125882, #55281, #35072 ) ) ;
#89320 = DIRECTION ( 'NONE',  ( 0.000000000000000000, 0.000000000000000000, 1.000000000000000000 ) ) ;
#89321 = DIRECTION ( 'NONE',  ( -0.000000000000000000, -1.000000000000000000, -0.000000000000000000 ) ) ;
#89322 = ADVANCED_FACE ( 'NONE', ( #64485 ), #57276, .T. ) ;
#89324 = AXIS2_PLACEMENT_3D ( 'NONE', #53611, #103998, #14927 ) ;
#89323 = AXIS2_PLACEMENT_3D ( 'NONE', #112320, #110375, #60018 ) ;
#89325 = EDGE_LOOP ( 'NONE', ( #116846, #15999 ) ) ;
#89326 = EDGE_CURVE ( 'NONE', #99388, #40733, #11301, .T. ) ;
#89327 = AXIS2_PLACEMENT_3D ( 'NONE', #89200, #118010, #28359 ) ;
#89329 = ADVANCED_FACE ( 'NONE', ( #93312 ), #17551, .T. ) ;
#89328 = CARTESIAN_POINT ( 'NONE',  ( -4.400000000000025224, 2.500000000000000000, -0.2464101615137783419 ) ) ;
#89331 = VERTEX_POINT ( 'NONE', #112950 ) ;
#89330 = FACE_OUTER_BOUND ( 'NONE', #31088, .T. ) ;
#89332 = DIRECTION ( 'NONE',  ( -0.000000000000000000, -1.000000000000000000, -0.000000000000000000 ) ) ;
#89333 = DIRECTION ( 'NONE',  ( -0.000000000000000000, 1.000000000000000000, -0.000000000000000000 ) ) ;
#89334 = EDGE_CURVE ( 'NONE', #96595, #45172, #94936, .T. ) ;
#89335 = ORIENTED_EDGE ( 'NONE', *, *, #111164, .F. ) ;
#89336 = CONICAL_SURFACE ( 'NONE', #43670, 0.09999999999999999167, 0.003490658503988666988 ) ;
#89337 = VERTEX_POINT ( 'NONE', #82202 ) ;
#89338 = EDGE_LOOP ( 'NONE', ( #82658, #29060, #59650, #96321 ) ) ;
#89339 = DIRECTION ( 'NONE',  ( -0.000000000000000000, 1.000000000000000000, -0.000000000000000000 ) ) ;
#89340 = DIRECTION ( 'NONE',  ( -0.000000000000000000, 1.000000000000000000, -0.000000000000000000 ) ) ;
#89341 = DIRECTION ( 'NONE',  ( -4.274815082592931898E-19, -0.9999939076577903929, -0.003490651415223739937 ) ) ;
#89342 = FACE_BOUND ( 'NONE', #89749, .T. ) ;
#89343 = ORIENTED_EDGE ( 'NONE', *, *, #105207, .F. ) ;
#89344 = AXIS2_PLACEMENT_3D ( 'NONE', #107251, #99381, #39189 ) ;
#89345 = DIRECTION ( 'NONE',  ( 0.000000000000000000, 0.000000000000000000, -1.000000000000000000 ) ) ;
#89346 = CARTESIAN_POINT ( 'NONE',  ( -10.00000000000000711, 2.500000000000000000, -3.737306695894645259 ) ) ;
#89347 = AXIS2_PLACEMENT_3D ( 'NONE', #62201, #100796, #11129 ) ;
#89348 = ORIENTED_EDGE ( 'NONE', *, *, #28275, .F. ) ;
#89349 = DIRECTION ( 'NONE',  ( 0.000000000000000000, 1.000000000000000000, 0.000000000000000000 ) ) ;
#89350 = CARTESIAN_POINT ( 'NONE',  ( -15.39999999999998082, 12.50000000000000000, 0.6277270498435143509 ) ) ;
#89351 = STYLED_ITEM ( 'NONE', ( #9462 ), #12695 ) ;
#89352 = DIRECTION ( 'NONE',  ( 0.000000000000000000, -0.9999939076577903929, 0.003490651415223739937 ) ) ;
#89353 = DIRECTION ( 'NONE',  ( -0.000000000000000000, 1.000000000000000000, -0.000000000000000000 ) ) ;
#89354 = CARTESIAN_POINT ( 'NONE',  ( -10.85000000000000142, 12.50000000000000000, -5.737276932171709198 ) ) ;
#89355 = CARTESIAN_POINT ( 'NONE',  ( 14.79999999999989413, 2.500000000000000000, -0.4464101615137782142 ) ) ;
#89356 = CIRCLE ( 'NONE', #120659, 0.06509327318403745899 ) ;
#89357 = CARTESIAN_POINT ( 'NONE',  ( 7.499999999999961808, 12.50000000000000000, 4.330127018922196314 ) ) ;
#89358 = AXIS2_PLACEMENT_3D ( 'NONE', #65856, #108991, #39656 ) ;
#89359 = CONICAL_SURFACE ( 'NONE', #101879, 0.09999999999999982514, 0.003490658503988666988 ) ;
#89360 = CIRCLE ( 'NONE', #108132, 0.06509327318403745899 ) ;
#89361 = EDGE_LOOP ( 'NONE', ( #84357, #114613 ) ) ;
#89362 = ORIENTED_EDGE ( 'NONE', *, *, #28109, .F. ) ;
#89363 = ORIENTED_EDGE ( 'NONE', *, *, #111451, .F. ) ;
#89364 = ORIENTED_EDGE ( 'NONE', *, *, #92037, .F. ) ;
#89365 = ORIENTED_EDGE ( 'NONE', *, *, #87513, .T. ) ;
#89366 = CARTESIAN_POINT ( 'NONE',  ( -0.8500000000000382805, 12.50000000000000000, -1.407149913249512663 ) ) ;
#89367 = CARTESIAN_POINT ( 'NONE',  ( -4.293440603042597559E-14, 12.50000000000000000, 5.022947341949748790 ) ) ;
#89368 = CONICAL_SURFACE ( 'NONE', #87199, 0.09999999999999982514, 0.003490658503988666988 ) ;
#89369 = ORIENTED_EDGE ( 'NONE', *, *, #79630, .F. ) ;
#89370 = FACE_BOUND ( 'NONE', #11902, .T. ) ;
#89371 = DIRECTION ( 'NONE',  ( -0.000000000000000000, 1.000000000000000000, -0.000000000000000000 ) ) ;
#89372 = ADVANCED_FACE ( 'NONE', ( #65114 ), #34311, .T. ) ;
#89374 = AXIS2_PLACEMENT_3D ( 'NONE', #3727, #51560, #13542 ) ;
#89373 = AXIS2_PLACEMENT_3D ( 'NONE', #66387, #65736, #106315 ) ;
#89375 = CARTESIAN_POINT ( 'NONE',  ( 142.3152275665817115, 2.500000000000000000, 2.763522878056728693 ) ) ;
#89376 = ADVANCED_FACE ( 'NONE', ( #2324 ), #43586, .T. ) ;
#89377 = CARTESIAN_POINT ( 'NONE',  ( 3.099999999999943245, 2.500000000000000000, 3.983716857408420076 ) ) ;
#89378 = CARTESIAN_POINT ( 'NONE',  ( -8.150000000000012790, 2.500000000000000000, -2.611473670974877592 ) ) ;
#89379 = DIRECTION ( 'NONE',  ( 0.000000000000000000, 0.000000000000000000, 1.000000000000000000 ) ) ;
#89380 = CARTESIAN_POINT ( 'NONE',  ( -10.65000000000000391, 12.50000000000000000, -1.818653347947322141 ) ) ;
#89381 = ORIENTED_EDGE ( 'NONE', *, *, #100842, .T. ) ;
#89382 = EDGE_CURVE ( 'NONE', #24998, #45239, #89673, .T. ) ;
#89383 = ORIENTED_EDGE ( 'NONE', *, *, #4191, .T. ) ;
#89384 = ORIENTED_EDGE ( 'NONE', *, *, #40358, .F. ) ;
#89385 = ORIENTED_EDGE ( 'NONE', *, *, #43511, .F. ) ;
#89386 = CARTESIAN_POINT ( 'NONE',  ( 12.31005523242794375, 2.499999999999999112, 7.488833079370742496 ) ) ;
#89387 = CARTESIAN_POINT ( 'NONE',  ( 11.69999999999990870, 12.50000000000000000, 4.330127018922196314 ) ) ;
#89388 = ORIENTED_EDGE ( 'NONE', *, *, #124788, .T. ) ;
#89389 = CONICAL_SURFACE ( 'NONE', #93498, 0.1000000000000002554, 0.003490658503988666988 ) ;
#89390 = CARTESIAN_POINT ( 'NONE',  ( -2.300000000000032685, 12.50000000000000000, -0.3464101615137783474 ) ) ;
#89391 = DIRECTION ( 'NONE',  ( -4.274815082592931898E-19, -0.9999939076577903929, -0.003490651415223739937 ) ) ;
#89392 = DIRECTION ( 'NONE',  ( -0.000000000000000000, -1.000000000000000000, -0.000000000000000000 ) ) ;
#89393 = CARTESIAN_POINT ( 'NONE',  ( 184.9843750003414016, -8.734944146203032389, -1.604583208406768146E-15 ) ) ;
#89394 = CARTESIAN_POINT ( 'NONE',  ( -2.900000000000029665, 2.500000000000000000, 3.537306695894645081 ) ) ;
#89395 = DIRECTION ( 'NONE',  ( 0.000000000000000000, 0.000000000000000000, 1.000000000000000000 ) ) ;
#89396 = DIRECTION ( 'NONE',  ( 0.000000000000000000, 1.000000000000000000, 0.000000000000000000 ) ) ;
#89397 = ORIENTED_EDGE ( 'NONE', *, *, #114497, .T. ) ;
#89398 = CARTESIAN_POINT ( 'NONE',  ( 5.599999999999933031, 2.500000000000000000, -0.3464101615137783474 ) ) ;
#89399 = VERTEX_POINT ( 'NONE', #17961 ) ;
#89400 = AXIS2_PLACEMENT_3D ( 'NONE', #52594, #32346, #72889 ) ;
#89401 = EDGE_LOOP ( 'NONE', ( #20971, #49376, #84206, #43635 ) ) ;
#89402 = DIRECTION ( 'NONE',  ( 0.000000000000000000, -0.9999939076577903929, 0.003490651415223739937 ) ) ;
#89403 = DIRECTION ( 'NONE',  ( 0.000000000000000000, 0.000000000000000000, -1.000000000000000000 ) ) ;
#89404 = DIRECTION ( 'NONE',  ( 0.000000000000000000, 0.000000000000000000, 1.000000000000000000 ) ) ;
#89405 = ORIENTED_EDGE ( 'NONE', *, *, #32016, .F. ) ;
#89406 = ORIENTED_EDGE ( 'NONE', *, *, #104529, .F. ) ;
#89407 = ADVANCED_FACE ( 'NONE', ( #27776 ), #12296, .T. ) ;
#89408 = DIRECTION ( 'NONE',  ( -0.000000000000000000, -1.000000000000000000, -0.000000000000000000 ) ) ;
#89409 = CIRCLE ( 'NONE', #66321, 0.06509327318403745899 ) ;
#89410 = AXIS2_PLACEMENT_3D ( 'NONE', #61718, #112097, #32269 ) ;
#89411 = CARTESIAN_POINT ( 'NONE',  ( 6.449999999999928235, 2.500000000000000000, 2.511473670974873507 ) ) ;
#89412 = DIRECTION ( 'NONE',  ( -0.000000000000000000, 1.000000000000000000, -0.000000000000000000 ) ) ;
#89413 = CARTESIAN_POINT ( 'NONE',  ( 4.149999999999939959, 12.50000000000000000, -6.495190528383302464 ) ) ;
#89414 = ORIENTED_EDGE ( 'NONE', *, *, #79572, .F. ) ;
#89415 = FACE_OUTER_BOUND ( 'NONE', #36502, .T. ) ;
#89416 = EDGE_LOOP ( 'NONE', ( #32549, #52925, #14419, #66026 ) ) ;
#89417 = DIRECTION ( 'NONE',  ( 0.000000000000000000, 1.000000000000000000, 0.000000000000000000 ) ) ;
#89418 = CONICAL_SURFACE ( 'NONE', #43464, 0.1000000000000000472, 0.003490658503988666988 ) ;
#89419 = ORIENTED_EDGE ( 'NONE', *, *, #6107, .T. ) ;
#89420 = CARTESIAN_POINT ( 'NONE',  ( 43.29488993686067033, -3.510952053399744255, 3.940495137596863984 ) ) ;
#89421 = FACE_OUTER_BOUND ( 'NONE', #97490, .T. ) ;
#89422 = ADVANCED_FACE ( 'NONE', ( #45514 ), #78189, .T. ) ;
#89423 = AXIS2_PLACEMENT_3D ( 'NONE', #4250, #35675, #35047 ) ;
#89424 = EDGE_CURVE ( 'NONE', #1125, #70010, #116800, .T. ) ;
#89425 = DIRECTION ( 'NONE',  ( 0.000000000000000000, 1.000000000000000000, 0.000000000000000000 ) ) ;
#89426 = EDGE_LOOP ( 'NONE', ( #38034, #68941 ) ) ;
#89427 = DIRECTION ( 'NONE',  ( -0.000000000000000000, -1.000000000000000000, -0.000000000000000000 ) ) ;
#89428 = CIRCLE ( 'NONE', #51781, 0.1000000000000002554 ) ;
#89429 = VERTEX_POINT ( 'NONE', #85418 ) ;
#89430 = ORIENTED_EDGE ( 'NONE', *, *, #24125, .F. ) ;
#89431 = EDGE_CURVE ( 'NONE', #76810, #13985, #33260, .T. ) ;
#89432 = CARTESIAN_POINT ( 'NONE',  ( -13.74999999999998757, 2.500000000000000000, -2.857883832488651521 ) ) ;
#89433 = CARTESIAN_POINT ( 'NONE',  ( 3.349999999999943689, 12.50000000000000000, 2.165063509461097713 ) ) ;
#89434 = CARTESIAN_POINT ( 'NONE',  ( 19.01901804971413767, 2.576149587736929369, 2.431039412660860766 ) ) ;
#89435 = FACE_OUTER_BOUND ( 'NONE', #57711, .T. ) ;
#89436 = CONICAL_SURFACE ( 'NONE', #81035, 0.1000000000000000472, 0.003490658503988666988 ) ;
#89438 = AXIS2_PLACEMENT_3D ( 'NONE', #91655, #81204, #123057 ) ;
#89437 = CARTESIAN_POINT ( 'NONE',  ( 3.949999999999941558, 2.500000000000000000, -6.148780366869526226 ) ) ;
#89439 = DIRECTION ( 'NONE',  ( 0.000000000000000000, 0.000000000000000000, 1.000000000000000000 ) ) ;
#89440 = VECTOR ( 'NONE', #66289, 1000.000000000000000 ) ;
#89441 = CARTESIAN_POINT ( 'NONE',  ( -8.100000000000013856, 12.50000000000000000, -3.983716857408426293 ) ) ;
#89442 = LINE ( 'NONE', #129398, #63837 ) ;
#89443 = CARTESIAN_POINT ( 'NONE',  ( -2.500000000000030642, 2.500000000000000000, -0.6928203230275541413 ) ) ;
#89444 = CIRCLE ( 'NONE', #112442, 0.09999999999999999167 ) ;
#89445 = AXIS2_PLACEMENT_3D ( 'NONE', #91954, #21940, #93249 ) ;
#89446 = VECTOR ( 'NONE', #87537, 1000.000000000000000 ) ;
#89447 = ORIENTED_EDGE ( 'NONE', *, *, #73825, .F. ) ;
#89448 = CARTESIAN_POINT ( 'NONE',  ( -13.34999999999999076, 2.500000000000000000, 2.757883832488653209 ) ) ;
#89449 = AXIS2_PLACEMENT_3D ( 'NONE', #97292, #38395, #19359 ) ;
#89450 = CARTESIAN_POINT ( 'NONE',  ( -11.44999999999999751, 2.500000000000000000, 2.411473670974873862 ) ) ;
#89451 = DIRECTION ( 'NONE',  ( -0.000000000000000000, 1.000000000000000000, -0.000000000000000000 ) ) ;
#89452 = CARTESIAN_POINT ( 'NONE',  ( 3.349999999999943689, 2.500000000000000000, 2.265063509461097357 ) ) ;
#89453 = PLANE ( 'NONE',  #108680 ) ;
#89454 = ORIENTED_EDGE ( 'NONE', *, *, #88631, .T. ) ;
#89455 = DIRECTION ( 'NONE',  ( -0.000000000000000000, 1.000000000000000000, -0.000000000000000000 ) ) ;
#89456 = ADVANCED_FACE ( 'NONE', ( #86038 ), #27146, .T. ) ;
#89458 = AXIS2_PLACEMENT_3D ( 'NONE', #18702, #58647, #128700 ) ;
#89457 = CIRCLE ( 'NONE', #87299, 0.09999999999999982514 ) ;
#89459 = DIRECTION ( 'NONE',  ( 0.000000000000000000, 1.000000000000000000, 0.000000000000000000 ) ) ;
#89461 = VERTEX_POINT ( 'NONE', #75584 ) ;
#89460 = FACE_OUTER_BOUND ( 'NONE', #20832, .T. ) ;
#89462 = EDGE_CURVE ( 'NONE', #56667, #10308, #117421, .T. ) ;
#89463 = EDGE_CURVE ( 'NONE', #129515, #95931, #118912, .T. ) ;
#89464 = ORIENTED_EDGE ( 'NONE', *, *, #99337, .T. ) ;
#89465 = PLANE ( 'NONE',  #19678 ) ;
#89466 = ORIENTED_EDGE ( 'NONE', *, *, #103004, .F. ) ;
#89467 = EDGE_LOOP ( 'NONE', ( #75715, #105419 ) ) ;
#89468 = ORIENTED_EDGE ( 'NONE', *, *, #125179, .F. ) ;
#89469 = CARTESIAN_POINT ( 'NONE',  ( 9.349999999999919709, 2.500000000000000000, -6.741600689897078169 ) ) ;
#89470 = EDGE_CURVE ( 'NONE', #124980, #76747, #97811, .T. ) ;
#89471 = EDGE_CURVE ( 'NONE', #46350, #93541, #98067, .T. ) ;
#89472 = EDGE_CURVE ( 'NONE', #5769, #114671, #45764, .T. ) ;
#89473 = CARTESIAN_POINT ( 'NONE',  ( 105.0000000000000142, 8.500000000000000000, 0.2500000000000003886 ) ) ;
#89474 = DIRECTION ( 'NONE',  ( 0.000000000000000000, 0.000000000000000000, 1.000000000000000000 ) ) ;
#89475 = DIRECTION ( 'NONE',  ( 0.000000000000000000, 1.000000000000000000, 0.000000000000000000 ) ) ;
#89476 = ORIENTED_EDGE ( 'NONE', *, *, #67845, .T. ) ;
#89477 = ADVANCED_FACE ( 'NONE', ( #5556 ), #31197, .T. ) ;
#89478 = CARTESIAN_POINT ( 'NONE',  ( -5.600000000000020073, 12.50000000000000000, 3.983716857408420964 ) ) ;
#89479 = ORIENTED_EDGE ( 'NONE', *, *, #13180, .F. ) ;
#89480 = DIRECTION ( 'NONE',  ( 0.000000000000000000, 1.000000000000000000, 0.000000000000000000 ) ) ;
#89481 = AXIS2_PLACEMENT_3D ( 'NONE', #17555, #88209, #57502 ) ;
#89482 = CARTESIAN_POINT ( 'NONE',  ( 19.72570408286463106, 0.6078483229320776893, 4.299616118078733784 ) ) ;
#89483 = CARTESIAN_POINT ( 'NONE',  ( -0.8500000000000382805, 2.500000000000000000, -5.702370205355749455 ) ) ;
#89484 = DIRECTION ( 'NONE',  ( 0.000000000000000000, 0.000000000000000000, 1.000000000000000000 ) ) ;
#89485 = EDGE_CURVE ( 'NONE', #126098, #123229, #83424, .T. ) ;
#89486 = ORIENTED_EDGE ( 'NONE', *, *, #45344, .F. ) ;
#89487 = CONICAL_SURFACE ( 'NONE', #12114, 0.09999999999999982514, 0.003490658503988666988 ) ;
#89488 = CIRCLE ( 'NONE', #33081, 0.06509327318403745899 ) ;
#89489 = ORIENTED_EDGE ( 'NONE', *, *, #59632, .F. ) ;
#89490 = EDGE_LOOP ( 'NONE', ( #34297, #10494, #43088, #35789 ) ) ;
#89491 = VERTEX_POINT ( 'NONE', #46794 ) ;
#89492 = ORIENTED_EDGE ( 'NONE', *, *, #26434, .F. ) ;
#89493 = DIRECTION ( 'NONE',  ( 0.000000000000000000, 0.000000000000000000, -1.000000000000000000 ) ) ;
#89494 = CARTESIAN_POINT ( 'NONE',  ( -1.700000000000035261, 2.500000000000000000, 4.330127018922196314 ) ) ;
#89495 = CARTESIAN_POINT ( 'NONE',  ( -12.49999999999999289, 2.500000000000000000, 5.022947341949748790 ) ) ;
#89496 = FACE_BOUND ( 'NONE', #86346, .T. ) ;
#89497 = CARTESIAN_POINT ( 'NONE',  ( 3.749999999999944045, 2.500000000000000000, -2.857883832488653741 ) ) ;
#89498 = CARTESIAN_POINT ( 'NONE',  ( -8.350000000000013856, 2.500000000000000000, -7.088010851410848190 ) ) ;
#89499 = CIRCLE ( 'NONE', #47742, 0.09999999999999999167 ) ;
#89500 = DIRECTION ( 'NONE',  ( 0.000000000000000000, 1.000000000000000000, 0.000000000000000000 ) ) ;
#89501 = FACE_OUTER_BOUND ( 'NONE', #121094, .T. ) ;
#89502 = CARTESIAN_POINT ( 'NONE',  ( 10.64999999999990976, 2.500000000000000000, -6.741600689897077281 ) ) ;
#89503 = CARTESIAN_POINT ( 'NONE',  ( -10.20000000000000462, 2.500000000000000000, 0.3464101615137735735 ) ) ;
#89504 = CARTESIAN_POINT ( 'NONE',  ( -3.350000000000028511, 2.500000000000000000, 1.472243186433545459 ) ) ;
#89505 = AXIS2_PLACEMENT_3D ( 'NONE', #113184, #34663, #86297 ) ;
#89506 = LINE ( 'NONE', #99338, #70265 ) ;
#89507 = ORIENTED_EDGE ( 'NONE', *, *, #71456, .F. ) ;
#89508 = ORIENTED_EDGE ( 'NONE', *, *, #105848, .T. ) ;
#89509 = ORIENTED_EDGE ( 'NONE', *, *, #28852, .F. ) ;
#89510 = ORIENTED_EDGE ( 'NONE', *, *, #53399, .T. ) ;
#89511 = CIRCLE ( 'NONE', #97914, 0.06509327318403745899 ) ;
#89512 = DIRECTION ( 'NONE',  ( 0.000000000000000000, 0.000000000000000000, 1.000000000000000000 ) ) ;
#89513 = CARTESIAN_POINT ( 'NONE',  ( 7.949999999999925571, 12.50000000000000000, -6.495190528383302464 ) ) ;
#89514 = FACE_BOUND ( 'NONE', #115004, .T. ) ;
#89515 = DIRECTION ( 'NONE',  ( -0.000000000000000000, 1.000000000000000000, -0.000000000000000000 ) ) ;
#89516 = AXIS2_PLACEMENT_3D ( 'NONE', #41168, #79777, #50318 ) ;
#89517 = EDGE_CURVE ( 'NONE', #17700, #23794, #79220, .T. ) ;
#89518 = EDGE_LOOP ( 'NONE', ( #101188, #29358 ) ) ;
#89519 = CARTESIAN_POINT ( 'NONE',  ( 9.149999999999920419, 2.500000000000000000, -5.702370205355749455 ) ) ;
#89520 = DIRECTION ( 'NONE',  ( -4.274815082592931898E-19, -0.9999939076577903929, -0.003490651415223739937 ) ) ;
#89521 = DIRECTION ( 'NONE',  ( 0.000000000000000000, 0.000000000000000000, -1.000000000000000000 ) ) ;
#89522 = CARTESIAN_POINT ( 'NONE',  ( -9.350000000000006750, 12.50000000000000000, -1.753560074763288457 ) ) ;
#89523 = AXIS2_PLACEMENT_3D ( 'NONE', #75535, #97770, #8091 ) ;
#89524 = EDGE_LOOP ( 'NONE', ( #25018, #36566 ) ) ;
#89525 = AXIS2_PLACEMENT_3D ( 'NONE', #72361, #35026, #3606 ) ;
#89526 = DIRECTION ( 'NONE',  ( 0.000000000000000000, -0.000000000000000000, 1.000000000000000000 ) ) ;
#89527 = ADVANCED_FACE ( 'NONE', ( #38265 ), #93879, .T. ) ;
#89528 = AXIS2_PLACEMENT_3D ( 'NONE', #111342, #30897, #100265 ) ;
#89529 = ORIENTED_EDGE ( 'NONE', *, *, #3179, .F. ) ;
#89530 = VERTEX_POINT ( 'NONE', #95248 ) ;
#89531 = CARTESIAN_POINT ( 'NONE',  ( 5.649999999999936406, 12.50000000000000000, -6.906693963081115051 ) ) ;
#89532 = DIRECTION ( 'NONE',  ( 0.000000000000000000, 0.000000000000000000, 1.000000000000000000 ) ) ;
#89533 = VERTEX_POINT ( 'NONE', #65767 ) ;
#89534 = DIRECTION ( 'NONE',  ( 0.000000000000000000, 0.000000000000000000, 1.000000000000000000 ) ) ;
#89535 = CARTESIAN_POINT ( 'NONE',  ( 179.5000000000000000, -0.6250000000000025535, -6.000000000000000888 ) ) ;
#89536 = ORIENTED_EDGE ( 'NONE', *, *, #125660, .F. ) ;
#89537 = CARTESIAN_POINT ( 'NONE',  ( -11.69999999999999929, 12.50000000000000000, -4.330127018922198978 ) ) ;
#89538 = ORIENTED_EDGE ( 'NONE', *, *, #71889, .F. ) ;
#89539 = AXIS2_PLACEMENT_3D ( 'NONE', #123162, #111382, #61676 ) ;
#89540 = FACE_OUTER_BOUND ( 'NONE', #103697, .T. ) ;
#89541 = ORIENTED_EDGE ( 'NONE', *, *, #62258, .T. ) ;
#89542 = DIRECTION ( 'NONE',  ( 0.000000000000000000, 1.000000000000000000, 0.000000000000000000 ) ) ;
#89543 = FACE_BOUND ( 'NONE', #78427, .T. ) ;
#89545 = VECTOR ( 'NONE', #124253, 1000.000000000000000 ) ;
#89544 = AXIS2_PLACEMENT_3D ( 'NONE', #26324, #21486, #7298 ) ;
#89546 = ORIENTED_EDGE ( 'NONE', *, *, #119017, .F. ) ;
#89547 = CARTESIAN_POINT ( 'NONE',  ( 111.0560539298719647, 6.600968029026939021, 3.970093675385399479 ) ) ;
#89548 = ORIENTED_EDGE ( 'NONE', *, *, #96140, .F. ) ;
#89549 = DIRECTION ( 'NONE',  ( 0.000000000000000000, 0.000000000000000000, 1.000000000000000000 ) ) ;
#89550 = CARTESIAN_POINT ( 'NONE',  ( -1.650000000000034328, 12.50000000000000000, -6.430097255199264339 ) ) ;
#89551 = SHAPE_REPRESENTATION ( 'Multi-Function Power _ Mode Button', ( #108296 ), #5971 ) ;
#89552 = FACE_OUTER_BOUND ( 'NONE', #87000, .T. ) ;
#89553 = CARTESIAN_POINT ( 'NONE',  ( 7.099999999999925926, 2.500000000000000000, 0.5928203230275495006 ) ) ;
#89554 = DIRECTION ( 'NONE',  ( 0.000000000000000000, 0.000000000000000000, -1.000000000000000000 ) ) ;
#89555 = ORIENTED_EDGE ( 'NONE', *, *, #8606, .T. ) ;
#89556 = ORIENTED_EDGE ( 'NONE', *, *, #60791, .T. ) ;
#89558 = ORIENTED_EDGE ( 'NONE', *, *, #14084, .F. ) ;
#89557 = ADVANCED_FACE ( 'NONE', ( #16655 ), #8179, .T. ) ;
#89559 = CARTESIAN_POINT ( 'NONE',  ( 0.8499999999999545697, 2.500000000000000000, 2.857883832488649301 ) ) ;
#89560 = CARTESIAN_POINT ( 'NONE',  ( -2.700000000000031264, 12.50000000000000000, 4.741630453620009789 ) ) ;
#89561 = CARTESIAN_POINT ( 'NONE',  ( -7.100000000000017408, 2.500000000000000000, -5.022947341949754119 ) ) ;
#89564 = ORIENTED_EDGE ( 'NONE', *, *, #119416, .T. ) ;
#89563 = VERTEX_POINT ( 'NONE', #96502 ) ;
#89562 = CIRCLE ( 'NONE', #102086, 0.09999999999999999167 ) ;
#89565 = EDGE_LOOP ( 'NONE', ( #102615, #101690 ) ) ;
#89566 = DIRECTION ( 'NONE',  ( 0.000000000000000000, -0.9999939076577903929, 0.003490651415223739937 ) ) ;
#89567 = ORIENTED_EDGE ( 'NONE', *, *, #67389, .F. ) ;
#89569 = EDGE_CURVE ( 'NONE', #91861, #87824, #37454, .T. ) ;
#89568 = DIRECTION ( 'NONE',  ( 0.000000000000000000, 0.000000000000000000, 1.000000000000000000 ) ) ;
#89570 = CONICAL_SURFACE ( 'NONE', #33147, 0.1000000000000002554, 0.003490658503988666988 ) ;
#89572 = CARTESIAN_POINT ( 'NONE',  ( -11.24999999999996270, 12.50000000000000000, 2.165063509461097713 ) ) ;
#89571 = VECTOR ( 'NONE', #6182, 1000.000000000000000 ) ;
#89573 = DIRECTION ( 'NONE',  ( 0.000000000000000000, 0.000000000000000000, -1.000000000000000000 ) ) ;
#89574 = AXIS2_PLACEMENT_3D ( 'NONE', #97451, #7773, #68634 ) ;
#89575 = PLANE ( 'NONE',  #109186 ) ;
#89576 = LINE ( 'NONE', #79754, #19987 ) ;
#89577 = CARTESIAN_POINT ( 'NONE',  ( -12.09999999999999609, 2.500000000000000000, -5.122947341949751987 ) ) ;
#89578 = EDGE_CURVE ( 'NONE', #13125, #119700, #49383, .T. ) ;
#89579 = EDGE_CURVE ( 'NONE', #96780, #3042, #47918, .T. ) ;
#89580 = CARTESIAN_POINT ( 'NONE',  ( -8.550000000000011369, 12.50000000000000000, -2.446380397790840266 ) ) ;
#89581 = VECTOR ( 'NONE', #65563, 1000.000000000000000 ) ;
#89582 = ORIENTED_EDGE ( 'NONE', *, *, #22732, .F. ) ;
#89584 = ORIENTED_EDGE ( 'NONE', *, *, #17803, .F. ) ;
#89583 = CONICAL_SURFACE ( 'NONE', #12197, 0.09999999999999982514, 0.003490658503988666988 ) ;
#89586 = CARTESIAN_POINT ( 'NONE',  ( 9.149999999999916866, 2.500000000000000000, 5.802370205355744659 ) ) ;
#89585 = VECTOR ( 'NONE', #45211, 1000.000000000000000 ) ;
#89587 = ADVANCED_FACE ( 'NONE', ( #89921 ), #69644, .F. ) ;
#89588 = LINE ( 'NONE', #122115, #25666 ) ;
#89589 = ORIENTED_EDGE ( 'NONE', *, *, #109184, .F. ) ;
#89590 = ORIENTED_EDGE ( 'NONE', *, *, #31645, .F. ) ;
#89591 = ADVANCED_FACE ( 'NONE', ( #78845 ), #24919, .T. ) ;
#89592 = CARTESIAN_POINT ( 'NONE',  ( 186.7760416670080588, 6.551208109652274736, 3.782341765625001351 ) ) ;
#89593 = DIRECTION ( 'NONE',  ( -0.000000000000000000, 1.000000000000000000, -0.000000000000000000 ) ) ;
#89594 = DIRECTION ( 'NONE',  ( -4.274815082592931898E-19, -0.9999939076577903929, -0.003490651415223739937 ) ) ;
#89595 = AXIS2_PLACEMENT_3D ( 'NONE', #103178, #3684, #16058 ) ;
#89596 = CARTESIAN_POINT ( 'NONE',  ( -4.800000000000024691, 12.50000000000000000, 0.4115034346978109769 ) ) ;
#89597 = AXIS2_PLACEMENT_3D ( 'NONE', #51776, #32152, #91698 ) ;
#89598 = DIRECTION ( 'NONE',  ( 0.000000000000000000, 1.000000000000000000, 0.000000000000000000 ) ) ;
#89599 = PLANE ( 'NONE',  #88683 ) ;
#89600 = FACE_OUTER_BOUND ( 'NONE', #124540, .T. ) ;
#89601 = DIRECTION ( 'NONE',  ( 0.000000000000000000, 0.000000000000000000, 1.000000000000000000 ) ) ;
#89602 = AXIS2_PLACEMENT_3D ( 'NONE', #66659, #106592, #56825 ) ;
#89603 = VERTEX_POINT ( 'NONE', #120041 ) ;
#89604 = ORIENTED_EDGE ( 'NONE', *, *, #65176, .T. ) ;
#89605 = CLOSED_SHELL ( 'NONE', ( #40130, #128218, #98175, #33446, #22564, #89587, #3749, #20589, #98751, #83636, #86949, #129142, #16019, #111605, #92078, #113651, #58307, #76522, #126752, #24276, #1783, #76625 ) ) ;
#89606 = AXIS2_PLACEMENT_3D ( 'NONE', #59696, #62256, #40697 ) ;
#89607 = ORIENTED_EDGE ( 'NONE', *, *, #41588, .F. ) ;
#89608 = VERTEX_POINT ( 'NONE', #18610 ) ;
#89609 = DIRECTION ( 'NONE',  ( -0.000000000000000000, 1.000000000000000000, -0.000000000000000000 ) ) ;
#89610 = CARTESIAN_POINT ( 'NONE',  ( -10.40000000000000213, 2.500000000000000000, -0.7928203230275542301 ) ) ;
#89611 = VECTOR ( 'NONE', #55478, 1000.000000000000000 ) ;
#89612 = ORIENTED_EDGE ( 'NONE', *, *, #49604, .F. ) ;
#89613 = CARTESIAN_POINT ( 'NONE',  ( 127.5000000000000000, 1.500000000000000000, 2.598076211353316900 ) ) ;
#89614 = ADVANCED_FACE ( 'NONE', ( #61111 ), #118741, .T. ) ;
#89615 = FACE_OUTER_BOUND ( 'NONE', #100189, .T. ) ;
#89616 = CARTESIAN_POINT ( 'NONE',  ( 0.5999999999999560130, 2.500000000000000000, -3.883716857408426648 ) ) ;
#89618 = ORIENTED_EDGE ( 'NONE', *, *, #75141, .F. ) ;
#89617 = CARTESIAN_POINT ( 'NONE',  ( 11.44999999999990514, 12.50000000000000000, 2.511473670974873507 ) ) ;
#89619 = DIRECTION ( 'NONE',  ( -0.000000000000000000, 1.000000000000000000, -0.000000000000000000 ) ) ;
#89620 = EDGE_CURVE ( 'NONE', #89736, #116685, #50648, .T. ) ;
#89621 = CARTESIAN_POINT ( 'NONE',  ( -13.09999999999999254, 12.50000000000000000, -0.2813168883297366696 ) ) ;
#89622 = EDGE_LOOP ( 'NONE', ( #93196, #39897, #109388, #91744 ) ) ;
#89623 = AXIS2_PLACEMENT_3D ( 'NONE', #3348, #43288, #49093 ) ;
#89624 = ORIENTED_EDGE ( 'NONE', *, *, #121521, .T. ) ;
#89625 = ORIENTED_EDGE ( 'NONE', *, *, #20761, .F. ) ;
#89626 = VERTEX_POINT ( 'NONE', #30388 ) ;
#89627 = DIRECTION ( 'NONE',  ( 0.000000000000000000, 1.000000000000000000, 0.000000000000000000 ) ) ;
#89628 = EDGE_CURVE ( 'NONE', #39021, #114247, #127333, .T. ) ;
#89629 = CIRCLE ( 'NONE', #66540, 0.1000000000000002554 ) ;
#89630 = ADVANCED_FACE ( 'NONE', ( #110220 ), #88640, .T. ) ;
#89631 = EDGE_CURVE ( 'NONE', #126381, #20628, #16488, .T. ) ;
#89632 = CARTESIAN_POINT ( 'NONE',  ( -13.54999999999998828, 2.500000000000000000, -2.411473670974875638 ) ) ;
#89633 = DIRECTION ( 'NONE',  ( 0.000000000000000000, 0.000000000000000000, 1.000000000000000000 ) ) ;
#89636 = EDGE_CURVE ( 'NONE', #8732, #43124, #41668, .T. ) ;
#89635 = VECTOR ( 'NONE', #30109, 1000.000000000000000 ) ;
#89634 = AXIS2_PLACEMENT_3D ( 'NONE', #21685, #96048, #83809 ) ;
#89637 = VERTEX_POINT ( 'NONE', #129242 ) ;
#89638 = DIRECTION ( 'NONE',  ( 0.000000000000000000, 1.000000000000000000, 0.000000000000000000 ) ) ;
#89640 = VECTOR ( 'NONE', #112388, 1000.000000000000000 ) ;
#89639 = DIRECTION ( 'NONE',  ( 0.000000000000000000, 0.000000000000000000, -1.000000000000000000 ) ) ;
#89641 = FACE_OUTER_BOUND ( 'NONE', #3626, .T. ) ;
#89642 = DIRECTION ( 'NONE',  ( 0.000000000000000000, 0.000000000000000000, 1.000000000000000000 ) ) ;
#89643 = EDGE_CURVE ( 'NONE', #84351, #50498, #68994, .T. ) ;
#89644 = VERTEX_POINT ( 'NONE', #19912 ) ;
#89647 = ADVANCED_FACE ( 'NONE', ( #91222 ), #108440, .T. ) ;
#89646 = AXIS2_PLACEMENT_3D ( 'NONE', #12976, #92868, #83048 ) ;
#89645 = CIRCLE ( 'NONE', #106362, 0.06509327318403741736 ) ;
#89648 = CARTESIAN_POINT ( 'NONE',  ( 187.4583333333333428, 4.445597072760117285, 7.700000000000001066 ) ) ;
#89649 = EDGE_LOOP ( 'NONE', ( #954, #83570, #68231, #103432 ) ) ;
#89650 = VERTEX_POINT ( 'NONE', #902 ) ;
#89651 = DIRECTION ( 'NONE',  ( 0.000000000000000000, 1.000000000000000000, 0.000000000000000000 ) ) ;
#89652 = CARTESIAN_POINT ( 'NONE',  ( 8.749999999999923617, 12.50000000000000000, 1.472243186433545459 ) ) ;
#89653 = FACE_BOUND ( 'NONE', #22176, .T. ) ;
#89654 = CARTESIAN_POINT ( 'NONE',  ( -3.350000000000028511, 12.50000000000000000, -2.857883832488653741 ) ) ;
#89655 = LINE ( 'NONE', #18320, #59126 ) ;
#89656 = CARTESIAN_POINT ( 'NONE',  ( -9.150000000000009237, 12.50000000000000000, -2.165063509461101710 ) ) ;
#89657 = CIRCLE ( 'NONE', #43712, 0.09999999999999982514 ) ;
#89658 = ORIENTED_EDGE ( 'NONE', *, *, #99843, .F. ) ;
#89659 = DIRECTION ( 'NONE',  ( 0.000000000000000000, 0.000000000000000000, -1.000000000000000000 ) ) ;
#89660 = CARTESIAN_POINT ( 'NONE',  ( 8.149999999999923972, 12.50000000000000000, 2.446380397790835826 ) ) ;
#89661 = PLANE ( 'NONE',  #80033 ) ;
#89662 = FACE_OUTER_BOUND ( 'NONE', #26539, .T. ) ;
#89663 = ORIENTED_EDGE ( 'NONE', *, *, #14070, .T. ) ;
#89664 = CARTESIAN_POINT ( 'NONE',  ( -11.25000000000000000, 12.50000000000000000, -7.188010851410850499 ) ) ;
#89665 = CIRCLE ( 'NONE', #81259, 0.1000000000000002554 ) ;
#89666 = CARTESIAN_POINT ( 'NONE',  ( -12.04999999999999538, 12.50000000000000000, 2.165063509461097713 ) ) ;
#89667 = ORIENTED_EDGE ( 'NONE', *, *, #128052, .T. ) ;
#89668 = ORIENTED_EDGE ( 'NONE', *, *, #110172, .F. ) ;
#89669 = DIRECTION ( 'NONE',  ( 0.000000000000000000, -0.000000000000000000, 1.000000000000000000 ) ) ;
#89670 = DIRECTION ( 'NONE',  ( 0.000000000000000000, 0.000000000000000000, -1.000000000000000000 ) ) ;
#89671 = FACE_BOUND ( 'NONE', #126239, .T. ) ;
#89672 = CARTESIAN_POINT ( 'NONE',  ( -0.6000000000000323963, 2.500000000000000000, 0.2464101615137759549 ) ) ;
#89673 = CIRCLE ( 'NONE', #85456, 7.500000000000000000 ) ;
#89674 = CIRCLE ( 'NONE', #56208, 0.06509327318403745899 ) ;
#89675 = DIRECTION ( 'NONE',  ( 0.000000000000000000, 0.000000000000000000, -1.000000000000000000 ) ) ;
#89676 = EDGE_CURVE ( 'NONE', #40679, #11966, #19236, .T. ) ;
#89677 = ORIENTED_EDGE ( 'NONE', *, *, #110304, .F. ) ;
#89678 = FACE_OUTER_BOUND ( 'NONE', #113917, .T. ) ;
#89679 = CARTESIAN_POINT ( 'NONE',  ( 184.0000000000000000, 0.000000000000000000, 7.700000000000000178 ) ) ;
#89680 = AXIS2_PLACEMENT_3D ( 'NONE', #91269, #31710, #120726 ) ;
#89681 = ORIENTED_EDGE ( 'NONE', *, *, #106889, .F. ) ;
#89682 = DIRECTION ( 'NONE',  ( -1.000000000000000000, 0.000000000000000000, 1.084202172485504434E-16 ) ) ;
#89683 = PLANE ( 'NONE',  #86663 ) ;
#89684 = EDGE_CURVE ( 'NONE', #42781, #41615, #114793, .T. ) ;
#89685 = DIRECTION ( 'NONE',  ( 0.000000000000000000, 0.000000000000000000, 1.000000000000000000 ) ) ;
#89686 = DIRECTION ( 'NONE',  ( -0.000000000000000000, -1.000000000000000000, -0.000000000000000000 ) ) ;
#89687 = CIRCLE ( 'NONE', #99884, 0.06509327318403745899 ) ;
#89688 = VERTEX_POINT ( 'NONE', #41504 ) ;
#89689 = FACE_OUTER_BOUND ( 'NONE', #498, .T. ) ;
#89690 = CARTESIAN_POINT ( 'NONE',  ( 8.749999999999957367, 12.50000000000000000, -6.560283801567339701 ) ) ;
#89691 = DIRECTION ( 'NONE',  ( 0.000000000000000000, 1.000000000000000000, 0.000000000000000000 ) ) ;
#89692 = CIRCLE ( 'NONE', #45882, 0.06509327318403745899 ) ;
#89693 = DIRECTION ( 'NONE',  ( -0.000000000000000000, 1.000000000000000000, -0.000000000000000000 ) ) ;
#89694 = ORIENTED_EDGE ( 'NONE', *, *, #86245, .T. ) ;
#89695 = ORIENTED_EDGE ( 'NONE', *, *, #116820, .F. ) ;
#89696 = CARTESIAN_POINT ( 'NONE',  ( 0.8499999999999545697, 12.50000000000000000, -1.407149913249512663 ) ) ;
#89697 = EDGE_LOOP ( 'NONE', ( #93274, #120748, #71765, #36286 ) ) ;
#89698 = CARTESIAN_POINT ( 'NONE',  ( -6.650000000000014566, 12.50000000000000000, 6.495190528383297135 ) ) ;
#89699 = CARTESIAN_POINT ( 'NONE',  ( 17.50000000000000000, -2.500000000000000000, 4.000000000000001776 ) ) ;
#89700 = DIRECTION ( 'NONE',  ( 0.000000000000000000, 0.000000000000000000, 1.000000000000000000 ) ) ;
#89701 = ORIENTED_EDGE ( 'NONE', *, *, #54398, .F. ) ;
#89702 = AXIS2_PLACEMENT_3D ( 'NONE', #55946, #85411, #96498 ) ;
#89703 = LINE ( 'NONE', #68120, #60026 ) ;
#89704 = CARTESIAN_POINT ( 'NONE',  ( -5.850000000000018296, 2.500000000000000000, 2.857883832488649301 ) ) ;
#89705 = CARTESIAN_POINT ( 'NONE',  ( 5.599999999999933031, 2.500000000000000000, 0.3464101615137735735 ) ) ;
#89706 = CARTESIAN_POINT ( 'NONE',  ( 185.2760416670080588, 6.551208109652274736, 3.782341765625001351 ) ) ;
#89707 = DIRECTION ( 'NONE',  ( 0.000000000000000000, 1.000000000000000000, 0.000000000000000000 ) ) ;
#89708 = AXIS2_PLACEMENT_3D ( 'NONE', #49358, #89255, #129214 ) ;
#89709 = DIRECTION ( 'NONE',  ( -0.000000000000000000, 1.000000000000000000, -0.000000000000000000 ) ) ;
#89711 = ORIENTED_EDGE ( 'NONE', *, *, #23443, .T. ) ;
#89710 = CIRCLE ( 'NONE', #106433, 0.09999999999999982514 ) ;
#89712 = ORIENTED_EDGE ( 'NONE', *, *, #90322, .F. ) ;
#89713 = CARTESIAN_POINT ( 'NONE',  ( 4.999999999999938716, 12.50000000000000000, -4.957854068765716882 ) ) ;
#89714 = ORIENTED_EDGE ( 'NONE', *, *, #71633, .T. ) ;
#89715 = DIRECTION ( 'NONE',  ( 0.000000000000000000, 0.000000000000000000, 1.000000000000000000 ) ) ;
#89717 = ORIENTED_EDGE ( 'NONE', *, *, #63116, .T. ) ;
#89716 = ORIENTED_EDGE ( 'NONE', *, *, #128990, .F. ) ;
#89718 = ORIENTED_EDGE ( 'NONE', *, *, #64217, .F. ) ;
#89719 = FACE_OUTER_BOUND ( 'NONE', #20875, .T. ) ;
#89721 = ADVANCED_FACE ( 'NONE', ( #99115 ), #87598, .T. ) ;
#89720 = FACE_OUTER_BOUND ( 'NONE', #15808, .T. ) ;
#89722 = CARTESIAN_POINT ( 'NONE',  ( 10.39999999999991154, 12.50000000000000000, -3.702399969078687292 ) ) ;
#89723 =( NAMED_UNIT ( * ) PLANE_ANGLE_UNIT ( ) SI_UNIT ( $, .RADIAN. ) );
#89724 = CIRCLE ( 'NONE', #37508, 0.1000000000000002554 ) ;
#89725 = CARTESIAN_POINT ( 'NONE',  ( -10.40000000000000391, 2.500000000000000000, -3.637306695894645614 ) ) ;
#89726 = CARTESIAN_POINT ( 'NONE',  ( 8.149999999999920419, 2.500000000000000000, -1.718653347947325827 ) ) ;
#89727 = CARTESIAN_POINT ( 'NONE',  ( 11.04999999999991012, 2.500000000000000000, 6.741600689897071952 ) ) ;
#89728 = FACE_OUTER_BOUND ( 'NONE', #14268, .T. ) ;
#89729 = DIRECTION ( 'NONE',  ( 0.000000000000000000, 1.000000000000000000, 0.000000000000000000 ) ) ;
#89730 = CONICAL_SURFACE ( 'NONE', #123186, 0.1000000000000002554, 0.003490658503988666988 ) ;
#89731 = EDGE_CURVE ( 'NONE', #50580, #60734, #1923, .T. ) ;
#89732 = EDGE_CURVE ( 'NONE', #93869, #118548, #102963, .T. ) ;
#89733 = CARTESIAN_POINT ( 'NONE',  ( 12.09999999999990550, 2.500000000000000000, 3.637306695894644726 ) ) ;
#89734 = VERTEX_POINT ( 'NONE', #32967 ) ;
#89735 = CIRCLE ( 'NONE', #98046, 0.06509327318403745899 ) ;
#89736 = VERTEX_POINT ( 'NONE', #94427 ) ;
#89737 = EDGE_CURVE ( 'NONE', #92549, #32647, #121062, .T. ) ;
#89739 = ADVANCED_FACE ( 'NONE', ( #32328 ), #93968, .T. ) ;
#89738 = PLANE ( 'NONE',  #63229 ) ;
#89740 = VERTEX_POINT ( 'NONE', #84624 ) ;
#89741 = ORIENTED_EDGE ( 'NONE', *, *, #9466, .F. ) ;
#89742 = EDGE_CURVE ( 'NONE', #80836, #114385, #106486, .T. ) ;
#89743 = CARTESIAN_POINT ( 'NONE',  ( 1.249999999999953815, 2.500000000000000000, 1.472243186433545459 ) ) ;
#89744 = CARTESIAN_POINT ( 'NONE',  ( 187.0312500006828031, 9.429780353434619030E-16, -7.700000000000000178 ) ) ;
#89745 = LINE ( 'NONE', #29539, #117514 ) ;
#89746 = CARTESIAN_POINT ( 'NONE',  ( 115.5000000000000000, 5.000000000000000000, 2.000000000000003553 ) ) ;
#89748 = AXIS2_PLACEMENT_3D ( 'NONE', #92589, #101119, #52652 ) ;
#89747 = CARTESIAN_POINT ( 'NONE',  ( 0.3999999999999619971, 2.500000000000000000, -0.1000000000000001166 ) ) ;
#89749 = EDGE_LOOP ( 'NONE', ( #10872, #18332 ) ) ;
#89750 = VERTEX_POINT ( 'NONE', #82706 ) ;
#89752 = DIRECTION ( 'NONE',  ( -0.000000000000000000, -1.000000000000000000, -0.000000000000000000 ) ) ;
#89751 = AXIS2_PLACEMENT_3D ( 'NONE', #32007, #71929, #62108 ) ;
#89754 = ORIENTED_EDGE ( 'NONE', *, *, #20185, .F. ) ;
#89753 = VECTOR ( 'NONE', #7158, 1000.000000000000000 ) ;
#89755 = DIRECTION ( 'NONE',  ( 0.000000000000000000, 0.000000000000000000, 1.000000000000000000 ) ) ;
#89756 = EDGE_LOOP ( 'NONE', ( #113983, #2940, #31599, #19314 ) ) ;
#89757 = ORIENTED_EDGE ( 'NONE', *, *, #37211, .T. ) ;
#89759 = CIRCLE ( 'NONE', #41755, 0.09999999999999982514 ) ;
#89758 = DIRECTION ( 'NONE',  ( -0.000000000000000000, 1.000000000000000000, -0.000000000000000000 ) ) ;
#89760 = CARTESIAN_POINT ( 'NONE',  ( 48.81612456492383956, -3.619496399135579523, -4.312668942933988170 ) ) ;
#89761 = AXIS2_PLACEMENT_3D ( 'NONE', #69782, #120179, #1674 ) ;
#89762 = DIRECTION ( 'NONE',  ( 0.000000000000000000, 0.000000000000000000, 1.000000000000000000 ) ) ;
#89763 = CARTESIAN_POINT ( 'NONE',  ( 10.84999999999991260, 12.50000000000000000, -2.857883832488653741 ) ) ;
#89764 = DIRECTION ( 'NONE',  ( -0.000000000000000000, 1.000000000000000000, -0.000000000000000000 ) ) ;
#89765 = ORIENTED_EDGE ( 'NONE', *, *, #108976, .T. ) ;
#89766 = CARTESIAN_POINT ( 'NONE',  ( 6.899999999999926636, 2.500000000000000000, 0.3464101615137736845 ) ) ;
#89767 = DIRECTION ( 'NONE',  ( -0.000000000000000000, 1.000000000000000000, -0.000000000000000000 ) ) ;
#89768 = DIRECTION ( 'NONE',  ( -0.000000000000000000, -1.000000000000000000, -0.000000000000000000 ) ) ;
#89769 = DIRECTION ( 'NONE',  ( 0.000000000000000000, 1.000000000000000000, 0.000000000000000000 ) ) ;
#89770 = AXIS2_PLACEMENT_3D ( 'NONE', #115386, #45403, #3532 ) ;
#89771 = LINE ( 'NONE', #9285, #20622 ) ;
#89772 = ORIENTED_EDGE ( 'NONE', *, *, #35563, .F. ) ;
#89773 = AXIS2_PLACEMENT_3D ( 'NONE', #19787, #28317, #19107 ) ;
#89774 = EDGE_LOOP ( 'NONE', ( #122777, #62100 ) ) ;
#89775 = EDGE_CURVE ( 'NONE', #127091, #39885, #54260, .T. ) ;
#89776 = DIRECTION ( 'NONE',  ( 0.000000000000000000, 0.000000000000000000, 1.000000000000000000 ) ) ;
#89777 = EDGE_CURVE ( 'NONE', #39666, #86814, #50073, .T. ) ;
#89778 = ADVANCED_FACE ( 'NONE', ( #63050 ), #111495, .T. ) ;
#89779 = ORIENTED_EDGE ( 'NONE', *, *, #105094, .T. ) ;
#89780 = DIRECTION ( 'NONE',  ( 0.000000000000000000, 0.000000000000000000, 1.000000000000000000 ) ) ;
#89781 = DIRECTION ( 'NONE',  ( -4.274815082592931898E-19, -0.9999939076577903929, -0.003490651415223739937 ) ) ;
#89782 = AXIS2_PLACEMENT_3D ( 'NONE', #62368, #3428, #32274 ) ;
#89783 = EDGE_CURVE ( 'NONE', #85004, #46456, #123886, .T. ) ;
#89784 = ORIENTED_EDGE ( 'NONE', *, *, #56808, .F. ) ;
#89785 = DIRECTION ( 'NONE',  ( -0.000000000000000000, -1.000000000000000000, -0.000000000000000000 ) ) ;
#89786 = DIRECTION ( 'NONE',  ( 0.000000000000000000, 0.000000000000000000, -1.000000000000000000 ) ) ;
#89787 = EDGE_CURVE ( 'NONE', #102432, #10582, #108627, .T. ) ;
#89788 = DIRECTION ( 'NONE',  ( 0.000000000000000000, -0.000000000000000000, 1.000000000000000000 ) ) ;
#89789 = DIRECTION ( 'NONE',  ( 0.000000000000000000, -0.000000000000000000, 1.000000000000000000 ) ) ;
#89790 = EDGE_CURVE ( 'NONE', #75194, #84422, #122620, .T. ) ;
#89791 = ADVANCED_FACE ( 'NONE', ( #72242 ), #45853, .T. ) ;
#89792 = EDGE_CURVE ( 'NONE', #65438, #55788, #93168, .T. ) ;
#89793 = DIRECTION ( 'NONE',  ( 0.000000000000000000, 0.000000000000000000, 1.000000000000000000 ) ) ;
#89794 = ORIENTED_EDGE ( 'NONE', *, *, #45440, .F. ) ;
#89795 = CARTESIAN_POINT ( 'NONE',  ( 43.31977652052934502, 2.029676442637600164, -5.113281004118873874 ) ) ;
#89796 = CARTESIAN_POINT ( 'NONE',  ( -6.250000000000019540, 12.50000000000000000, -7.122917578226816815 ) ) ;
#89797 = ADVANCED_FACE ( 'NONE', ( #51952 ), #110681, .T. ) ;
#89798 = DIRECTION ( 'NONE',  ( 0.000000000000000000, 0.000000000000000000, 1.000000000000000000 ) ) ;
#89799 = ORIENTED_EDGE ( 'NONE', *, *, #71905, .T. ) ;
#89800 = DIRECTION ( 'NONE',  ( 0.000000000000000000, 0.000000000000000000, 1.000000000000000000 ) ) ;
#89801 = VERTEX_POINT ( 'NONE', #13935 ) ;
#89803 = CIRCLE ( 'NONE', #68870, 0.06509327318403745899 ) ;
#89802 = FACE_OUTER_BOUND ( 'NONE', #59292, .T. ) ;
#89804 = DIRECTION ( 'NONE',  ( 0.000000000000000000, 0.000000000000000000, 1.000000000000000000 ) ) ;
#89805 = DIRECTION ( 'NONE',  ( 0.000000000000000000, 0.000000000000000000, 1.000000000000000000 ) ) ;
#89806 = VERTEX_POINT ( 'NONE', #34254 ) ;
#89807 = CARTESIAN_POINT ( 'NONE',  ( 105.0000000000000142, 8.500000000000000000, -0.2499999999999996392 ) ) ;
#89809 = AXIS2_PLACEMENT_3D ( 'NONE', #126201, #57469, #106552 ) ;
#89808 = VECTOR ( 'NONE', #24577, 1000.000000000000000 ) ;
#89810 = DIRECTION ( 'NONE',  ( 0.000000000000000000, -0.9999939076577903929, 0.003490651415223739937 ) ) ;
#89811 = VECTOR ( 'NONE', #36258, 1000.000000000000000 ) ;
#89812 = ORIENTED_EDGE ( 'NONE', *, *, #51808, .T. ) ;
#89813 = DIRECTION ( 'NONE',  ( -4.274815082592931898E-19, -0.9999939076577903929, -0.003490651415223739937 ) ) ;
#89814 = ORIENTED_EDGE ( 'NONE', *, *, #84258, .T. ) ;
#89815 = CARTESIAN_POINT ( 'NONE',  ( 13.54999999999989591, 2.500000000000000000, -1.818653347947326138 ) ) ;
#89817 = CONICAL_SURFACE ( 'NONE', #33413, 0.1000000000000002554, 0.003490658503988666988 ) ;
#89816 = AXIS2_PLACEMENT_3D ( 'NONE', #390, #92013, #99270 ) ;
#89818 = VERTEX_POINT ( 'NONE', #112153 ) ;
#89819 = DIRECTION ( 'NONE',  ( 0.000000000000000000, 1.000000000000000000, 0.000000000000000000 ) ) ;
#89820 = FACE_OUTER_BOUND ( 'NONE', #70609, .T. ) ;
#89821 = ORIENTED_EDGE ( 'NONE', *, *, #11878, .F. ) ;
#89822 = ORIENTED_EDGE ( 'NONE', *, *, #24041, .T. ) ;
#89823 = DIRECTION ( 'NONE',  ( 0.000000000000000000, 0.000000000000000000, 1.000000000000000000 ) ) ;
#89824 = DIRECTION ( 'NONE',  ( 0.000000000000000000, 1.000000000000000000, 0.000000000000000000 ) ) ;
#89825 = ORIENTED_EDGE ( 'NONE', *, *, #95835, .F. ) ;
#89826 = CARTESIAN_POINT ( 'NONE',  ( -0.4000000000000331624, 12.50000000000000000, -0.06509327318403743123 ) ) ;
#89827 = CARTESIAN_POINT ( 'NONE',  ( 12.09999999999990195, 12.50000000000000000, -0.6928203230275541413 ) ) ;
#89828 = ADVANCED_FACE ( 'NONE', ( #44053 ), #83963, .T. ) ;
#89829 = LINE ( 'NONE', #119287, #118457 ) ;
#89830 = CARTESIAN_POINT ( 'NONE',  ( 103.0416006710161554, 8.676147590107849084, -0.6650176703920132049 ) ) ;
#89831 = DIRECTION ( 'NONE',  ( 0.000000000000000000, -0.000000000000000000, 1.000000000000000000 ) ) ;
#89832 = LINE ( 'NONE', #111391, #82836 ) ;
#89833 = DIRECTION ( 'NONE',  ( 0.000000000000000000, 1.000000000000000000, 0.000000000000000000 ) ) ;
#89834 = AXIS2_PLACEMENT_3D ( 'NONE', #121336, #80791, #71597 ) ;
#89835 = VECTOR ( 'NONE', #76410, 1000.000000000000000 ) ;
#89836 = ORIENTED_EDGE ( 'NONE', *, *, #53226, .F. ) ;
#89837 = EDGE_LOOP ( 'NONE', ( #34634, #92974, #24540, #118389 ) ) ;
#89838 = ORIENTED_EDGE ( 'NONE', *, *, #93664, .T. ) ;
#89839 = DIRECTION ( 'NONE',  ( -4.274815082592931898E-19, -0.9999939076577903929, -0.003490651415223739937 ) ) ;
#89840 = CARTESIAN_POINT ( 'NONE',  ( 12.89999999999990088, 2.500000000000000000, 4.430127018922196847 ) ) ;
#89841 = DIRECTION ( 'NONE',  ( -0.000000000000000000, 1.000000000000000000, -0.000000000000000000 ) ) ;
#89842 = VERTEX_POINT ( 'NONE', #121975 ) ;
#89843 = FACE_BOUND ( 'NONE', #70853, .T. ) ;
#89844 = EDGE_LOOP ( 'NONE', ( #89658, #94473, #7795, #32703 ) ) ;
#89845 = CARTESIAN_POINT ( 'NONE',  ( 8.549999999999918998, 2.500000000000000000, -1.918653347947326004 ) ) ;
#89846 = CARTESIAN_POINT ( 'NONE',  ( 187.5000000000000000, -1.375000000000002442, -7.576237522675751457 ) ) ;
#89848 = AXIS2_PLACEMENT_3D ( 'NONE', #107434, #38055, #7285 ) ;
#89847 = CONICAL_SURFACE ( 'NONE', #5918, 0.09999999999999982514, 0.003490658503988666988 ) ;
#89849 = CARTESIAN_POINT ( 'NONE',  ( -3.469446951953614189E-14, 12.50000000000000000, -0.6277270498435144619 ) ) ;
#89850 = DIRECTION ( 'NONE',  ( -0.000000000000000000, 1.000000000000000000, -0.000000000000000000 ) ) ;
#89851 = CARTESIAN_POINT ( 'NONE',  ( -4.550000000000026468, 12.50000000000000000, -6.430097255199264339 ) ) ;
#89852 = LINE ( 'NONE', #9368, #45537 ) ;
#89853 = FACE_OUTER_BOUND ( 'NONE', #15649, .T. ) ;
#89854 = DIRECTION ( 'NONE',  ( 0.000000000000000000, 0.000000000000000000, 1.000000000000000000 ) ) ;
#89855 = AXIS2_PLACEMENT_3D ( 'NONE', #80661, #40086, #91756 ) ;
#89856 = FACE_OUTER_BOUND ( 'NONE', #43391, .T. ) ;
#89857 = VERTEX_POINT ( 'NONE', #92498 ) ;
#89858 = VERTEX_POINT ( 'NONE', #54504 ) ;
#89859 = AXIS2_PLACEMENT_3D ( 'NONE', #85132, #34773, #125066 ) ;
#89860 = ORIENTED_EDGE ( 'NONE', *, *, #60251, .T. ) ;
#89861 = VERTEX_POINT ( 'NONE', #91869 ) ;
#89862 = DIRECTION ( 'NONE',  ( 0.000000000000000000, -0.000000000000000000, 1.000000000000000000 ) ) ;
#89863 = DIRECTION ( 'NONE',  ( 0.000000000000000000, 0.000000000000000000, 1.000000000000000000 ) ) ;
#89864 = UNCERTAINTY_MEASURE_WITH_UNIT (LENGTH_MEASURE( 1.000000000000000082E-05 ), #26307, 'distance_accuracy_value', 'NONE');
#89866 = EDGE_LOOP ( 'NONE', ( #72980, #112761, #65235, #64662 ) ) ;
#89865 = ORIENTED_EDGE ( 'NONE', *, *, #93955, .T. ) ;
#89867 = CIRCLE ( 'NONE', #4169, 0.09999999999999999167 ) ;
#89868 = ORIENTED_EDGE ( 'NONE', *, *, #83785, .F. ) ;
#89869 = DIRECTION ( 'NONE',  ( 0.000000000000000000, 0.000000000000000000, 1.000000000000000000 ) ) ;
#89870 = CIRCLE ( 'NONE', #77360, 0.1000000000000002554 ) ;
#89871 = ADVANCED_FACE ( 'NONE', ( #62421 ), #116931, .T. ) ;
#89872 = DIRECTION ( 'NONE',  ( 0.000000000000000000, 1.000000000000000000, 0.000000000000000000 ) ) ;
#89873 = DIRECTION ( 'NONE',  ( -0.000000000000000000, -1.000000000000000000, -0.000000000000000000 ) ) ;
#89874 = CARTESIAN_POINT ( 'NONE',  ( 12.49999999999990052, 12.50000000000000000, 0.6928203230275494784 ) ) ;
#89875 = CARTESIAN_POINT ( 'NONE',  ( -12.49999999999995914, 2.500000000000000000, 1.843143693225357538E-15 ) ) ;
#89876 = CIRCLE ( 'NONE', #85751, 0.09999999999999982514 ) ;
#89877 = CARTESIAN_POINT ( 'NONE',  ( -3.950000000000028155, 12.50000000000000000, -6.841600689897077814 ) ) ;
#89878 = CARTESIAN_POINT ( 'NONE',  ( -5.850000000000021849, 12.50000000000000000, -5.802370205355749988 ) ) ;
#89879 = ADVANCED_FACE ( 'NONE', ( #67531 ), #52201, .T. ) ;
#89880 = ORIENTED_EDGE ( 'NONE', *, *, #105110, .F. ) ;
#89881 = ADVANCED_FACE ( 'NONE', ( #95738 ), #127422, .T. ) ;
#89882 = CARTESIAN_POINT ( 'NONE',  ( 0.8499999999999557909, 2.500000000000000000, -7.188010851410854052 ) ) ;
#89883 = ORIENTED_EDGE ( 'NONE', *, *, #110080, .T. ) ;
#89884 = ORIENTED_EDGE ( 'NONE', *, *, #63929, .T. ) ;
#89885 = VERTEX_POINT ( 'NONE', #45997 ) ;
#89886 = EDGE_CURVE ( 'NONE', #54425, #18483, #60540, .T. ) ;
#89888 = EDGE_CURVE ( 'NONE', #88688, #17050, #77381, .T. ) ;
#89887 = CARTESIAN_POINT ( 'NONE',  ( 108.0000000000000142, 8.500000000000000000, 0.2500000000000000000 ) ) ;
#89890 = ORIENTED_EDGE ( 'NONE', *, *, #106557, .F. ) ;
#89889 = ADVANCED_FACE ( 'NONE', ( #115341 ), #75186, .T. ) ;
#89891 = EDGE_CURVE ( 'NONE', #54633, #29223, #102294, .T. ) ;
#89893 = ORIENTED_EDGE ( 'NONE', *, *, #99731, .T. ) ;
#89892 = EDGE_CURVE ( 'NONE', #57396, #110257, #73036, .T. ) ;
#89894 = CARTESIAN_POINT ( 'NONE',  ( -3.950000000000024603, 12.50000000000000000, 1.753560074763284016 ) ) ;
#89895 = DIRECTION ( 'NONE',  ( 0.000000000000000000, 1.000000000000000000, 0.000000000000000000 ) ) ;
#89896 = DIRECTION ( 'NONE',  ( 0.000000000000000000, -0.000000000000000000, 1.000000000000000000 ) ) ;
#89897 = CARTESIAN_POINT ( 'NONE',  ( -0.6500000000000398792, 12.50000000000000000, -6.841600689897078702 ) ) ;
#89898 = CIRCLE ( 'NONE', #60591, 0.1000000000000002554 ) ;
#89899 = ADVANCED_FACE ( 'NONE', ( #85891 ), #36177, .T. ) ;
#89900 = ORIENTED_EDGE ( 'NONE', *, *, #110561, .F. ) ;
#89901 = DIRECTION ( 'NONE',  ( 0.000000000000000000, 0.000000000000000000, 1.000000000000000000 ) ) ;
#89902 = EDGE_CURVE ( 'NONE', #91091, #121671, #66261, .T. ) ;
#89903 = VERTEX_POINT ( 'NONE', #75431 ) ;
#89904 = DIRECTION ( 'NONE',  ( 0.000000000000000000, 1.000000000000000000, 0.000000000000000000 ) ) ;
#89905 = VECTOR ( 'NONE', #65823, 1000.000000000000000 ) ;
#89906 = EDGE_LOOP ( 'NONE', ( #51360, #83351 ) ) ;
#89907 = CARTESIAN_POINT ( 'NONE',  ( 5.649999999999936406, 2.500000000000000000, -6.841600689897077814 ) ) ;
#89908 = DIRECTION ( 'NONE',  ( 0.000000000000000000, 0.000000000000000000, 1.000000000000000000 ) ) ;
#89909 = ORIENTED_EDGE ( 'NONE', *, *, #53214, .T. ) ;
#89910 = CARTESIAN_POINT ( 'NONE',  ( -10.45000000000000107, 2.500000000000000000, 6.495190528383297135 ) ) ;
#89911 = DIRECTION ( 'NONE',  ( -4.274815082592931898E-19, -0.9999939076577903929, -0.003490651415223739937 ) ) ;
#89912 = ORIENTED_EDGE ( 'NONE', *, *, #41575, .T. ) ;
#89913 = VECTOR ( 'NONE', #125191, 1000.000000000000000 ) ;
#89914 = DIRECTION ( 'NONE',  ( 0.000000000000000000, 0.000000000000000000, 1.000000000000000000 ) ) ;
#89915 = VERTEX_POINT ( 'NONE', #104886 ) ;
#89916 = EDGE_LOOP ( 'NONE', ( #84171, #53204 ) ) ;
#89917 = DIRECTION ( 'NONE',  ( 0.000000000000000000, -0.9999939076577903929, 0.003490651415223739937 ) ) ;
#89918 = DIRECTION ( 'NONE',  ( -0.000000000000000000, -1.000000000000000000, -0.000000000000000000 ) ) ;
#89919 = CARTESIAN_POINT ( 'NONE',  ( 184.9218750003414016, 0.000000000000000000, 7.564683531250000925 ) ) ;
#89920 = CARTESIAN_POINT ( 'NONE',  ( 8.299999999999922551, 2.500000000000000000, 4.430127018922196847 ) ) ;
#89921 = FACE_OUTER_BOUND ( 'NONE', #91344, .T. ) ;
#89922 = ORIENTED_EDGE ( 'NONE', *, *, #70197, .F. ) ;
#89923 = DIRECTION ( 'NONE',  ( 0.000000000000000000, 0.000000000000000000, 1.000000000000000000 ) ) ;
#89924 = ADVANCED_FACE ( 'NONE', ( #125194 ), #31286, .T. ) ;
#89925 = ADVANCED_FACE ( 'NONE', ( #117268 ), #87693, .T. ) ;
#89926 = VERTEX_POINT ( 'NONE', #124556 ) ;
#89927 = FACE_OUTER_BOUND ( 'NONE', #50516, .T. ) ;
#89928 = AXIS2_PLACEMENT_3D ( 'NONE', #86991, #28732, #46416 ) ;
#89929 = CARTESIAN_POINT ( 'NONE',  ( -7.300000000000014921, 12.50000000000000000, 4.611443907251934426 ) ) ;
#89930 = CONICAL_SURFACE ( 'NONE', #23038, 0.1000000000000002554, 0.003490658503988666988 ) ;
#89931 = ADVANCED_FACE ( 'NONE', ( #27609 ), #14527, .T. ) ;
#89932 = CARTESIAN_POINT ( 'NONE',  ( 187.2552083336747444, 6.551208109652275624, -3.782341765624998686 ) ) ;
#89933 = FACE_OUTER_BOUND ( 'NONE', #85907, .T. ) ;
#89934 = DIRECTION ( 'NONE',  ( 0.000000000000000000, 1.000000000000000000, 0.000000000000000000 ) ) ;
#89935 = EDGE_CURVE ( 'NONE', #21947, #111738, #114718, .T. ) ;
#89936 = FACE_OUTER_BOUND ( 'NONE', #75591, .T. ) ;
#89937 = LINE ( 'NONE', #88656, #5659 ) ;
#89938 = ORIENTED_EDGE ( 'NONE', *, *, #109250, .F. ) ;
#89939 = CONICAL_SURFACE ( 'NONE', #25095, 0.1000000000000002554, 0.003490658503988666988 ) ;
#89940 = EDGE_CURVE ( 'NONE', #35226, #67849, #68829, .T. ) ;
#89941 = LINE ( 'NONE', #111521, #100313 ) ;
#89942 = EDGE_CURVE ( 'NONE', #118985, #97598, #91907, .T. ) ;
#89943 = DIRECTION ( 'NONE',  ( -0.000000000000000000, 1.000000000000000000, -0.000000000000000000 ) ) ;
#89944 = DIRECTION ( 'NONE',  ( 0.000000000000000000, 0.000000000000000000, 1.000000000000000000 ) ) ;
#89945 = CIRCLE ( 'NONE', #23061, 0.1000000000000000472 ) ;
#89946 = VERTEX_POINT ( 'NONE', #96353 ) ;
#89947 = EDGE_CURVE ( 'NONE', #52167, #47194, #89759, .T. ) ;
#89948 = CARTESIAN_POINT ( 'NONE',  ( 12.49999999999990585, 2.500000000000000000, -5.022947341949754119 ) ) ;
#89949 = CIRCLE ( 'NONE', #52394, 0.06509327318403745899 ) ;
#89950 = CONICAL_SURFACE ( 'NONE', #79503, 0.09999999999999982514, 0.003490658503988666988 ) ;
#89951 = VERTEX_POINT ( 'NONE', #34899 ) ;
#89952 = ORIENTED_EDGE ( 'NONE', *, *, #37051, .F. ) ;
#89953 = CARTESIAN_POINT ( 'NONE',  ( 9.799999999999913669, 2.500000000000000000, 4.576537180435972019 ) ) ;
#89954 = VERTEX_POINT ( 'NONE', #106819 ) ;
#89955 = FACE_OUTER_BOUND ( 'NONE', #71208, .T. ) ;
#89956 = CARTESIAN_POINT ( 'NONE',  ( 108.0000000000000142, 9.000000000000001776, 0.000000000000000000 ) ) ;
#89957 = CIRCLE ( 'NONE', #31482, 0.06509327318403745899 ) ;
#89958 = EDGE_LOOP ( 'NONE', ( #54549, #56632 ) ) ;
#89959 = CARTESIAN_POINT ( 'NONE',  ( -3.950000000000025491, 12.50000000000000000, 6.148780366869520897 ) ) ;
#89960 = DIRECTION ( 'NONE',  ( 0.000000000000000000, 0.000000000000000000, 1.000000000000000000 ) ) ;
#89961 = AXIS2_PLACEMENT_3D ( 'NONE', #46859, #15432, #56643 ) ;
#89962 = CARTESIAN_POINT ( 'NONE',  ( -8.150000000000014566, 2.500000000000000000, -6.841600689897073373 ) ) ;
#89963 = EDGE_CURVE ( 'NONE', #98405, #99586, #33354, .T. ) ;
#89964 = ORIENTED_EDGE ( 'NONE', *, *, #108413, .F. ) ;
#89965 = ORIENTED_EDGE ( 'NONE', *, *, #112518, .F. ) ;
#89966 = EDGE_LOOP ( 'NONE', ( #23527, #120133 ) ) ;
#89967 = FACE_OUTER_BOUND ( 'NONE', #110513, .T. ) ;
#89968 = FACE_OUTER_BOUND ( 'NONE', #21739, .T. ) ;
#89969 = DIRECTION ( 'NONE',  ( 0.000000000000000000, 0.000000000000000000, 1.000000000000000000 ) ) ;
#89970 = FACE_BOUND ( 'NONE', #109182, .T. ) ;
#89971 = ORIENTED_EDGE ( 'NONE', *, *, #112669, .T. ) ;
#89972 = DIRECTION ( 'NONE',  ( 0.000000000000000000, 0.000000000000000000, 1.000000000000000000 ) ) ;
#89973 = CARTESIAN_POINT ( 'NONE',  ( 9.999999999999911182, 12.50000000000000000, -3.572213422710612374 ) ) ;
#89974 = ORIENTED_EDGE ( 'NONE', *, *, #33960, .T. ) ;
#89975 = FACE_OUTER_BOUND ( 'NONE', #107912, .T. ) ;
#89976 = CARTESIAN_POINT ( 'NONE',  ( 8.949999999999917577, 2.500000000000000000, 6.048780366869520364 ) ) ;
#89977 = EDGE_CURVE ( 'NONE', #123416, #76721, #59033, .T. ) ;
#89979 = DIRECTION ( 'NONE',  ( 0.000000000000000000, 0.000000000000000000, 1.000000000000000000 ) ) ;
#89978 = CIRCLE ( 'NONE', #73262, 0.1000000000000002554 ) ;
#89980 = CARTESIAN_POINT ( 'NONE',  ( 11.44999999999990870, 2.500000000000000000, -1.718653347947326049 ) ) ;
#89981 = DIRECTION ( 'NONE',  ( 0.000000000000000000, 1.000000000000000000, 0.000000000000000000 ) ) ;
#89982 = CIRCLE ( 'NONE', #39926, 0.06509327318403745899 ) ;
#89983 = DIRECTION ( 'NONE',  ( 0.000000000000000000, 0.000000000000000000, 1.000000000000000000 ) ) ;
#89984 = CARTESIAN_POINT ( 'NONE',  ( 4.999999999999971578, 2.500000000000000000, -2.276824562219559311E-15 ) ) ;
#89985 = VECTOR ( 'NONE', #83975, 1000.000000000000000 ) ;
#89986 = EDGE_LOOP ( 'NONE', ( #51018, #63248 ) ) ;
#89987 = ORIENTED_EDGE ( 'NONE', *, *, #12305, .F. ) ;
#89988 = ORIENTED_EDGE ( 'NONE', *, *, #89004, .F. ) ;
#89989 = EDGE_LOOP ( 'NONE', ( #38878, #95275 ) ) ;
#89990 = DIRECTION ( 'NONE',  ( 0.000000000000000000, 0.000000000000000000, 1.000000000000000000 ) ) ;
#89991 = CARTESIAN_POINT ( 'NONE',  ( 2.499999999999981792, 12.50000000000000000, 4.265033745738159077 ) ) ;
#89992 = ORIENTED_EDGE ( 'NONE', *, *, #10568, .F. ) ;
#89993 = ADVANCED_FACE ( 'NONE', ( #30235 ), #93780, .T. ) ;
#89994 = FACE_BOUND ( 'NONE', #69599, .T. ) ;
#89995 = DIRECTION ( 'NONE',  ( 0.000000000000000000, 0.000000000000000000, -1.000000000000000000 ) ) ;
#89996 = CARTESIAN_POINT ( 'NONE',  ( 4.349999999999940137, 2.500000000000000000, -6.841600689897078702 ) ) ;
#89997 = DIRECTION ( 'NONE',  ( 0.000000000000000000, 0.000000000000000000, 1.000000000000000000 ) ) ;
#89998 = DIRECTION ( 'NONE',  ( 0.000000000000000000, 1.000000000000000000, 0.000000000000000000 ) ) ;
#89999 = CARTESIAN_POINT ( 'NONE',  ( 12.49999999999990585, 2.500000000000000000, 3.537306695894645081 ) ) ;
#90000 = CARTESIAN_POINT ( 'NONE',  ( 5.849999999999932143, 12.50000000000000000, 1.472243186433545459 ) ) ;
#90001 = VERTEX_POINT ( 'NONE', #28284 ) ;
#90002 = ORIENTED_EDGE ( 'NONE', *, *, #80771, .F. ) ;
#90003 = ORIENTED_EDGE ( 'NONE', *, *, #86034, .T. ) ;
#90004 = ORIENTED_EDGE ( 'NONE', *, *, #39696, .F. ) ;
#90005 = ORIENTED_EDGE ( 'NONE', *, *, #63914, .T. ) ;
#90006 = ORIENTED_EDGE ( 'NONE', *, *, #13330, .F. ) ;
#90007 = LINE ( 'NONE', #111599, #4562 ) ;
#90008 = PLANE ( 'NONE',  #67698 ) ;
#90009 = ORIENTED_EDGE ( 'NONE', *, *, #49759, .F. ) ;
#90010 = CARTESIAN_POINT ( 'NONE',  ( -9.350000000000004974, 2.500000000000000000, 6.841600689897072485 ) ) ;
#90011 = CIRCLE ( 'NONE', #4237, 0.1000000000000000472 ) ;
#90012 = ADVANCED_FACE ( 'NONE', ( #98293 ), #112562, .T. ) ;
#90013 = DIRECTION ( 'NONE',  ( 0.000000000000000000, 1.000000000000000000, 0.000000000000000000 ) ) ;
#90014 = CARTESIAN_POINT ( 'NONE',  ( 185.6927083336747160, 6.551208109652275624, -3.782341765624998686 ) ) ;
#90015 = DIRECTION ( 'NONE',  ( 0.000000000000000000, -0.9999939076577903929, 0.003490651415223739937 ) ) ;
#90016 = CARTESIAN_POINT ( 'NONE',  ( -13.09999999999999076, 2.500000000000000000, 3.983716857408420964 ) ) ;
#90017 = EDGE_LOOP ( 'NONE', ( #58231, #52263 ) ) ;
#90018 = FACE_OUTER_BOUND ( 'NONE', #67910, .T. ) ;
#90019 = AXIS2_PLACEMENT_3D ( 'NONE', #60041, #111700, #119568 ) ;
#90020 = EDGE_CURVE ( 'NONE', #49149, #101786, #18464, .T. ) ;
#90021 = VERTEX_POINT ( 'NONE', #48570 ) ;
#90022 = VERTEX_POINT ( 'NONE', #99607 ) ;
#90023 = FACE_OUTER_BOUND ( 'NONE', #31945, .T. ) ;
#90024 = ADVANCED_FACE ( 'NONE', ( #97 ), #35209, .T. ) ;
#90025 = DIRECTION ( 'NONE',  ( 0.000000000000000000, -0.000000000000000000, 1.000000000000000000 ) ) ;
#90027 = EDGE_CURVE ( 'NONE', #117051, #88674, #108339, .T. ) ;
#90026 = DIRECTION ( 'NONE',  ( 0.000000000000000000, 0.000000000000000000, -1.000000000000000000 ) ) ;
#90028 = ADVANCED_FACE ( 'NONE', ( #38104 ), #70776, .T. ) ;
#90029 = EDGE_CURVE ( 'NONE', #73591, #112590, #128438, .T. ) ;
#90030 = EDGE_LOOP ( 'NONE', ( #31862, #48264, #87838, #13478 ) ) ;
#90031 = ORIENTED_EDGE ( 'NONE', *, *, #106721, .T. ) ;
#90032 = AXIS2_PLACEMENT_3D ( 'NONE', #112499, #31367, #90919 ) ;
#90033 = CARTESIAN_POINT ( 'NONE',  ( 4.999999999999938716, 2.500000000000000000, -5.022947341949754119 ) ) ;
#90034 = AXIS2_PLACEMENT_3D ( 'NONE', #37184, #18807, #87546 ) ;
#90036 = EDGE_CURVE ( 'NONE', #86174, #113061, #10151, .T. ) ;
#90035 = CARTESIAN_POINT ( 'NONE',  ( 4.349999999999937472, 2.500000000000000000, 6.841600689897072485 ) ) ;
#90037 = CARTESIAN_POINT ( 'NONE',  ( -2.100000000000033840, 2.500000000000000000, 3.537306695894645081 ) ) ;
#90038 = ADVANCED_FACE ( 'NONE', ( #19757 ), #89570, .T. ) ;
#90039 = CARTESIAN_POINT ( 'NONE',  ( -10.00000000000000355, 12.50000000000000000, 3.637306695894644726 ) ) ;
#90040 = EDGE_LOOP ( 'NONE', ( #85248, #87145, #55682, #126605 ) ) ;
#90041 = FACE_OUTER_BOUND ( 'NONE', #34573, .T. ) ;
#90042 = EDGE_CURVE ( 'NONE', #92801, #101017, #69478, .T. ) ;
#90043 = CONICAL_SURFACE ( 'NONE', #92103, 0.1000000000000002554, 0.003490658503988666988 ) ;
#90044 = VERTEX_POINT ( 'NONE', #109412 ) ;
#90045 = DIRECTION ( 'NONE',  ( 0.000000000000000000, -0.9999939076577903929, 0.003490651415223739937 ) ) ;
#90046 = EDGE_CURVE ( 'NONE', #19500, #15955, #89771, .T. ) ;
#90047 = EDGE_CURVE ( 'NONE', #110619, #49354, #78017, .T. ) ;
#90048 = ORIENTED_EDGE ( 'NONE', *, *, #82460, .T. ) ;
#90049 = DIRECTION ( 'NONE',  ( 0.000000000000000000, 0.000000000000000000, 1.000000000000000000 ) ) ;
#90050 = DIRECTION ( 'NONE',  ( 0.000000000000000000, 0.000000000000000000, 1.000000000000000000 ) ) ;
#90051 = AXIS2_PLACEMENT_3D ( 'NONE', #10756, #8841, #79538 ) ;
#90052 = DIRECTION ( 'NONE',  ( 0.000000000000000000, 0.000000000000000000, 1.000000000000000000 ) ) ;
#90054 = EDGE_CURVE ( 'NONE', #61247, #30638, #43615, .T. ) ;
#90053 = DIRECTION ( 'NONE',  ( 0.000000000000000000, -0.9999939076577903929, 0.003490651415223739937 ) ) ;
#90055 = EDGE_LOOP ( 'NONE', ( #80052, #11797, #17178, #75835 ) ) ;
#90056 = CARTESIAN_POINT ( 'NONE',  ( 2.699999999999947331, 2.500000000000000000, -0.4464101615137783252 ) ) ;
#90057 = DIRECTION ( 'NONE',  ( -0.000000000000000000, 1.000000000000000000, -0.000000000000000000 ) ) ;
#90058 = EDGE_LOOP ( 'NONE', ( #31794, #57223, #42922, #44690 ) ) ;
#90059 = ORIENTED_EDGE ( 'NONE', *, *, #109915, .F. ) ;
#90060 = ORIENTED_EDGE ( 'NONE', *, *, #39277, .T. ) ;
#90061 = CARTESIAN_POINT ( 'NONE',  ( -11.84999999999999787, 2.500000000000000000, -6.248780366869523206 ) ) ;
#90062 = LINE ( 'NONE', #120829, #76260 ) ;
#90063 = CARTESIAN_POINT ( 'NONE',  ( -10.65000000000000213, 2.500000000000000000, 1.818653347947321475 ) ) ;
#90064 = FACE_OUTER_BOUND ( 'NONE', #97727, .T. ) ;
#90065 = CARTESIAN_POINT ( 'NONE',  ( 6.449999999999930012, 2.500000000000000000, -1.718653347947326049 ) ) ;
#90066 = CARTESIAN_POINT ( 'NONE',  ( -6.249999999999984901, 2.500000000000000000, -2.165063509461101710 ) ) ;
#90067 = DIRECTION ( 'NONE',  ( 0.000000000000000000, 0.000000000000000000, -1.000000000000000000 ) ) ;
#90068 = DIRECTION ( 'NONE',  ( 0.000000000000000000, -0.9999939076577903929, 0.003490651415223739937 ) ) ;
#90069 = CARTESIAN_POINT ( 'NONE',  ( -0.2000000000000339284, 12.50000000000000000, -0.3464101615137759604 ) ) ;
#90070 = AXIS2_PLACEMENT_3D ( 'NONE', #25171, #65084, #105015 ) ;
#90071 = AXIS2_PLACEMENT_3D ( 'NONE', #105538, #55150, #103609 ) ;
#90072 = VECTOR ( 'NONE', #41623, 1000.000000000000000 ) ;
#90073 = CIRCLE ( 'NONE', #94200, 0.1000000000000002554 ) ;
#90074 = VERTEX_POINT ( 'NONE', #40703 ) ;
#90075 = CARTESIAN_POINT ( 'NONE',  ( -0.4500000000000402012, 2.500000000000000000, 6.395190528383296602 ) ) ;
#90076 = AXIS2_PLACEMENT_3D ( 'NONE', #57366, #13406, #61235 ) ;
#90077 = FACE_OUTER_BOUND ( 'NONE', #49834, .T. ) ;
#90078 = CARTESIAN_POINT ( 'NONE',  ( -4.800000000000022915, 12.50000000000000000, -0.2813168883297409439 ) ) ;
#90079 = DIRECTION ( 'NONE',  ( 0.000000000000000000, 0.000000000000000000, 1.000000000000000000 ) ) ;
#90080 = FACE_OUTER_BOUND ( 'NONE', #43094, .T. ) ;
#90081 = VERTEX_POINT ( 'NONE', #21030 ) ;
#90082 = DIRECTION ( 'NONE',  ( -0.000000000000000000, 1.000000000000000000, -0.000000000000000000 ) ) ;
#90083 = EDGE_CURVE ( 'NONE', #127944, #64309, #114596, .T. ) ;
#90084 = ADVANCED_FACE ( 'NONE', ( #90399 ), #11200, .T. ) ;
#90085 = CARTESIAN_POINT ( 'NONE',  ( 7.899999999999923084, 2.500000000000000000, 0.7928203230275495672 ) ) ;
#90087 = ORIENTED_EDGE ( 'NONE', *, *, #57908, .F. ) ;
#90086 = DIRECTION ( 'NONE',  ( -0.000000000000000000, -1.000000000000000000, -0.000000000000000000 ) ) ;
#90088 = ORIENTED_EDGE ( 'NONE', *, *, #63067, .T. ) ;
#90089 = EDGE_CURVE ( 'NONE', #114467, #64833, #56106, .T. ) ;
#90090 = CARTESIAN_POINT ( 'NONE',  ( -1.450000000000036371, 12.50000000000000000, 2.511473670974873507 ) ) ;
#90091 = TOROIDAL_SURFACE ( 'NONE', #71317, 9.000000000000001776, 1.000000000000000000 ) ;
#90092 = ORIENTED_EDGE ( 'NONE', *, *, #53995, .F. ) ;
#90093 = ORIENTED_EDGE ( 'NONE', *, *, #90940, .T. ) ;
#90094 = DIRECTION ( 'NONE',  ( 0.000000000000000000, 0.000000000000000000, -1.000000000000000000 ) ) ;
#90095 = CARTESIAN_POINT ( 'NONE',  ( 18.93069778776544609, 2.571126379696650144, -2.451182541063273490 ) ) ;
#90096 = CARTESIAN_POINT ( 'NONE',  ( -4.800000000000026468, 12.50000000000000000, -4.676537180435978769 ) ) ;
#90097 = FACE_OUTER_BOUND ( 'NONE', #49095, .T. ) ;
#90098 = AXIS2_PLACEMENT_3D ( 'NONE', #128261, #57585, #76570 ) ;
#90099 = ORIENTED_EDGE ( 'NONE', *, *, #35411, .T. ) ;
#90100 = AXIS2_PLACEMENT_3D ( 'NONE', #110969, #80898, #48869 ) ;
#90101 = DIRECTION ( 'NONE',  ( 0.000000000000000000, -0.000000000000000000, 1.000000000000000000 ) ) ;
#90102 = ORIENTED_EDGE ( 'NONE', *, *, #12413, .T. ) ;
#90103 = DIRECTION ( 'NONE',  ( -0.000000000000000000, 1.000000000000000000, -0.000000000000000000 ) ) ;
#90104 = CARTESIAN_POINT ( 'NONE',  ( -0.4000000000000339950, 12.50000000000000000, 0.6277270498435143509 ) ) ;
#90105 = DIRECTION ( 'NONE',  ( -0.000000000000000000, -1.000000000000000000, -0.000000000000000000 ) ) ;
#90106 = AXIS2_PLACEMENT_3D ( 'NONE', #89897, #10671, #11981 ) ;
#90107 = EDGE_LOOP ( 'NONE', ( #105001, #53281, #95330, #121211 ) ) ;
#90108 = AXIS2_PLACEMENT_3D ( 'NONE', #31475, #72690, #112616 ) ;
#90109 = ORIENTED_EDGE ( 'NONE', *, *, #99350, .T. ) ;
#90110 = ORIENTED_EDGE ( 'NONE', *, *, #90831, .T. ) ;
#90111 = ORIENTED_EDGE ( 'NONE', *, *, #64807, .T. ) ;
#90112 = ORIENTED_EDGE ( 'NONE', *, *, #78593, .T. ) ;
#90113 = CARTESIAN_POINT ( 'NONE',  ( 0.8499999999999527933, 2.500000000000000000, 7.088010851410848190 ) ) ;
#90114 = CARTESIAN_POINT ( 'NONE',  ( 15.50668944026764962, 2.500000000000127010, 6.997696164093728299 ) ) ;
#90115 = CARTESIAN_POINT ( 'NONE',  ( 12.94999999999989981, 2.500000000000000000, -2.065063509461102065 ) ) ;
#90116 = FACE_BOUND ( 'NONE', #81974, .T. ) ;
#90117 = CARTESIAN_POINT ( 'NONE',  ( -8.150000000000012790, 12.50000000000000000, -2.446380397790840266 ) ) ;
#90118 = CARTESIAN_POINT ( 'NONE',  ( 186.2812500006828031, 0.000000000000000000, 7.700000000000000178 ) ) ;
#90119 = CARTESIAN_POINT ( 'NONE',  ( 12.29999999999990479, 12.50000000000000000, 4.676537180435972552 ) ) ;
#90120 = CARTESIAN_POINT ( 'NONE',  ( -2.950000000000033484, 12.50000000000000000, -6.495190528383302464 ) ) ;
#90121 = AXIS2_PLACEMENT_3D ( 'NONE', #125524, #105243, #124251 ) ;
#90122 = CONICAL_SURFACE ( 'NONE', #2380, 0.09999999999999982514, 0.003490658503988666988 ) ;
#90123 = DIRECTION ( 'NONE',  ( 0.000000000000000000, 1.000000000000000000, 0.000000000000000000 ) ) ;
#90124 = FACE_OUTER_BOUND ( 'NONE', #105611, .T. ) ;
#90125 = LINE ( 'NONE', #77730, #126466 ) ;
#90126 = CIRCLE ( 'NONE', #94337, 0.06509327318403745899 ) ;
#90127 = DIRECTION ( 'NONE',  ( 0.000000000000000000, 0.000000000000000000, 1.000000000000000000 ) ) ;
#90128 = ORIENTED_EDGE ( 'NONE', *, *, #29388, .T. ) ;
#90129 = CONICAL_SURFACE ( 'NONE', #50351, 0.09999999999999982514, 0.003490658503988666988 ) ;
#90130 = CIRCLE ( 'NONE', #39999, 0.09999999999999999167 ) ;
#90131 = EDGE_LOOP ( 'NONE', ( #11338, #18577, #113282, #12854 ) ) ;
#90132 = ORIENTED_EDGE ( 'NONE', *, *, #51155, .T. ) ;
#90133 = ORIENTED_EDGE ( 'NONE', *, *, #67126, .F. ) ;
#90134 = EDGE_CURVE ( 'NONE', #3310, #24288, #45668, .T. ) ;
#90135 = CARTESIAN_POINT ( 'NONE',  ( 8.349999999999919709, 12.50000000000000000, -2.922977105672691422 ) ) ;
#90136 = DIRECTION ( 'NONE',  ( 0.000000000000000000, 1.000000000000000000, 0.000000000000000000 ) ) ;
#90137 = EDGE_CURVE ( 'NONE', #86700, #108664, #6207, .T. ) ;
#90138 = FACE_BOUND ( 'NONE', #89906, .T. ) ;
#90139 = DIRECTION ( 'NONE',  ( -4.274815082592931898E-19, -0.9999939076577903929, -0.003490651415223739937 ) ) ;
#90140 = ORIENTED_EDGE ( 'NONE', *, *, #71847, .T. ) ;
#90141 = DIRECTION ( 'NONE',  ( -4.274815082592931898E-19, -0.9999939076577903929, -0.003490651415223739937 ) ) ;
#90142 = CARTESIAN_POINT ( 'NONE',  ( 14.14999999999989200, 2.500000000000000000, -2.165063509461101710 ) ) ;
#90143 = EDGE_CURVE ( 'NONE', #10563, #62105, #1726, .T. ) ;
#90144 = DIRECTION ( 'NONE',  ( -0.000000000000000000, 1.000000000000000000, -0.000000000000000000 ) ) ;
#90145 = CARTESIAN_POINT ( 'NONE',  ( -2.100000000000033396, 12.50000000000000000, -5.088040615133791356 ) ) ;
#90146 = ORIENTED_EDGE ( 'NONE', *, *, #73747, .T. ) ;
#90147 = FACE_OUTER_BOUND ( 'NONE', #33035, .T. ) ;
#90148 = EDGE_LOOP ( 'NONE', ( #127599, #57978 ) ) ;
#90149 = ORIENTED_EDGE ( 'NONE', *, *, #91538, .T. ) ;
#90150 = VECTOR ( 'NONE', #66883, 1000.000000000000000 ) ;
#90151 = CARTESIAN_POINT ( 'NONE',  ( -5.600000000000023626, 12.50000000000000000, -4.676537180435977881 ) ) ;
#90152 = CARTESIAN_POINT ( 'NONE',  ( 108.0000000000000142, 8.500000000000000000, 0.000000000000000000 ) ) ;
#90153 = ORIENTED_EDGE ( 'NONE', *, *, #45037, .F. ) ;
#90154 = DIRECTION ( 'NONE',  ( 0.000000000000000000, 0.000000000000000000, 1.000000000000000000 ) ) ;
#90155 = AXIS2_PLACEMENT_3D ( 'NONE', #92353, #114569, #107981 ) ;
#90158 = ADVANCED_FACE ( 'NONE', ( #92338 ), #129305, .T. ) ;
#90157 = AXIS2_PLACEMENT_3D ( 'NONE', #5016, #44971, #84877 ) ;
#90156 = CARTESIAN_POINT ( 'NONE',  ( 8.949999999999919353, 12.50000000000000000, -6.148780366869526226 ) ) ;
#90159 = DIRECTION ( 'NONE',  ( 0.000000000000000000, 0.000000000000000000, -1.000000000000000000 ) ) ;
#90160 = VERTEX_POINT ( 'NONE', #62894 ) ;
#90161 = AXIS2_PLACEMENT_3D ( 'NONE', #118057, #126607, #36934 ) ;
#90162 = DIRECTION ( 'NONE',  ( 0.000000000000000000, 1.000000000000000000, 0.000000000000000000 ) ) ;
#90163 = VERTEX_POINT ( 'NONE', #121166 ) ;
#90164 = DIRECTION ( 'NONE',  ( -0.000000000000000000, -1.000000000000000000, -0.000000000000000000 ) ) ;
#90165 = EDGE_CURVE ( 'NONE', #93275, #122496, #60344, .T. ) ;
#90166 = ORIENTED_EDGE ( 'NONE', *, *, #66849, .T. ) ;
#90167 = CARTESIAN_POINT ( 'NONE',  ( 111.3003809011547105, 6.719038074301505681, -3.769326045731886232 ) ) ;
#90168 = ORIENTED_EDGE ( 'NONE', *, *, #24921, .F. ) ;
#90169 = DIRECTION ( 'NONE',  ( -0.000000000000000000, -1.000000000000000000, -0.000000000000000000 ) ) ;
#90170 = DIRECTION ( 'NONE',  ( 0.000000000000000000, 1.000000000000000000, 0.000000000000000000 ) ) ;
#90171 = EDGE_CURVE ( 'NONE', #66106, #79633, #106294, .T. ) ;
#90172 = CARTESIAN_POINT ( 'NONE',  ( 1.449999999999951328, 12.50000000000000000, 2.576566944158910744 ) ) ;
#90174 = EDGE_CURVE ( 'NONE', #57536, #67817, #95834, .T. ) ;
#90173 = FACE_OUTER_BOUND ( 'NONE', #122726, .T. ) ;
#90175 = ADVANCED_FACE ( 'NONE', ( #93645 ), #83325, .T. ) ;
#90176 = CARTESIAN_POINT ( 'NONE',  ( 3.549999999999943867, 12.50000000000000000, -6.083687093685488989 ) ) ;
#90177 = EDGE_CURVE ( 'NONE', #56615, #118548, #3878, .T. ) ;
#90178 = EDGE_LOOP ( 'NONE', ( #38981, #43881, #33461, #28649 ) ) ;
#90179 = VERTEX_POINT ( 'NONE', #41970 ) ;
#90180 = ORIENTED_EDGE ( 'NONE', *, *, #120813, .F. ) ;
#90181 = CARTESIAN_POINT ( 'NONE',  ( -0.8500000000000390576, 12.50000000000000000, -2.165063509461101710 ) ) ;
#90182 = LINE ( 'NONE', #40486, #43149 ) ;
#90183 = ADVANCED_FACE ( 'NONE', ( #64175 ), #26874, .T. ) ;
#90184 = LINE ( 'NONE', #98090, #35539 ) ;
#90186 = ORIENTED_EDGE ( 'NONE', *, *, #28265, .F. ) ;
#90185 = VERTEX_POINT ( 'NONE', #3962 ) ;
#90187 = ORIENTED_EDGE ( 'NONE', *, *, #30716, .F. ) ;
#90188 = EDGE_CURVE ( 'NONE', #125479, #19146, #68919, .T. ) ;
#90189 = CARTESIAN_POINT ( 'NONE',  ( 4.149999999999938183, 12.50000000000000000, 5.867463478539781896 ) ) ;
#90191 = EDGE_LOOP ( 'NONE', ( #29189, #94212, #17120, #21767 ) ) ;
#90190 = AXIS2_PLACEMENT_3D ( 'NONE', #118261, #66580, #6349 ) ;
#90192 = CARTESIAN_POINT ( 'NONE',  ( 4.399999999999939071, 2.500000000000000000, 0.2464101615137736789 ) ) ;
#90193 = AXIS2_PLACEMENT_3D ( 'NONE', #28420, #58533, #98421 ) ;
#90194 = EDGE_CURVE ( 'NONE', #47712, #13125, #77051, .T. ) ;
#90195 = CARTESIAN_POINT ( 'NONE',  ( -3.950000000000026379, 2.500000000000000000, 2.511473670974873507 ) ) ;
#90196 = LINE ( 'NONE', #40501, #102462 ) ;
#90197 = DIRECTION ( 'NONE',  ( -4.274815082592931898E-19, -0.9999939076577903929, -0.003490651415223739937 ) ) ;
#90198 = CARTESIAN_POINT ( 'NONE',  ( -7.900000000000014566, 2.500000000000000000, 0.09999999999999772959 ) ) ;
#90199 = DIRECTION ( 'NONE',  ( 0.000000000000000000, 0.000000000000000000, 1.000000000000000000 ) ) ;
#90200 = EDGE_CURVE ( 'NONE', #30524, #20308, #97875, .T. ) ;
#90203 = ADVANCED_FACE ( 'NONE', ( #81869 ), #12482, .T. ) ;
#90202 = AXIS2_PLACEMENT_3D ( 'NONE', #92875, #32683, #12359 ) ;
#90201 = PLANE ( 'NONE',  #102202 ) ;
#90204 = VERTEX_POINT ( 'NONE', #74002 ) ;
#90205 = ORIENTED_EDGE ( 'NONE', *, *, #106943, .T. ) ;
#90206 = DIRECTION ( 'NONE',  ( 0.000000000000000000, 0.000000000000000000, -1.000000000000000000 ) ) ;
#90207 = AXIS2_PLACEMENT_3D ( 'NONE', #17467, #67866, #107801 ) ;
#90208 = DIRECTION ( 'NONE',  ( 0.000000000000000000, 1.000000000000000000, 0.000000000000000000 ) ) ;
#90209 = ORIENTED_EDGE ( 'NONE', *, *, #47915, .T. ) ;
#90210 = VERTEX_POINT ( 'NONE', #83189 ) ;
#90211 = CARTESIAN_POINT ( 'NONE',  ( 186.0677083336747444, -4.367472073101514418, -7.564683531250002702 ) ) ;
#90212 = CARTESIAN_POINT ( 'NONE',  ( 7.299999999999926104, 12.50000000000000000, -0.3464101615137782364 ) ) ;
#90213 = DIRECTION ( 'NONE',  ( 0.000000000000000000, 0.000000000000000000, -1.000000000000000000 ) ) ;
#90214 = AXIS2_PLACEMENT_3D ( 'NONE', #85445, #36373, #76278 ) ;
#90215 = DIRECTION ( 'NONE',  ( -0.000000000000000000, 1.000000000000000000, -0.000000000000000000 ) ) ;
#90216 =( GEOMETRIC_REPRESENTATION_CONTEXT ( 3 ) GLOBAL_UNCERTAINTY_ASSIGNED_CONTEXT ( ( #55809 ) ) GLOBAL_UNIT_ASSIGNED_CONTEXT ( ( #54949, #6459, #28078 ) ) REPRESENTATION_CONTEXT ( 'NONE', 'WORKASPACE' ) );
#90217 = AXIS2_PLACEMENT_3D ( 'NONE', #76139, #18501, #28985 ) ;
#90218 = FACE_OUTER_BOUND ( 'NONE', #6684, .T. ) ;
#90219 = FACE_OUTER_BOUND ( 'NONE', #74359, .T. ) ;
#90220 = AXIS2_PLACEMENT_3D ( 'NONE', #18777, #48908, #88812 ) ;
#90221 = DIRECTION ( 'NONE',  ( 0.000000000000000000, 1.000000000000000000, 0.000000000000000000 ) ) ;
#90222 = AXIS2_PLACEMENT_3D ( 'NONE', #52626, #12057, #2895 ) ;
#90223 = CARTESIAN_POINT ( 'NONE',  ( 4.599999999999938360, 2.500000000000000000, -0.1000000000000022815 ) ) ;
#90224 = ORIENTED_EDGE ( 'NONE', *, *, #6556, .T. ) ;
#90225 = ORIENTED_EDGE ( 'NONE', *, *, #118392, .T. ) ;
#90226 = VECTOR ( 'NONE', #38164, 1000.000000000000000 ) ;
#90227 = AXIS2_PLACEMENT_3D ( 'NONE', #99257, #29229, #100519 ) ;
#90228 = ORIENTED_EDGE ( 'NONE', *, *, #99090, .T. ) ;
#90229 = ORIENTED_EDGE ( 'NONE', *, *, #108089, .T. ) ;
#90230 = ORIENTED_EDGE ( 'NONE', *, *, #1976, .T. ) ;
#90231 = DIRECTION ( 'NONE',  ( 0.000000000000000000, 1.000000000000000000, 0.000000000000000000 ) ) ;
#90232 = DIRECTION ( 'NONE',  ( 0.000000000000000000, 1.000000000000000000, 0.000000000000000000 ) ) ;
#90233 = EDGE_LOOP ( 'NONE', ( #59841, #55484 ) ) ;
#90234 = LINE ( 'NONE', #88301, #100906 ) ;
#90235 = EDGE_CURVE ( 'NONE', #68041, #91784, #41480, .T. ) ;
#90236 = CARTESIAN_POINT ( 'NONE',  ( 10.64999999999990976, 2.500000000000000000, -6.941600689897077459 ) ) ;
#90237 = EDGE_CURVE ( 'NONE', #129597, #116188, #36816, .T. ) ;
#90238 = DIRECTION ( 'NONE',  ( 0.000000000000000000, 1.000000000000000000, 0.000000000000000000 ) ) ;
#90240 = ORIENTED_EDGE ( 'NONE', *, *, #86029, .F. ) ;
#90239 = DIRECTION ( 'NONE',  ( -0.000000000000000000, -1.000000000000000000, -0.000000000000000000 ) ) ;
#90241 = LINE ( 'NONE', #121646, #74632 ) ;
#90242 = CARTESIAN_POINT ( 'NONE',  ( 8.749999999999920064, 12.50000000000000000, 5.737276932171707422 ) ) ;
#90243 = ORIENTED_EDGE ( 'NONE', *, *, #23726, .F. ) ;
#90244 = ORIENTED_EDGE ( 'NONE', *, *, #114298, .T. ) ;
#90245 = EDGE_LOOP ( 'NONE', ( #122247, #45201, #14806, #53968 ) ) ;
#90246 = AXIS2_PLACEMENT_3D ( 'NONE', #79206, #96887, #98822 ) ;
#90247 = ORIENTED_EDGE ( 'NONE', *, *, #74581, .T. ) ;
#90248 = DIRECTION ( 'NONE',  ( 0.000000000000000000, 1.000000000000000000, 0.000000000000000000 ) ) ;
#90249 = VECTOR ( 'NONE', #100542, 1000.000000000000000 ) ;
#90250 = CARTESIAN_POINT ( 'NONE',  ( -7.950000000000012612, 12.50000000000000000, 2.230156782645134950 ) ) ;
#90251 = DIRECTION ( 'NONE',  ( 0.000000000000000000, 1.000000000000000000, 0.000000000000000000 ) ) ;
#90252 = AXIS2_PLACEMENT_3D ( 'NONE', #14284, #32027, #52940 ) ;
#90253 = CIRCLE ( 'NONE', #104922, 0.06509327318403745899 ) ;
#90254 = DIRECTION ( 'NONE',  ( 0.000000000000000000, 0.000000000000000000, -1.000000000000000000 ) ) ;
#90256 = ORIENTED_EDGE ( 'NONE', *, *, #33951, .T. ) ;
#90255 = VECTOR ( 'NONE', #33063, 1000.000000000000000 ) ;
#90257 = FACE_OUTER_BOUND ( 'NONE', #9786, .T. ) ;
#90258 = DIRECTION ( 'NONE',  ( -0.000000000000000000, 1.000000000000000000, -0.000000000000000000 ) ) ;
#90259 = CIRCLE ( 'NONE', #84005, 0.1000000000000000472 ) ;
#90260 = DIRECTION ( 'NONE',  ( -0.000000000000000000, 1.000000000000000000, -0.000000000000000000 ) ) ;
#90261 = CARTESIAN_POINT ( 'NONE',  ( 1.249999999999988454, 2.500000000000000000, 2.165063509461097713 ) ) ;
#90262 = CIRCLE ( 'NONE', #106992, 0.06509327318403745899 ) ;
#90263 = VERTEX_POINT ( 'NONE', #124398 ) ;
#90264 = DIRECTION ( 'NONE',  ( -4.274815082592931898E-19, -0.9999939076577903929, -0.003490651415223739937 ) ) ;
#90265 = ORIENTED_EDGE ( 'NONE', *, *, #72595, .F. ) ;
#90266 = ORIENTED_EDGE ( 'NONE', *, *, #125597, .T. ) ;
#90267 = DIRECTION ( 'NONE',  ( -0.000000000000000000, -1.000000000000000000, -0.000000000000000000 ) ) ;
#90268 = CARTESIAN_POINT ( 'NONE',  ( 9.149999999999915090, 12.50000000000000000, 6.495190528383297135 ) ) ;
#90269 = FACE_BOUND ( 'NONE', #110156, .T. ) ;
#90270 = FACE_OUTER_BOUND ( 'NONE', #123865, .T. ) ;
#90271 = CARTESIAN_POINT ( 'NONE',  ( 3.949999999999942446, 2.500000000000000000, -6.841600689897078702 ) ) ;
#90272 = CARTESIAN_POINT ( 'NONE',  ( -2.900000000000030109, 12.50000000000000000, -3.637306695894650055 ) ) ;
#90273 = EDGE_CURVE ( 'NONE', #29184, #43211, #76582, .T. ) ;
#90274 = FACE_OUTER_BOUND ( 'NONE', #52408, .T. ) ;
#90275 = FACE_OUTER_BOUND ( 'NONE', #103173, .T. ) ;
#90276 = CARTESIAN_POINT ( 'NONE',  ( 5.599999999999931255, 2.500000000000000000, 4.083716857408420609 ) ) ;
#90277 = CARTESIAN_POINT ( 'NONE',  ( -6.650000000000018119, 2.500000000000000000, -2.065063509461102065 ) ) ;
#90278 = VERTEX_POINT ( 'NONE', #56281 ) ;
#90279 = VECTOR ( 'NONE', #21350, 1000.000000000000000 ) ;
#90280 = DIRECTION ( 'NONE',  ( 0.000000000000000000, -0.000000000000000000, 1.000000000000000000 ) ) ;
#90281 = AXIS2_PLACEMENT_3D ( 'NONE', #48548, #49211, #117916 ) ;
#90282 = PLANE ( 'NONE',  #3639 ) ;
#90283 = ORIENTED_EDGE ( 'NONE', *, *, #82078, .T. ) ;
#90284 = ORIENTED_EDGE ( 'NONE', *, *, #84585, .T. ) ;
#90285 = EDGE_CURVE ( 'NONE', #116013, #109874, #26193, .T. ) ;
#90286 = DIRECTION ( 'NONE',  ( 0.000000000000000000, -0.000000000000000000, 1.000000000000000000 ) ) ;
#90288 = ADVANCED_FACE ( 'NONE', ( #105395 ), #10243, .T. ) ;
#90287 = CARTESIAN_POINT ( 'NONE',  ( 9.149999999999920419, 12.50000000000000000, 2.792790559304612064 ) ) ;
#90289 = FACE_BOUND ( 'NONE', #76217, .T. ) ;
#90290 = AXIS2_PLACEMENT_3D ( 'NONE', #35245, #46994, #86898 ) ;
#90291 = CARTESIAN_POINT ( 'NONE',  ( 6.449999999999930012, 12.50000000000000000, -1.818653347947326138 ) ) ;
#90292 = CONICAL_SURFACE ( 'NONE', #65152, 0.09999999999999999167, 0.003490658503988666988 ) ;
#90293 = AXIS2_PLACEMENT_3D ( 'NONE', #108107, #50479, #110051 ) ;
#90295 = FACE_OUTER_BOUND ( 'NONE', #24831, .T. ) ;
#90294 = AXIS2_PLACEMENT_3D ( 'NONE', #16508, #36184, #76740 ) ;
#90296 =( BOUNDED_CURVE ( )  B_SPLINE_CURVE ( 2, ( #58553, #38933, #119381, #39577, #79484, #27777, #78847 ),
 .UNSPECIFIED., .F., .F. ) 
 B_SPLINE_CURVE_WITH_KNOTS ( ( 3, 2, 2, 3 ),
 ( 0.8571428571428578724, 0.8809523809523817084, 0.9047619047619054333, 0.9285714285714292693 ),
 .UNSPECIFIED. ) 
 CURVE ( )  GEOMETRIC_REPRESENTATION_ITEM ( )  RATIONAL_B_SPLINE_CURVE ( ( 0.9999999999999956701, 0.8660254037844430375, 1.000000000000000000, 0.8660254037844387076, 1.000000000000000000, 0.8660254037844349329, 1.000000000000003775 ) ) 
 REPRESENTATION_ITEM ( '' )  );
#90297 = EDGE_LOOP ( 'NONE', ( #120847, #72205 ) ) ;
#90298 = FACE_OUTER_BOUND ( 'NONE', #12705, .T. ) ;
#90299 = EDGE_CURVE ( 'NONE', #105300, #5812, #62488, .T. ) ;
#90300 = DIRECTION ( 'NONE',  ( -0.000000000000000000, 1.000000000000000000, -0.000000000000000000 ) ) ;
#90301 = EDGE_LOOP ( 'NONE', ( #2661, #102463, #32885, #82076 ) ) ;
#90303 = CARTESIAN_POINT ( 'NONE',  ( 5.799999999999933209, 12.50000000000000000, -2.385244779468109755E-15 ) ) ;
#90302 = AXIS2_PLACEMENT_3D ( 'NONE', #15069, #26863, #45869 ) ;
#90304 = DIRECTION ( 'NONE',  ( 0.000000000000000000, 1.000000000000000000, 0.000000000000000000 ) ) ;
#90305 = AXIS2_PLACEMENT_3D ( 'NONE', #1436, #119933, #135 ) ;
#90306 = CONICAL_SURFACE ( 'NONE', #67307, 0.1000000000000002554, 0.003490658503988666988 ) ;
#90307 = CONICAL_SURFACE ( 'NONE', #36048, 0.09999999999999999167, 0.003490658503988666988 ) ;
#90308 = CARTESIAN_POINT ( 'NONE',  ( 6.649999999999928413, 2.500000000000000000, 2.757883832488649656 ) ) ;
#90309 = FACE_OUTER_BOUND ( 'NONE', #32992, .T. ) ;
#90310 = ORIENTED_EDGE ( 'NONE', *, *, #10260, .T. ) ;
#90311 = CARTESIAN_POINT ( 'NONE',  ( 12.09999999999990550, 2.500000000000000000, 5.122947341949749323 ) ) ;
#90312 = CIRCLE ( 'NONE', #88158, 0.06509327318403745899 ) ;
#90313 = DIRECTION ( 'NONE',  ( -0.000000000000000000, 1.000000000000000000, -0.000000000000000000 ) ) ;
#90314 = DIRECTION ( 'NONE',  ( 0.000000000000000000, 0.000000000000000000, 1.000000000000000000 ) ) ;
#90315 = CARTESIAN_POINT ( 'NONE',  ( -7.050000000000013145, 12.50000000000000000, 6.495190528383297135 ) ) ;
#90316 = ORIENTED_EDGE ( 'NONE', *, *, #37731, .T. ) ;
#90317 = ORIENTED_EDGE ( 'NONE', *, *, #112530, .F. ) ;
#90318 = DIRECTION ( 'NONE',  ( 0.000000000000000000, 1.000000000000000000, 0.000000000000000000 ) ) ;
#90319 = EDGE_LOOP ( 'NONE', ( #30117, #74752 ) ) ;
#90320 = DIRECTION ( 'NONE',  ( -0.000000000000000000, -1.000000000000000000, -0.000000000000000000 ) ) ;
#90321 = CARTESIAN_POINT ( 'NONE',  ( 3.949999999999938005, 2.500000000000000000, 6.841600689897072485 ) ) ;
#90322 = EDGE_CURVE ( 'NONE', #32289, #11740, #5880, .T. ) ;
#90323 = DIRECTION ( 'NONE',  ( 0.000000000000000000, 1.000000000000000000, 0.000000000000000000 ) ) ;
#90324 = ORIENTED_EDGE ( 'NONE', *, *, #12912, .T. ) ;
#90325 = DIRECTION ( 'NONE',  ( -4.274815082592931898E-19, -0.9999939076577903929, -0.003490651415223739937 ) ) ;
#90326 = DIRECTION ( 'NONE',  ( 0.000000000000000000, 0.000000000000000000, -1.000000000000000000 ) ) ;
#90327 = CARTESIAN_POINT ( 'NONE',  ( -12.09999999999999432, 2.500000000000000000, 5.022947341949748790 ) ) ;
#90328 = LINE ( 'NONE', #119812, #20395 ) ;
#90329 = DIRECTION ( 'NONE',  ( 0.000000000000000000, 0.000000000000000000, 1.000000000000000000 ) ) ;
#90330 = ADVANCED_FACE ( 'NONE', ( #64815 ), #67362, .T. ) ;
#90331 = CARTESIAN_POINT ( 'NONE',  ( 0.5999999999999612310, 12.50000000000000000, -0.3464101615137760715 ) ) ;
#90332 = ADVANCED_FACE ( 'NONE', ( #114556 ), #95917, .T. ) ;
#90333 = ORIENTED_EDGE ( 'NONE', *, *, #88631, .F. ) ;
#90334 = EDGE_LOOP ( 'NONE', ( #51783, #114739 ) ) ;
#90335 = CARTESIAN_POINT ( 'NONE',  ( -11.24999999999996270, 2.500000000000000000, 6.495190528383297135 ) ) ;
#90336 = VERTEX_POINT ( 'NONE', #16965 ) ;
#90337 = AXIS2_PLACEMENT_3D ( 'NONE', #80975, #31240, #111047 ) ;
#90338 = CARTESIAN_POINT ( 'NONE',  ( -4.150000000000025224, 2.500000000000000000, 7.188010851410848723 ) ) ;
#90339 = CIRCLE ( 'NONE', #84088, 0.1000000000000002554 ) ;
#90340 = EDGE_CURVE ( 'NONE', #24778, #44661, #6021, .T. ) ;
#90341 = CIRCLE ( 'NONE', #125852, 0.09999999999999982514 ) ;
#90343 = ORIENTED_EDGE ( 'NONE', *, *, #36901, .F. ) ;
#90342 = ORIENTED_EDGE ( 'NONE', *, *, #36321, .F. ) ;
#90344 = EDGE_CURVE ( 'NONE', #99703, #93625, #125028, .T. ) ;
#90345 = ORIENTED_EDGE ( 'NONE', *, *, #115428, .T. ) ;
#90346 = EDGE_CURVE ( 'NONE', #111372, #65580, #84467, .T. ) ;
#90347 = CARTESIAN_POINT ( 'NONE',  ( 17.50000000000000000, 1.666666666666669627, -3.999999999999996447 ) ) ;
#90348 = EDGE_CURVE ( 'NONE', #28873, #49975, #89665, .T. ) ;
#90349 = PLANE ( 'NONE',  #84096 ) ;
#90350 = AXIS2_PLACEMENT_3D ( 'NONE', #94793, #107177, #85611 ) ;
#90352 = CARTESIAN_POINT ( 'NONE',  ( 7.949999999999925571, 12.50000000000000000, 2.165063509461097713 ) ) ;
#90351 = CONICAL_SURFACE ( 'NONE', #125859, 0.1000000000000000472, 0.003490658503988666988 ) ;
#90353 = VECTOR ( 'NONE', #58349, 1000.000000000000000 ) ;
#90354 = EDGE_CURVE ( 'NONE', #4982, #56070, #24816, .T. ) ;
#90355 = CARTESIAN_POINT ( 'NONE',  ( -3.150000000000033218, 2.500000000000000000, -6.741600689897078169 ) ) ;
#90356 = DIRECTION ( 'NONE',  ( 0.000000000000000000, -0.9999939076577903929, 0.003490651415223739937 ) ) ;
#90357 = DIRECTION ( 'NONE',  ( 0.000000000000000000, -0.9999939076577903929, 0.003490651415223739937 ) ) ;
#90358 = DIRECTION ( 'NONE',  ( -0.000000000000000000, 1.000000000000000000, -0.000000000000000000 ) ) ;
#90359 = DIRECTION ( 'NONE',  ( 0.000000000000000000, 0.000000000000000000, -1.000000000000000000 ) ) ;
#90360 = CIRCLE ( 'NONE', #15125, 4.000000000000000000 ) ;
#90362 = EDGE_CURVE ( 'NONE', #35098, #73050, #97969, .T. ) ;
#90361 = DIRECTION ( 'NONE',  ( -0.000000000000000000, 1.000000000000000000, -0.000000000000000000 ) ) ;
#90363 = AXIS2_PLACEMENT_3D ( 'NONE', #24079, #63999, #105204 ) ;
#90364 = ORIENTED_EDGE ( 'NONE', *, *, #28221, .F. ) ;
#90365 = FACE_OUTER_BOUND ( 'NONE', #2450, .T. ) ;
#90366 = ORIENTED_EDGE ( 'NONE', *, *, #21071, .F. ) ;
#90367 = ORIENTED_EDGE ( 'NONE', *, *, #29686, .F. ) ;
#90368 = FACE_OUTER_BOUND ( 'NONE', #87053, .T. ) ;
#90369 = FACE_OUTER_BOUND ( 'NONE', #26272, .T. ) ;
#90370 = DIRECTION ( 'NONE',  ( 0.000000000000000000, 0.000000000000000000, -1.000000000000000000 ) ) ;
#90371 = CARTESIAN_POINT ( 'NONE',  ( -9.600000000000006750, 2.500000000000000000, 0.6928203230275494784 ) ) ;
#90372 = CARTESIAN_POINT ( 'NONE',  ( -12.04999999999999538, 12.50000000000000000, 6.495190528383297135 ) ) ;
#90373 = DIRECTION ( 'NONE',  ( -0.000000000000000000, -1.000000000000000000, -0.000000000000000000 ) ) ;
#90374 = EDGE_LOOP ( 'NONE', ( #118746, #26338, #39377, #15083 ) ) ;
#90375 = AXIS2_PLACEMENT_3D ( 'NONE', #39587, #41515, #109593 ) ;
#90376 = EDGE_LOOP ( 'NONE', ( #24326, #81706 ) ) ;
#90377 = CARTESIAN_POINT ( 'NONE',  ( -4.600000000000028066, 2.500000000000000000, -3.737306695894649700 ) ) ;
#90378 = ORIENTED_EDGE ( 'NONE', *, *, #105742, .T. ) ;
#90379 = DIRECTION ( 'NONE',  ( 0.000000000000000000, 0.000000000000000000, 1.000000000000000000 ) ) ;
#90380 = ORIENTED_EDGE ( 'NONE', *, *, #54044, .T. ) ;
#90381 = EDGE_LOOP ( 'NONE', ( #57452, #55267, #72853, #34040 ) ) ;
#90382 = AXIS2_PLACEMENT_3D ( 'NONE', #56621, #86076, #73693 ) ;
#90383 = DIRECTION ( 'NONE',  ( -0.000000000000000000, 1.000000000000000000, -0.000000000000000000 ) ) ;
#90384 = CARTESIAN_POINT ( 'NONE',  ( 65.38811649227264411, -3.824344232458583459, -5.305600839591994244 ) ) ;
#90385 = VECTOR ( 'NONE', #90533, 1000.000000000000000 ) ;
#90386 = AXIS2_PLACEMENT_3D ( 'NONE', #10013, #100332, #49962 ) ;
#90387 = DIRECTION ( 'NONE',  ( 0.000000000000000000, 1.000000000000000000, 0.000000000000000000 ) ) ;
#90388 = AXIS2_PLACEMENT_3D ( 'NONE', #8139, #97816, #48087 ) ;
#90389 = EDGE_CURVE ( 'NONE', #30036, #75419, #35294, .T. ) ;
#90390 = CARTESIAN_POINT ( 'NONE',  ( 2.099999999999949463, 12.50000000000000000, 0.6928203230275494784 ) ) ;
#90391 = CARTESIAN_POINT ( 'NONE',  ( 87.50000000000001421, 3.413194297214861894, 6.711110875543778498 ) ) ;
#90392 = ORIENTED_EDGE ( 'NONE', *, *, #16438, .F. ) ;
#90393 = CARTESIAN_POINT ( 'NONE',  ( -3.150000000000032330, 2.500000000000000000, -6.148780366869526226 ) ) ;
#90394 = DIRECTION ( 'NONE',  ( 0.000000000000000000, 1.000000000000000000, 0.000000000000000000 ) ) ;
#90395 = CARTESIAN_POINT ( 'NONE',  ( 5.199999999999935341, 2.500000000000000000, -0.3464101615137783474 ) ) ;
#90396 = DIRECTION ( 'NONE',  ( 0.000000000000000000, 0.000000000000000000, 1.000000000000000000 ) ) ;
#90397 = AXIS2_PLACEMENT_3D ( 'NONE', #107993, #79826, #9154 ) ;
#90398 = AXIS2_PLACEMENT_3D ( 'NONE', #37991, #26249, #58294 ) ;
#90400 = EDGE_CURVE ( 'NONE', #56590, #95073, #54997, .T. ) ;
#90399 = FACE_OUTER_BOUND ( 'NONE', #27714, .T. ) ;
#90401 = ORIENTED_EDGE ( 'NONE', *, *, #82820, .T. ) ;
#90402 = AXIS2_PLACEMENT_3D ( 'NONE', #116444, #26788, #35967 ) ;
#90403 = AXIS2_PLACEMENT_3D ( 'NONE', #5204, #43238, #102763 ) ;
#90404 = ORIENTED_EDGE ( 'NONE', *, *, #98833, .T. ) ;
#90405 = CARTESIAN_POINT ( 'NONE',  ( 0.3999999999999568345, 2.500000000000000000, -3.537306695894649966 ) ) ;
#90406 = AXIS2_PLACEMENT_3D ( 'NONE', #114455, #59437, #20133 ) ;
#90407 = VERTEX_POINT ( 'NONE', #87034 ) ;
#90408 = DIRECTION ( 'NONE',  ( 0.000000000000000000, 0.000000000000000000, 1.000000000000000000 ) ) ;
#90409 = DIRECTION ( 'NONE',  ( -0.000000000000000000, -1.000000000000000000, -0.000000000000000000 ) ) ;
#90410 = AXIS2_PLACEMENT_3D ( 'NONE', #6420, #54907, #13688 ) ;
#90411 = VERTEX_POINT ( 'NONE', #26836 ) ;
#90412 = DIRECTION ( 'NONE',  ( 0.000000000000000000, 0.000000000000000000, 1.000000000000000000 ) ) ;
#90413 = DIRECTION ( 'NONE',  ( 0.000000000000000000, 0.000000000000000000, 1.000000000000000000 ) ) ;
#90414 = DIRECTION ( 'NONE',  ( 0.000000000000000000, -0.000000000000000000, 1.000000000000000000 ) ) ;
#90415 = DIRECTION ( 'NONE',  ( 0.000000000000000000, 0.000000000000000000, 1.000000000000000000 ) ) ;
#90416 = DIRECTION ( 'NONE',  ( -0.000000000000000000, -1.000000000000000000, -0.000000000000000000 ) ) ;
#90417 = ORIENTED_EDGE ( 'NONE', *, *, #17666, .T. ) ;
#90418 = CIRCLE ( 'NONE', #40279, 0.09999999999999982514 ) ;
#90419 = CARTESIAN_POINT ( 'NONE',  ( 65.40463321312788025, 3.824478825999977794, -5.306487653624172296 ) ) ;
#90420 = DIRECTION ( 'NONE',  ( 0.000000000000000000, 0.000000000000000000, -1.000000000000000000 ) ) ;
#90421 = LINE ( 'NONE', #48594, #36606 ) ;
#90422 = LINE ( 'NONE', #60982, #16645 ) ;
#90423 = EDGE_CURVE ( 'NONE', #53181, #19084, #77138, .T. ) ;
#90424 = ORIENTED_EDGE ( 'NONE', *, *, #1396, .T. ) ;
#90425 = AXIS2_PLACEMENT_3D ( 'NONE', #104663, #74577, #86311 ) ;
#90426 = AXIS2_PLACEMENT_3D ( 'NONE', #383, #125635, #50164 ) ;
#90427 = ORIENTED_EDGE ( 'NONE', *, *, #108413, .T. ) ;
#90428 = DIRECTION ( 'NONE',  ( 0.000000000000000000, 0.000000000000000000, 1.000000000000000000 ) ) ;
#90429 = LINE ( 'NONE', #40735, #63384 ) ;
#90430 = FACE_OUTER_BOUND ( 'NONE', #79266, .T. ) ;
#90431 = VERTEX_POINT ( 'NONE', #16342 ) ;
#90432 = ADVANCED_FACE ( 'NONE', ( #45835 ), #6506, .T. ) ;
#90434 = CARTESIAN_POINT ( 'NONE',  ( 6.649999999999931966, 2.500000000000000000, -5.702370205355749455 ) ) ;
#90433 = CONICAL_SURFACE ( 'NONE', #96698, 0.09999999999999999167, 0.003490658503988666988 ) ;
#90435 = CIRCLE ( 'NONE', #42347, 0.06509327318403745899 ) ;
#90436 = AXIS2_PLACEMENT_3D ( 'NONE', #114239, #74960, #95890 ) ;
#90437 = DIRECTION ( 'NONE',  ( 0.000000000000000000, 1.000000000000000000, 0.000000000000000000 ) ) ;
#90438 = AXIS2_PLACEMENT_3D ( 'NONE', #26770, #115788, #116420 ) ;
#90439 = ORIENTED_EDGE ( 'NONE', *, *, #61067, .F. ) ;
#90440 = AXIS2_PLACEMENT_3D ( 'NONE', #90626, #40918, #28500 ) ;
#90441 = ADVANCED_FACE ( 'NONE', ( #80460 ), #3971, .T. ) ;
#90442 = AXIS2_PLACEMENT_3D ( 'NONE', #78145, #29049, #57860 ) ;
#90443 = CARTESIAN_POINT ( 'NONE',  ( -12.09999999999999609, 2.500000000000000000, -5.022947341949751454 ) ) ;
#90444 = ADVANCED_FACE ( 'NONE', ( #78537 ), #119084, .T. ) ;
#90445 = ORIENTED_EDGE ( 'NONE', *, *, #64221, .T. ) ;
#90446 = CONICAL_SURFACE ( 'NONE', #63278, 0.09999999999999982514, 0.003490658503988666988 ) ;
#90447 = CARTESIAN_POINT ( 'NONE',  ( -5.000000000000022204, 2.500000000000000000, 3.537306695894645081 ) ) ;
#90448 = ORIENTED_EDGE ( 'NONE', *, *, #64591, .F. ) ;
#90449 = CARTESIAN_POINT ( 'NONE',  ( 7.099999999999928590, 2.500000000000000000, -4.230127018922201998 ) ) ;
#90450 = CARTESIAN_POINT ( 'NONE',  ( -0.2000000000000339284, 2.500000000000000000, -0.4464101615137759382 ) ) ;
#90451 = ADVANCED_FACE ( 'NONE', ( #29419 ), #120377, .T. ) ;
#90452 = EDGE_LOOP ( 'NONE', ( #93172, #102945, #92054, #84077 ) ) ;
#90453 = ORIENTED_EDGE ( 'NONE', *, *, #7205, .F. ) ;
#90454 = EDGE_CURVE ( 'NONE', #69316, #97467, #28780, .T. ) ;
#90455 = FACE_OUTER_BOUND ( 'NONE', #36994, .T. ) ;
#90456 = DIRECTION ( 'NONE',  ( 0.000000000000000000, 0.000000000000000000, 1.000000000000000000 ) ) ;
#90457 = ORIENTED_EDGE ( 'NONE', *, *, #56214, .T. ) ;
#90458 = AXIS2_PLACEMENT_3D ( 'NONE', #86735, #97839, #8168 ) ;
#90459 = CARTESIAN_POINT ( 'NONE',  ( -5.600000000000020073, 2.500000000000000000, -0.3464101615137782364 ) ) ;
#90460 = DIRECTION ( 'NONE',  ( 0.000000000000000000, 0.000000000000000000, 1.000000000000000000 ) ) ;
#90461 = LINE ( 'NONE', #91125, #49529 ) ;
#90462 = CARTESIAN_POINT ( 'NONE',  ( 103.0345226653136450, 8.680034755040322736, 0.6735062902075328317 ) ) ;
#90463 = CARTESIAN_POINT ( 'NONE',  ( 87.50000000000001421, 3.975350567648425759, 6.360562287258741065 ) ) ;
#90464 = CARTESIAN_POINT ( 'NONE',  ( 4.999999999999935163, 12.50000000000000000, 3.702399969078682407 ) ) ;
#90465 = DIRECTION ( 'NONE',  ( -0.000000000000000000, -1.000000000000000000, -0.000000000000000000 ) ) ;
#90466 = CONICAL_SURFACE ( 'NONE', #77962, 0.1000000000000000472, 0.003490658503988666988 ) ;
#90467 = CIRCLE ( 'NONE', #84215, 0.06509327318403745899 ) ;
#90468 = AXIS2_PLACEMENT_3D ( 'NONE', #52487, #91135, #2092 ) ;
#90469 = EDGE_LOOP ( 'NONE', ( #82062, #32575, #90149, #34447, #32655 ) ) ;
#90470 = ORIENTED_EDGE ( 'NONE', *, *, #29176, .F. ) ;
#90471 = VERTEX_POINT ( 'NONE', #60179 ) ;
#90472 = CARTESIAN_POINT ( 'NONE',  ( -13.09999999999999254, 2.500000000000000000, -4.776537180435974861 ) ) ;
#90473 = DIRECTION ( 'NONE',  ( 0.000000000000000000, -0.9999939076577903929, 0.003490651415223739937 ) ) ;
#90474 = DIRECTION ( 'NONE',  ( -0.000000000000000000, 1.000000000000000000, -0.000000000000000000 ) ) ;
#90476 = ORIENTED_EDGE ( 'NONE', *, *, #68476, .T. ) ;
#90475 = ORIENTED_EDGE ( 'NONE', *, *, #74835, .T. ) ;
#90477 = FACE_BOUND ( 'NONE', #44804, .T. ) ;
#90478 = ORIENTED_EDGE ( 'NONE', *, *, #51772, .F. ) ;
#90479 = AXIS2_PLACEMENT_3D ( 'NONE', #50375, #119119, #109953 ) ;
#90480 = CARTESIAN_POINT ( 'NONE',  ( -0.8500000000000386136, 12.50000000000000000, 7.188010851410848723 ) ) ;
#90481 = CARTESIAN_POINT ( 'NONE',  ( 139.9358549477330200, 2.500000000000000000, -1.098523788719517169 ) ) ;
#90482 = CIRCLE ( 'NONE', #29864, 0.06509327318403745899 ) ;
#90484 = FACE_OUTER_BOUND ( 'NONE', #98144, .T. ) ;
#90483 = AXIS2_PLACEMENT_3D ( 'NONE', #19679, #30155, #89700 ) ;
#90485 = CARTESIAN_POINT ( 'NONE',  ( -3.100000000000028511, 2.500000000000000000, 0.3464101615137736845 ) ) ;
#90486 = AXIS2_PLACEMENT_3D ( 'NONE', #58407, #110073, #18462 ) ;
#90487 = CARTESIAN_POINT ( 'NONE',  ( -13.14999999999999147, 2.500000000000000000, 1.818653347947325472 ) ) ;
#90488 = PLANE ( 'NONE',  #29764 ) ;
#90489 = CARTESIAN_POINT ( 'NONE',  ( 0.3999999999999563904, 2.500000000000000000, 5.022947341949748790 ) ) ;
#90490 = LINE ( 'NONE', #121257, #10167 ) ;
#90491 = CARTESIAN_POINT ( 'NONE',  ( 9.999999999999948486, 2.500000000000000000, 4.330127018922196314 ) ) ;
#90492 = VECTOR ( 'NONE', #118310, 1000.000000000000000 ) ;
#90493 = LINE ( 'NONE', #42061, #84811 ) ;
#90494 = ADVANCED_FACE ( 'NONE', ( #107324 ), #112651, .T. ) ;
#90495 = AXIS2_PLACEMENT_3D ( 'NONE', #31193, #101849, #22018 ) ;
#90496 = VERTEX_POINT ( 'NONE', #57595 ) ;
#90497 = EDGE_LOOP ( 'NONE', ( #63858, #22556, #41885, #31004 ) ) ;
#90498 = ORIENTED_EDGE ( 'NONE', *, *, #100237, .T. ) ;
#90500 = EDGE_LOOP ( 'NONE', ( #83941, #101371 ) ) ;
#90499 = AXIS2_PLACEMENT_3D ( 'NONE', #1191, #82995, #41143 ) ;
#90501 = AXIS2_PLACEMENT_3D ( 'NONE', #36639, #116454, #28089 ) ;
#90502 = CIRCLE ( 'NONE', #42507, 0.06509327318403745899 ) ;
#90503 = CARTESIAN_POINT ( 'NONE',  ( 11.64999999999990266, 2.500000000000000000, -6.395190528383301931 ) ) ;
#90504 = EDGE_CURVE ( 'NONE', #114462, #24394, #72937, .T. ) ;
#90505 = CARTESIAN_POINT ( 'NONE',  ( -1.250000000000001554, 12.50000000000000000, 2.165063509461097713 ) ) ;
#90506 = ADVANCED_FACE ( 'NONE', ( #117765 ), #128273, .T. ) ;
#90508 = ORIENTED_EDGE ( 'NONE', *, *, #26068, .T. ) ;
#90507 = ORIENTED_EDGE ( 'NONE', *, *, #33434, .F. ) ;
#90509 = EDGE_LOOP ( 'NONE', ( #113339, #1632, #61141, #90931 ) ) ;
#90510 = CIRCLE ( 'NONE', #42512, 0.06509327318403745899 ) ;
#90511 = EDGE_CURVE ( 'NONE', #38970, #100810, #26976, .T. ) ;
#90512 = CARTESIAN_POINT ( 'NONE',  ( -0.6000000000000383915, 12.50000000000000000, -4.676537180435977881 ) ) ;
#90513 = ADVANCED_FACE ( 'NONE', ( #68040 ), #54164, .T. ) ;
#90514 = CARTESIAN_POINT ( 'NONE',  ( -2.300000000000033573, 12.50000000000000000, 4.676537180435972552 ) ) ;
#90515 = CIRCLE ( 'NONE', #96761, 0.1000000000000002554 ) ;
#90516 = DIRECTION ( 'NONE',  ( 0.000000000000000000, 0.000000000000000000, 1.000000000000000000 ) ) ;
#90517 = DIRECTION ( 'NONE',  ( 0.000000000000000000, 0.000000000000000000, -1.000000000000000000 ) ) ;
#90518 = EDGE_CURVE ( 'NONE', #55517, #116823, #18295, .T. ) ;
#90519 = DIRECTION ( 'NONE',  ( -0.000000000000000000, 1.000000000000000000, -0.000000000000000000 ) ) ;
#90520 = DIRECTION ( 'NONE',  ( -0.000000000000000000, 1.000000000000000000, -0.000000000000000000 ) ) ;
#90521 = DIRECTION ( 'NONE',  ( 0.000000000000000000, 1.000000000000000000, 0.000000000000000000 ) ) ;
#90522 = VERTEX_POINT ( 'NONE', #58244 ) ;
#90524 = EDGE_CURVE ( 'NONE', #78169, #72699, #70887, .T. ) ;
#90523 = DIRECTION ( 'NONE',  ( 0.000000000000000000, 1.000000000000000000, 0.000000000000000000 ) ) ;
#90525 = VERTEX_POINT ( 'NONE', #89621 ) ;
#90526 = ADVANCED_FACE ( 'NONE', ( #109248 ), #16480, .T. ) ;
#90527 = VERTEX_POINT ( 'NONE', #9126 ) ;
#90528 = EDGE_LOOP ( 'NONE', ( #16241, #52804 ) ) ;
#90529 = DIRECTION ( 'NONE',  ( -1.000000000000000000, 0.000000000000000000, 1.224646799147352221E-16 ) ) ;
#90530 = AXIS2_PLACEMENT_3D ( 'NONE', #53672, #73302, #62221 ) ;
#90531 = VERTEX_POINT ( 'NONE', #88978 ) ;
#90532 = ORIENTED_EDGE ( 'NONE', *, *, #78530, .T. ) ;
#90533 = DIRECTION ( 'NONE',  ( -4.274815082592931898E-19, -0.9999939076577903929, -0.003490651415223739937 ) ) ;
#90535 = DIRECTION ( 'NONE',  ( 0.000000000000000000, 0.000000000000000000, 1.000000000000000000 ) ) ;
#90534 = AXIS2_PLACEMENT_3D ( 'NONE', #22037, #41684, #121487 ) ;
#90536 = FACE_OUTER_BOUND ( 'NONE', #106475, .T. ) ;
#90538 = DIRECTION ( 'NONE',  ( 0.000000000000000000, -0.9999939076577903929, 0.003490651415223739937 ) ) ;
#90537 = CIRCLE ( 'NONE', #38325, 0.09999999999999982514 ) ;
#90539 = DIRECTION ( 'NONE',  ( 0.000000000000000000, 0.000000000000000000, -1.000000000000000000 ) ) ;
#90540 = CIRCLE ( 'NONE', #98848, 0.06509327318403745899 ) ;
#90541 = AXIS2_PLACEMENT_3D ( 'NONE', #36336, #105034, #16647 ) ;
#90542 = DIRECTION ( 'NONE',  ( -4.274815082592931898E-19, -0.9999939076577903929, -0.003490651415223739937 ) ) ;
#90543 = EDGE_CURVE ( 'NONE', #38720, #7794, #104240, .T. ) ;
#90544 = CARTESIAN_POINT ( 'NONE',  ( -12.49999999999995914, 2.500000000000000000, -4.430127018922199511 ) ) ;
#90546 = ORIENTED_EDGE ( 'NONE', *, *, #22000, .F. ) ;
#90545 = AXIS2_PLACEMENT_3D ( 'NONE', #56118, #14881, #67198 ) ;
#90547 = CARTESIAN_POINT ( 'NONE',  ( 21.24748443165277223, 0.7426079187842503648, 4.181982372968837680 ) ) ;
#90548 = CIRCLE ( 'NONE', #67544, 0.09999999999999982514 ) ;
#90549 = ORIENTED_EDGE ( 'NONE', *, *, #65318, .T. ) ;
#90550 = CARTESIAN_POINT ( 'NONE',  ( 112.7289338494457809, 8.546997317143256723, 1.632411909918629167 ) ) ;
#90551 = CARTESIAN_POINT ( 'NONE',  ( 0.8499999999999550138, 2.500000000000000000, -5.802370205355749988 ) ) ;
#90552 = AXIS2_PLACEMENT_3D ( 'NONE', #67969, #47709, #18223 ) ;
#90553 = ORIENTED_EDGE ( 'NONE', *, *, #111671, .T. ) ;
#90554 = AXIS2_PLACEMENT_3D ( 'NONE', #117910, #58375, #98270 ) ;
#90555 = DIRECTION ( 'NONE',  ( 0.000000000000000000, 0.000000000000000000, 1.000000000000000000 ) ) ;
#90556 = DIRECTION ( 'NONE',  ( 0.000000000000000000, -0.9999939076577903929, 0.003490651415223739937 ) ) ;
#90557 = ORIENTED_EDGE ( 'NONE', *, *, #84359, .F. ) ;
#90558 = AXIS2_PLACEMENT_3D ( 'NONE', #31815, #120197, #81554 ) ;
#90559 = DIRECTION ( 'NONE',  ( -0.000000000000000000, 1.000000000000000000, -0.000000000000000000 ) ) ;
#90560 = VERTEX_POINT ( 'NONE', #99455 ) ;
#90561 = ORIENTED_EDGE ( 'NONE', *, *, #97697, .F. ) ;
#90562 = DIRECTION ( 'NONE',  ( -0.000000000000000000, -1.000000000000000000, -0.000000000000000000 ) ) ;
#90563 = DIRECTION ( 'NONE',  ( 0.000000000000000000, -0.000000000000000000, 1.000000000000000000 ) ) ;
#90564 = LINE ( 'NONE', #900, #41820 ) ;
#90565 = DIRECTION ( 'NONE',  ( 0.000000000000000000, -0.9999939076577903929, 0.003490651415223739937 ) ) ;
#90566 = AXIS2_PLACEMENT_3D ( 'NONE', #84656, #82742, #112832 ) ;
#90568 = EDGE_CURVE ( 'NONE', #97131, #65281, #9770, .T. ) ;
#90567 = DIRECTION ( 'NONE',  ( -0.000000000000000000, 1.000000000000000000, -0.000000000000000000 ) ) ;
#90569 = EDGE_LOOP ( 'NONE', ( #115120, #69079 ) ) ;
#90570 = CARTESIAN_POINT ( 'NONE',  ( 3.949999999999942446, 12.50000000000000000, -2.446380397790840266 ) ) ;
#90571 = VECTOR ( 'NONE', #12974, 1000.000000000000000 ) ;
#90572 = VERTEX_POINT ( 'NONE', #119715 ) ;
#90573 = CONICAL_SURFACE ( 'NONE', #42480, 0.1000000000000002554, 0.003490658503988666988 ) ;
#90574 = DIRECTION ( 'NONE',  ( -0.000000000000000000, 1.000000000000000000, -0.000000000000000000 ) ) ;
#90575 = DIRECTION ( 'NONE',  ( 0.000000000000000000, 1.000000000000000000, 0.000000000000000000 ) ) ;
#90576 =( GEOMETRIC_REPRESENTATION_CONTEXT ( 3 ) GLOBAL_UNCERTAINTY_ASSIGNED_CONTEXT ( ( #103088 ) ) GLOBAL_UNIT_ASSIGNED_CONTEXT ( ( #18362, #29486, #59615 ) ) REPRESENTATION_CONTEXT ( 'NONE', 'WORKASPACE' ) );
#90577 = CARTESIAN_POINT ( 'NONE',  ( 186.0052083336747444, -6.551208109652278289, 3.782341765624995134 ) ) ;
#90578 = DIRECTION ( 'NONE',  ( 0.000000000000000000, 0.000000000000000000, -1.000000000000000000 ) ) ;
#90579 = CARTESIAN_POINT ( 'NONE',  ( 6.849999999999927702, 12.50000000000000000, 2.511473670974873507 ) ) ;
#90580 = DIRECTION ( 'NONE',  ( 0.000000000000000000, 0.000000000000000000, 1.000000000000000000 ) ) ;
#90581 = AXIS2_PLACEMENT_3D ( 'NONE', #4466, #44419, #41861 ) ;
#90583 = VECTOR ( 'NONE', #12299, 1000.000000000000000 ) ;
#90582 = DIRECTION ( 'NONE',  ( -0.000000000000000000, -1.000000000000000000, -0.000000000000000000 ) ) ;
#90584 = VERTEX_POINT ( 'NONE', #50341 ) ;
#90585 = CONICAL_SURFACE ( 'NONE', #59321, 0.1000000000000002554, 0.003490658503988666988 ) ;
#90586 = DIRECTION ( 'NONE',  ( -0.000000000000000000, 1.000000000000000000, -0.000000000000000000 ) ) ;
#90587 = DIRECTION ( 'NONE',  ( 0.000000000000000000, 0.000000000000000000, 1.000000000000000000 ) ) ;
#90588 = DIRECTION ( 'NONE',  ( -0.000000000000000000, 1.000000000000000000, -0.000000000000000000 ) ) ;
#90589 = CONICAL_SURFACE ( 'NONE', #709, 0.1000000000000000472, 0.003490658503988666988 ) ;
#90590 = VERTEX_POINT ( 'NONE', #90242 ) ;
#90591 = CARTESIAN_POINT ( 'NONE',  ( 11.24999999999990763, 12.50000000000000000, -7.188010851410854052 ) ) ;
#90592 = ORIENTED_EDGE ( 'NONE', *, *, #119407, .F. ) ;
#90593 = VECTOR ( 'NONE', #298, 1000.000000000000000 ) ;
#90595 = ORIENTED_EDGE ( 'NONE', *, *, #33871, .F. ) ;
#90594 = AXIS2_PLACEMENT_3D ( 'NONE', #84102, #35037, #93939 ) ;
#90596 = CONICAL_SURFACE ( 'NONE', #82300, 0.1000000000000002554, 0.003490658503988666988 ) ;
#90597 = CARTESIAN_POINT ( 'NONE',  ( 2.949999999999945111, 2.500000000000000000, 2.165063509461097713 ) ) ;
#90599 = ORIENTED_EDGE ( 'NONE', *, *, #48595, .F. ) ;
#90598 = CONICAL_SURFACE ( 'NONE', #76037, 0.1000000000000002554, 0.003490658503988666988 ) ;
#90600 = FACE_OUTER_BOUND ( 'NONE', #6812, .T. ) ;
#90601 = DIRECTION ( 'NONE',  ( -0.000000000000000000, 1.000000000000000000, -0.000000000000000000 ) ) ;
#90602 = EDGE_LOOP ( 'NONE', ( #95373, #110955 ) ) ;
#90603 = ADVANCED_FACE ( 'NONE', ( #580 ), #123114, .T. ) ;
#90604 = FACE_OUTER_BOUND ( 'NONE', #8093, .T. ) ;
#90605 = DIRECTION ( 'NONE',  ( 0.000000000000000000, 1.000000000000000000, 0.000000000000000000 ) ) ;
#90606 = CARTESIAN_POINT ( 'NONE',  ( 4.349999999999939249, 12.50000000000000000, 2.511473670974873507 ) ) ;
#90607 = EDGE_CURVE ( 'NONE', #89818, #73855, #100134, .T. ) ;
#90608 = EDGE_CURVE ( 'NONE', #103695, #103569, #71259, .T. ) ;
#90609 = ORIENTED_EDGE ( 'NONE', *, *, #91360, .F. ) ;
#90610 = ORIENTED_EDGE ( 'NONE', *, *, #126161, .T. ) ;
#90611 = ORIENTED_EDGE ( 'NONE', *, *, #122700, .T. ) ;
#90612 = DIRECTION ( 'NONE',  ( 0.000000000000000000, 0.000000000000000000, 1.000000000000000000 ) ) ;
#90613 = CARTESIAN_POINT ( 'NONE',  ( -9.999999999999971578, 12.50000000000000000, -4.330127018922197202 ) ) ;
#90614 = EDGE_CURVE ( 'NONE', #45894, #37222, #121012, .T. ) ;
#90615 = EDGE_CURVE ( 'NONE', #104775, #97182, #12284, .T. ) ;
#90616 = DIRECTION ( 'NONE',  ( 0.000000000000000000, 0.000000000000000000, 1.000000000000000000 ) ) ;
#90617 = AXIS2_PLACEMENT_3D ( 'NONE', #127389, #128707, #16755 ) ;
#90618 = ADVANCED_FACE ( 'NONE', ( #22190 ), #118903, .T. ) ;
#90619 = FACE_BOUND ( 'NONE', #37380, .T. ) ;
#90621 = EDGE_CURVE ( 'NONE', #51095, #18351, #102190, .T. ) ;
#90620 = EDGE_LOOP ( 'NONE', ( #30537, #69002 ) ) ;
#90622 = EDGE_CURVE ( 'NONE', #121481, #36772, #87684, .T. ) ;
#90623 = CARTESIAN_POINT ( 'NONE',  ( -14.79999999999998472, 2.500000000000000000, 0.3464101615137758494 ) ) ;
#90624 = DIRECTION ( 'NONE',  ( -4.274815082592931898E-19, -0.9999939076577903929, -0.003490651415223739937 ) ) ;
#90625 = ORIENTED_EDGE ( 'NONE', *, *, #1698, .F. ) ;
#90626 = CARTESIAN_POINT ( 'NONE',  ( -7.500000000000011546, 2.500000000000000000, 3.637306695894644726 ) ) ;
#90628 = CARTESIAN_POINT ( 'NONE',  ( 0.3999999999999563904, 12.50000000000000000, 5.022947341949748790 ) ) ;
#90627 = AXIS2_PLACEMENT_3D ( 'NONE', #45385, #62450, #114744 ) ;
#90629 = VECTOR ( 'NONE', #15527, 1000.000000000000000 ) ;
#90630 = CIRCLE ( 'NONE', #65489, 0.1000000000000000056 ) ;
#90631 = CONICAL_SURFACE ( 'NONE', #27943, 0.1000000000000000472, 0.003490658503988666988 ) ;
#90632 = LINE ( 'NONE', #49444, #554 ) ;
#90633 = DIRECTION ( 'NONE',  ( 0.000000000000000000, 0.000000000000000000, -1.000000000000000000 ) ) ;
#90634 = DIRECTION ( 'NONE',  ( 0.000000000000000000, 0.000000000000000000, 1.000000000000000000 ) ) ;
#90635 = EDGE_CURVE ( 'NONE', #13143, #108629, #98059, .T. ) ;
#90636 = CARTESIAN_POINT ( 'NONE',  ( -2.900000000000029221, 2.500000000000000000, -4.922947341949753586 ) ) ;
#90637 = DIRECTION ( 'NONE',  ( 0.000000000000000000, 0.000000000000000000, -1.000000000000000000 ) ) ;
#90638 = AXIS2_PLACEMENT_3D ( 'NONE', #76586, #104112, #123726 ) ;
#90639 = AXIS2_PLACEMENT_3D ( 'NONE', #104207, #83297, #53820 ) ;
#90640 = AXIS2_PLACEMENT_3D ( 'NONE', #17189, #106251, #76798 ) ;
#90641 = ORIENTED_EDGE ( 'NONE', *, *, #83216, .T. ) ;
#90642 = EDGE_LOOP ( 'NONE', ( #44620, #93724 ) ) ;
#90643 = VERTEX_POINT ( 'NONE', #20884 ) ;
#90644 = EDGE_LOOP ( 'NONE', ( #129265, #114698, #54730, #28824 ) ) ;
#90645 = CARTESIAN_POINT ( 'NONE',  ( 5.849999999999933920, 2.500000000000000000, -2.757883832488654097 ) ) ;
#90646 = VECTOR ( 'NONE', #8437, 1000.000000000000000 ) ;
#90647 = DIRECTION ( 'NONE',  ( -4.274815082592931898E-19, -0.9999939076577903929, -0.003490651415223739937 ) ) ;
#90648 = ORIENTED_EDGE ( 'NONE', *, *, #67334, .F. ) ;
#90649 = FACE_BOUND ( 'NONE', #89361, .T. ) ;
#90650 = DIRECTION ( 'NONE',  ( -0.000000000000000000, -1.000000000000000000, -0.000000000000000000 ) ) ;
#90651 = DIRECTION ( 'NONE',  ( 0.000000000000000000, 0.000000000000000000, 1.000000000000000000 ) ) ;
#90652 = DIRECTION ( 'NONE',  ( -0.000000000000000000, 1.000000000000000000, -0.000000000000000000 ) ) ;
#90653 = DIRECTION ( 'NONE',  ( 0.000000000000000000, 1.000000000000000000, 0.000000000000000000 ) ) ;
#90654 = CARTESIAN_POINT ( 'NONE',  ( 5.199999999999933564, 12.50000000000000000, 3.983716857408420076 ) ) ;
#90655 = DIRECTION ( 'NONE',  ( 0.000000000000000000, -0.9999939076577903929, 0.003490651415223739937 ) ) ;
#90656 = LINE ( 'NONE', #21938, #78450 ) ;
#90657 = DIRECTION ( 'NONE',  ( 0.000000000000000000, 1.000000000000000000, 0.000000000000000000 ) ) ;
#90658 = ORIENTED_EDGE ( 'NONE', *, *, #105541, .F. ) ;
#90659 = CONICAL_SURFACE ( 'NONE', #126165, 0.1000000000000000056, 0.003490658503988666988 ) ;
#90660 = VERTEX_POINT ( 'NONE', #82396 ) ;
#90661 = ORIENTED_EDGE ( 'NONE', *, *, #95505, .F. ) ;
#90662 = ORIENTED_EDGE ( 'NONE', *, *, #46921, .T. ) ;
#90663 = ORIENTED_EDGE ( 'NONE', *, *, #67561, .F. ) ;
#90664 = ORIENTED_EDGE ( 'NONE', *, *, #35213, .F. ) ;
#90665 = FACE_OUTER_BOUND ( 'NONE', #84186, .T. ) ;
#90666 = ADVANCED_FACE ( 'NONE', ( #1239 ), #92855, .T. ) ;
#90667 = ORIENTED_EDGE ( 'NONE', *, *, #63505, .F. ) ;
#90668 = CIRCLE ( 'NONE', #34256, 0.06509327318403745899 ) ;
#90669 = ADVANCED_FACE ( 'NONE', ( #51645 ), #3815, .F. ) ;
#90670 = CIRCLE ( 'NONE', #4972, 0.1000000000000002554 ) ;
#90671 = AXIS2_PLACEMENT_3D ( 'NONE', #127332, #89333, #127960 ) ;
#90672 = EDGE_CURVE ( 'NONE', #113210, #112816, #112491, .T. ) ;
#90673 = DIRECTION ( 'NONE',  ( 0.000000000000000000, 1.000000000000000000, 0.000000000000000000 ) ) ;
#90674 = CARTESIAN_POINT ( 'NONE',  ( 184.1510416670080588, 4.367472073101518859, -7.564683531249999149 ) ) ;
#90675 = CARTESIAN_POINT ( 'NONE',  ( -9.800000000000006040, 2.500000000000000000, 0.4464101615137735513 ) ) ;
#90676 = DIRECTION ( 'NONE',  ( 0.000000000000000000, 0.000000000000000000, 1.000000000000000000 ) ) ;
#90677 = ADVANCED_FACE ( 'NONE', ( #12338 ), #96015, .T. ) ;
#90678 = AXIS2_PLACEMENT_3D ( 'NONE', #93372, #111048, #22713 ) ;
#90679 = ORIENTED_EDGE ( 'NONE', *, *, #38543, .F. ) ;
#90680 = FACE_OUTER_BOUND ( 'NONE', #69828, .T. ) ;
#90681 = CIRCLE ( 'NONE', #107402, 0.06509327318403745899 ) ;
#90682 = ADVANCED_FACE ( 'NONE', ( #83671 ), #52922, .T. ) ;
#90683 = ADVANCED_FACE ( 'NONE', ( #3182 ), #1913, .T. ) ;
#90684 = ORIENTED_EDGE ( 'NONE', *, *, #77824, .T. ) ;
#90685 = VECTOR ( 'NONE', #103146, 1000.000000000000000 ) ;
#90686 = ADVANCED_FACE ( 'NONE', ( #91555 ), #33297, .T. ) ;
#90687 = ORIENTED_EDGE ( 'NONE', *, *, #90831, .F. ) ;
#90688 = PLANE ( 'NONE',  #25989 ) ;
#90689 = DIRECTION ( 'NONE',  ( 0.000000000000000000, 0.000000000000000000, 1.000000000000000000 ) ) ;
#90690 = CARTESIAN_POINT ( 'NONE',  ( 4.149999999999936406, 2.500000000000000000, 6.395190528383296602 ) ) ;
#90691 = CONICAL_SURFACE ( 'NONE', #44734, 0.1000000000000000472, 0.003490658503988666988 ) ;
#90692 = ORIENTED_EDGE ( 'NONE', *, *, #98332, .F. ) ;
#90693 = EDGE_CURVE ( 'NONE', #87945, #78195, #123215, .T. ) ;
#90694 = ORIENTED_EDGE ( 'NONE', *, *, #89684, .F. ) ;
#90695 = PLANE ( 'NONE',  #6650 ) ;
#90697 = CIRCLE ( 'NONE', #69767, 0.06509327318403745899 ) ;
#90696 = CARTESIAN_POINT ( 'NONE',  ( 1.249999999999952038, 12.50000000000000000, 5.802370205355744659 ) ) ;
#90699 = AXIS2_PLACEMENT_3D ( 'NONE', #73266, #82463, #63454 ) ;
#90698 = LINE ( 'NONE', #69768, #85415 ) ;
#90700 = AXIS2_PLACEMENT_3D ( 'NONE', #127184, #48612, #29605 ) ;
#90701 = LINE ( 'NONE', #51440, #90072 ) ;
#90702 = VERTEX_POINT ( 'NONE', #76427 ) ;
#90703 = DIRECTION ( 'NONE',  ( 0.000000000000000000, 0.000000000000000000, 1.000000000000000000 ) ) ;
#90704 = VECTOR ( 'NONE', #14003, 1000.000000000000000 ) ;
#90705 = ORIENTED_EDGE ( 'NONE', *, *, #128813, .T. ) ;
#90706 = AXIS2_PLACEMENT_3D ( 'NONE', #59089, #38155, #86597 ) ;
#90707 = CARTESIAN_POINT ( 'NONE',  ( 13.12246079422085288, -2.500000000000001332, 7.156134183588244824 ) ) ;
#90708 = ORIENTED_EDGE ( 'NONE', *, *, #65098, .T. ) ;
#90709 = CARTESIAN_POINT ( 'NONE',  ( 87.50000000000001421, 4.424430252271040587, 6.079088403633666537 ) ) ;
#90710 = CARTESIAN_POINT ( 'NONE',  ( 0.3999999999999619971, 2.500000000000000000, -1.084202172485504434E-16 ) ) ;
#90711 = DIRECTION ( 'NONE',  ( -0.000000000000000000, -1.000000000000000000, -0.000000000000000000 ) ) ;
#90712 = ADVANCED_FACE ( 'NONE', ( #105234 ), #127411, .T. ) ;
#90713 = CARTESIAN_POINT ( 'NONE',  ( 1.899999999999949507, 2.500000000000000000, 3.883716857408421319 ) ) ;
#90714 = ORIENTED_EDGE ( 'NONE', *, *, #16495, .T. ) ;
#90715 = DIRECTION ( 'NONE',  ( -0.000000000000000000, -1.000000000000000000, -0.000000000000000000 ) ) ;
#90716 = CARTESIAN_POINT ( 'NONE',  ( 4.999999999999933387, 2.500000000000000000, 4.922947341949748257 ) ) ;
#90717 = ORIENTED_EDGE ( 'NONE', *, *, #41866, .F. ) ;
#90718 = VERTEX_POINT ( 'NONE', #115689 ) ;
#90719 = AXIS2_PLACEMENT_3D ( 'NONE', #110503, #100667, #10997 ) ;
#90720 = CIRCLE ( 'NONE', #105298, 0.1000000000000000472 ) ;
#90721 = VERTEX_POINT ( 'NONE', #116332 ) ;
#90722 = DIRECTION ( 'NONE',  ( 0.000000000000000000, -0.9999939076577903929, 0.003490651415223739937 ) ) ;
#90723 = DIRECTION ( 'NONE',  ( 0.000000000000000000, 0.000000000000000000, 1.000000000000000000 ) ) ;
#90724 = DIRECTION ( 'NONE',  ( -0.000000000000000000, 1.000000000000000000, -0.000000000000000000 ) ) ;
#90725 = FACE_OUTER_BOUND ( 'NONE', #98047, .T. ) ;
#90726 = FACE_OUTER_BOUND ( 'NONE', #69756, .T. ) ;
#90727 = DIRECTION ( 'NONE',  ( -0.000000000000000000, 1.000000000000000000, -0.000000000000000000 ) ) ;
#90728 = AXIS2_PLACEMENT_3D ( 'NONE', #94454, #95123, #15238 ) ;
#90729 = AXIS2_PLACEMENT_3D ( 'NONE', #102484, #92663, #122772 ) ;
#90731 = ADVANCED_FACE ( 'NONE', ( #15551 ), #39608, .T. ) ;
#90730 = CARTESIAN_POINT ( 'NONE',  ( 6.649999999999930189, 12.50000000000000000, -2.857883832488653741 ) ) ;
#90732 = AXIS2_PLACEMENT_3D ( 'NONE', #70519, #31262, #110443 ) ;
#90733 = DIRECTION ( 'NONE',  ( 0.000000000000000000, 0.000000000000000000, -1.000000000000000000 ) ) ;
#90735 = CIRCLE ( 'NONE', #51038, 0.1000000000000002554 ) ;
#90734 = DIRECTION ( 'NONE',  ( 0.000000000000000000, 0.000000000000000000, 1.000000000000000000 ) ) ;
#90736 = CIRCLE ( 'NONE', #99062, 0.1000000000000002554 ) ;
#90737 = ORIENTED_EDGE ( 'NONE', *, *, #40319, .F. ) ;
#90738 = DIRECTION ( 'NONE',  ( 0.000000000000000000, -0.000000000000000000, 1.000000000000000000 ) ) ;
#90739 = EDGE_CURVE ( 'NONE', #105289, #126127, #46974, .T. ) ;
#90740 = CARTESIAN_POINT ( 'NONE',  ( -4.119968255444916849E-14, 12.50000000000000000, 3.637306695894644726 ) ) ;
#90741 = LINE ( 'NONE', #1065, #90279 ) ;
#90742 = DIRECTION ( 'NONE',  ( 0.000000000000000000, -0.000000000000000000, 1.000000000000000000 ) ) ;
#90743 = ORIENTED_EDGE ( 'NONE', *, *, #123945, .F. ) ;
#90744 = PLANE ( 'NONE',  #46637 ) ;
#90745 = DIRECTION ( 'NONE',  ( 0.000000000000000000, 0.000000000000000000, -1.000000000000000000 ) ) ;
#90747 = ORIENTED_EDGE ( 'NONE', *, *, #95975, .T. ) ;
#90746 = DIRECTION ( 'NONE',  ( -4.274815082592931898E-19, -0.9999939076577903929, -0.003490651415223739937 ) ) ;
#90748 = AXIS2_PLACEMENT_3D ( 'NONE', #91175, #52540, #91820 ) ;
#90749 = VECTOR ( 'NONE', #36491, 1000.000000000000000 ) ;
#90750 = VERTEX_POINT ( 'NONE', #45683 ) ;
#90751 = CARTESIAN_POINT ( 'NONE',  ( 8.149999999999920419, 2.500000000000000000, 6.048780366869521252 ) ) ;
#90752 = ORIENTED_EDGE ( 'NONE', *, *, #42640, .F. ) ;
#90753 = ORIENTED_EDGE ( 'NONE', *, *, #60921, .F. ) ;
#90754 = CARTESIAN_POINT ( 'NONE',  ( 10.19999999999991047, 2.500000000000000000, -3.983716857408426293 ) ) ;
#90755 = CARTESIAN_POINT ( 'NONE',  ( -14.34999999999998543, 12.50000000000000000, 2.511473670974877503 ) ) ;
#90756 = FACE_OUTER_BOUND ( 'NONE', #108805, .T. ) ;
#90757 = CIRCLE ( 'NONE', #36402, 0.1000000000000000472 ) ;
#90758 = CARTESIAN_POINT ( 'NONE',  ( 10.84999999999990905, 2.500000000000000000, 1.472243186433545459 ) ) ;
#90759 = CONICAL_SURFACE ( 'NONE', #76101, 0.09999999999999982514, 0.003490658503988666988 ) ;
#90760 = EDGE_LOOP ( 'NONE', ( #52319, #34615 ) ) ;
#90761 = ADVANCED_FACE ( 'NONE', ( #113777 ), #104419, .T. ) ;
#90762 = FACE_OUTER_BOUND ( 'NONE', #121055, .T. ) ;
#90763 = ORIENTED_EDGE ( 'NONE', *, *, #60221, .F. ) ;
#90764 = LINE ( 'NONE', #1093, #115410 ) ;
#90765 = DIRECTION ( 'NONE',  ( -4.274815082592931898E-19, -0.9999939076577903929, -0.003490651415223739937 ) ) ;
#90766 = EDGE_CURVE ( 'NONE', #113146, #20664, #4424, .T. ) ;
#90767 = VERTEX_POINT ( 'NONE', #95422 ) ;
#90768 = CIRCLE ( 'NONE', #34362, 0.1000000000000002554 ) ;
#90769 = ORIENTED_EDGE ( 'NONE', *, *, #64312, .F. ) ;
#90770 = ORIENTED_EDGE ( 'NONE', *, *, #83409, .T. ) ;
#90771 = ORIENTED_EDGE ( 'NONE', *, *, #53531, .F. ) ;
#90772 = CARTESIAN_POINT ( 'NONE',  ( 10.39999999999991331, 12.50000000000000000, 0.06509327318403504425 ) ) ;
#90773 = CARTESIAN_POINT ( 'NONE',  ( -5.450000000000023270, 12.50000000000000000, -6.430097255199264339 ) ) ;
#90774 = ADVANCED_FACE ( 'NONE', ( #24750 ), #84305, .T. ) ;
#90775 = EDGE_CURVE ( 'NONE', #18351, #51095, #31279, .T. ) ;
#90776 = DIRECTION ( 'NONE',  ( 0.000000000000000000, 0.000000000000000000, -1.000000000000000000 ) ) ;
#90777 = ADVANCED_FACE ( 'NONE', ( #35855 ), #112751, .T. ) ;
#90778 = FACE_BOUND ( 'NONE', #90958, .T. ) ;
#90779 = EDGE_CURVE ( 'NONE', #47037, #113203, #114779, .T. ) ;
#90780 = DIRECTION ( 'NONE',  ( -0.000000000000000000, 1.000000000000000000, -0.000000000000000000 ) ) ;
#90781 = CARTESIAN_POINT ( 'NONE',  ( 185.9479166673494603, -6.668395609140176816, -3.850000000000003642 ) ) ;
#90782 = DIRECTION ( 'NONE',  ( -0.000000000000000000, 1.000000000000000000, -0.000000000000000000 ) ) ;
#90783 = DIRECTION ( 'NONE',  ( -0.000000000000000000, -1.000000000000000000, -0.000000000000000000 ) ) ;
#90784 = VECTOR ( 'NONE', #7213, 1000.000000000000000 ) ;
#90785 = AXIS2_PLACEMENT_3D ( 'NONE', #59742, #79996, #97061 ) ;
#90786 = DIRECTION ( 'NONE',  ( 0.000000000000000000, 0.000000000000000000, -1.000000000000000000 ) ) ;
#90787 = CARTESIAN_POINT ( 'NONE',  ( -4.150000000000025224, 2.500000000000000000, 7.088010851410848190 ) ) ;
#90788 = AXIS2_PLACEMENT_3D ( 'NONE', #34819, #45912, #125728 ) ;
#90789 = EDGE_CURVE ( 'NONE', #119719, #6241, #96683, .T. ) ;
#90790 = CARTESIAN_POINT ( 'NONE',  ( -12.09999999999999609, 12.50000000000000000, 1.734723475976807094E-15 ) ) ;
#90791 = AXIS2_PLACEMENT_3D ( 'NONE', #54706, #4964, #44916 ) ;
#90792 = EDGE_CURVE ( 'NONE', #5713, #7097, #118993, .T. ) ;
#90793 = EDGE_CURVE ( 'NONE', #79722, #113934, #34588, .T. ) ;
#90794 = DIRECTION ( 'NONE',  ( 0.000000000000000000, -0.000000000000000000, 1.000000000000000000 ) ) ;
#90795 = VERTEX_POINT ( 'NONE', #6358 ) ;
#90796 = ORIENTED_EDGE ( 'NONE', *, *, #33947, .T. ) ;
#90797 = VERTEX_POINT ( 'NONE', #73845 ) ;
#90798 = ORIENTED_EDGE ( 'NONE', *, *, #2323, .T. ) ;
#90799 = ORIENTED_EDGE ( 'NONE', *, *, #90143, .T. ) ;
#90800 = DIRECTION ( 'NONE',  ( 0.000000000000000000, 0.000000000000000000, 1.000000000000000000 ) ) ;
#90801 = CARTESIAN_POINT ( 'NONE',  ( -10.45000000000000107, 12.50000000000000000, 6.495190528383297135 ) ) ;
#90802 = EDGE_LOOP ( 'NONE', ( #124537, #18208, #24334, #116472 ) ) ;
#90803 = FACE_BOUND ( 'NONE', #113530, .T. ) ;
#90804 = CARTESIAN_POINT ( 'NONE',  ( -3.550000000000028244, 2.500000000000000000, 2.511473670974873507 ) ) ;
#90805 = CIRCLE ( 'NONE', #34398, 0.06509327318403745899 ) ;
#90806 = CIRCLE ( 'NONE', #3081, 0.09999999999999982514 ) ;
#90808 = ORIENTED_EDGE ( 'NONE', *, *, #13371, .T. ) ;
#90807 = CIRCLE ( 'NONE', #65665, 0.06509327318403745899 ) ;
#90809 = CARTESIAN_POINT ( 'NONE',  ( -8.350000000000012079, 12.50000000000000000, -2.792790559304616504 ) ) ;
#90810 = LINE ( 'NONE', #71824, #103750 ) ;
#90811 = CARTESIAN_POINT ( 'NONE',  ( 9.199999999999919353, 2.500000000000000000, 0.09999999999999772959 ) ) ;
#90812 = CARTESIAN_POINT ( 'NONE',  ( -11.84999999999999787, 12.50000000000000000, -1.883746621131359378 ) ) ;
#90813 = ORIENTED_EDGE ( 'NONE', *, *, #6966, .T. ) ;
#90814 = DIRECTION ( 'NONE',  ( 0.000000000000000000, 0.000000000000000000, -1.000000000000000000 ) ) ;
#90815 = CONICAL_SURFACE ( 'NONE', #53179, 0.1000000000000002554, 0.003490658503988666988 ) ;
#90816 = AXIS2_PLACEMENT_3D ( 'NONE', #50298, #108568, #9727 ) ;
#90817 = VECTOR ( 'NONE', #34386, 1000.000000000000000 ) ;
#90818 = ORIENTED_EDGE ( 'NONE', *, *, #68426, .F. ) ;
#90819 = ORIENTED_EDGE ( 'NONE', *, *, #42020, .F. ) ;
#90820 = FACE_OUTER_BOUND ( 'NONE', #101367, .T. ) ;
#90821 = PLANE ( 'NONE',  #47731 ) ;
#90822 = VERTEX_POINT ( 'NONE', #56124 ) ;
#90823 = CARTESIAN_POINT ( 'NONE',  ( 11.24999999999990763, 2.500000000000000000, -7.188010851410854052 ) ) ;
#90824 = CIRCLE ( 'NONE', #61600, 0.09999999999999982514 ) ;
#90825 = CARTESIAN_POINT ( 'NONE',  ( -7.300000000000018474, 12.50000000000000000, 0.3464101615137735735 ) ) ;
#90826 = FACE_OUTER_BOUND ( 'NONE', #83946, .T. ) ;
#90827 = CARTESIAN_POINT ( 'NONE',  ( 1.649999999999949729, 12.50000000000000000, 7.188010851410848723 ) ) ;
#90829 = ORIENTED_EDGE ( 'NONE', *, *, #116484, .F. ) ;
#90828 = CIRCLE ( 'NONE', #34420, 0.06509327318403745899 ) ;
#90830 = DIRECTION ( 'NONE',  ( -0.000000000000000000, -1.000000000000000000, -0.000000000000000000 ) ) ;
#90831 = EDGE_CURVE ( 'NONE', #36682, #1853, #108529, .T. ) ;
#90832 = EDGE_LOOP ( 'NONE', ( #65197, #104397, #4344, #2316 ) ) ;
#90833 = DIRECTION ( 'NONE',  ( 0.000000000000000000, -0.000000000000000000, 1.000000000000000000 ) ) ;
#90834 = EDGE_CURVE ( 'NONE', #21997, #25459, #52109, .T. ) ;
#90835 = ORIENTED_EDGE ( 'NONE', *, *, #127160, .T. ) ;
#90837 = EDGE_CURVE ( 'NONE', #39963, #73967, #75087, .T. ) ;
#90836 = CARTESIAN_POINT ( 'NONE',  ( 10.44999999999991402, 12.50000000000000000, -2.165063509461101710 ) ) ;
#90838 = VERTEX_POINT ( 'NONE', #54832 ) ;
#90839 = CARTESIAN_POINT ( 'NONE',  ( -8.350000000000013856, 2.500000000000000000, -2.265063509461101798 ) ) ;
#90840 = DIRECTION ( 'NONE',  ( 0.000000000000000000, 0.000000000000000000, -1.000000000000000000 ) ) ;
#90841 = CARTESIAN_POINT ( 'NONE',  ( -10.85000000000000142, 12.50000000000000000, 2.165063509461097713 ) ) ;
#90842 = DIRECTION ( 'NONE',  ( 0.000000000000000000, 1.000000000000000000, 0.000000000000000000 ) ) ;
#90843 = DIRECTION ( 'NONE',  ( -0.000000000000000000, 1.000000000000000000, -0.000000000000000000 ) ) ;
#90844 = CIRCLE ( 'NONE', #55340, 0.1000000000000000056 ) ;
#90845 = VERTEX_POINT ( 'NONE', #96056 ) ;
#90846 = EDGE_CURVE ( 'NONE', #83004, #76936, #129491, .T. ) ;
#90847 = ORIENTED_EDGE ( 'NONE', *, *, #56479, .F. ) ;
#90848 = ORIENTED_EDGE ( 'NONE', *, *, #72536, .T. ) ;
#90849 = DIRECTION ( 'NONE',  ( 0.000000000000000000, 0.000000000000000000, 1.000000000000000000 ) ) ;
#90850 = DIRECTION ( 'NONE',  ( 0.000000000000000000, 1.000000000000000000, 0.000000000000000000 ) ) ;
#90851 = CARTESIAN_POINT ( 'NONE',  ( -8.550000000000013145, 2.500000000000000000, -1.818653347947326138 ) ) ;
#90853 = ORIENTED_EDGE ( 'NONE', *, *, #75879, .T. ) ;
#90852 = ORIENTED_EDGE ( 'NONE', *, *, #26067, .F. ) ;
#90854 = VERTEX_POINT ( 'NONE', #12021 ) ;
#90855 = CARTESIAN_POINT ( 'NONE',  ( 5.449999999999936229, 2.500000000000000000, -2.165063509461101710 ) ) ;
#90856 = CIRCLE ( 'NONE', #59500, 0.1000000000000002554 ) ;
#90857 = ORIENTED_EDGE ( 'NONE', *, *, #9592, .F. ) ;
#90858 = CARTESIAN_POINT ( 'NONE',  ( 13.54999999999989768, 2.500000000000000000, -2.511473670974877948 ) ) ;
#90859 = CARTESIAN_POINT ( 'NONE',  ( 5.199999999999935341, 2.500000000000000000, -3.883716857408426648 ) ) ;
#90860 = FACE_OUTER_BOUND ( 'NONE', #23288, .T. ) ;
#90861 = DIRECTION ( 'NONE',  ( 0.000000000000000000, 0.000000000000000000, -1.000000000000000000 ) ) ;
#90862 = FACE_OUTER_BOUND ( 'NONE', #4374, .T. ) ;
#90863 = CARTESIAN_POINT ( 'NONE',  ( 9.999999999999912959, 12.50000000000000000, 3.702399969078682407 ) ) ;
#90864 = CARTESIAN_POINT ( 'NONE',  ( -2.300000000000033129, 2.500000000000000000, 3.883716857408420431 ) ) ;
#90865 = EDGE_CURVE ( 'NONE', #129208, #81079, #69661, .T. ) ;
#90866 = DIRECTION ( 'NONE',  ( 0.000000000000000000, 1.000000000000000000, 0.000000000000000000 ) ) ;
#90867 = VERTEX_POINT ( 'NONE', #70315 ) ;
#90868 = CIRCLE ( 'NONE', #59600, 0.09999999999999999167 ) ;
#90869 = DIRECTION ( 'NONE',  ( 0.000000000000000000, -0.000000000000000000, 1.000000000000000000 ) ) ;
#90871 = AXIS2_PLACEMENT_3D ( 'NONE', #34801, #114618, #96257 ) ;
#90870 = CARTESIAN_POINT ( 'NONE',  ( 5.199999999999933564, 12.50000000000000000, 0.3464101615137735735 ) ) ;
#90872 = ORIENTED_EDGE ( 'NONE', *, *, #73394, .T. ) ;
#90873 = VERTEX_POINT ( 'NONE', #110234 ) ;
#90874 = CARTESIAN_POINT ( 'NONE',  ( 185.0260416670080588, -6.551208109652273848, -3.782341765625003571 ) ) ;
#90875 = DIRECTION ( 'NONE',  ( -0.000000000000000000, 1.000000000000000000, -0.000000000000000000 ) ) ;
#90876 = FACE_OUTER_BOUND ( 'NONE', #14477, .T. ) ;
#90877 = LINE ( 'NONE', #41162, #30391 ) ;
#90878 = CARTESIAN_POINT ( 'NONE',  ( -10.45000000000000462, 12.50000000000000000, -2.165063509461097713 ) ) ;
#90879 = CONICAL_SURFACE ( 'NONE', #86669, 0.1000000000000000472, 0.003490658503988666988 ) ;
#90880 = LINE ( 'NONE', #69290, #19798 ) ;
#90881 = AXIS2_PLACEMENT_3D ( 'NONE', #85499, #86117, #55397 ) ;
#90882 = EDGE_CURVE ( 'NONE', #5168, #116825, #12382, .T. ) ;
#90883 = FACE_OUTER_BOUND ( 'NONE', #63308, .T. ) ;
#90884 = CARTESIAN_POINT ( 'NONE',  ( 0.6499999999999561684, 12.50000000000000000, 2.576566944158910744 ) ) ;
#90885 = AXIS2_PLACEMENT_3D ( 'NONE', #7243, #107396, #46532 ) ;
#90886 = AXIS2_PLACEMENT_3D ( 'NONE', #31714, #21236, #42851 ) ;
#90887 = PLANE ( 'NONE',  #29133 ) ;
#90888 = VERTEX_POINT ( 'NONE', #40213 ) ;
#90889 = EDGE_LOOP ( 'NONE', ( #115544, #87280, #50641, #66089 ) ) ;
#90890 = EDGE_LOOP ( 'NONE', ( #2343, #101617, #86371, #91290 ) ) ;
#90891 = ORIENTED_EDGE ( 'NONE', *, *, #53050, .T. ) ;
#90893 = ORIENTED_EDGE ( 'NONE', *, *, #112042, .T. ) ;
#90892 = EDGE_CURVE ( 'NONE', #11640, #87436, #14520, .T. ) ;
#90894 = CARTESIAN_POINT ( 'NONE',  ( 10.84999999999990905, 12.50000000000000000, 2.857883832488649301 ) ) ;
#90895 = CARTESIAN_POINT ( 'NONE',  ( -4.150000000000028777, 2.500000000000000000, -5.802370205355749988 ) ) ;
#90896 = ORIENTED_EDGE ( 'NONE', *, *, #45744, .F. ) ;
#90897 = PLANE ( 'NONE',  #75778 ) ;
#90898 = CARTESIAN_POINT ( 'NONE',  ( 186.1979166673494603, 6.668395609140176816, 3.850000000000000977 ) ) ;
#90899 = CONICAL_SURFACE ( 'NONE', #74179, 0.09999999999999982514, 0.003490658503988666988 ) ;
#90900 = AXIS2_PLACEMENT_3D ( 'NONE', #81553, #113593, #122766 ) ;
#90901 = FACE_OUTER_BOUND ( 'NONE', #7182, .T. ) ;
#90903 = ORIENTED_EDGE ( 'NONE', *, *, #90046, .T. ) ;
#90902 = DIRECTION ( 'NONE',  ( 0.000000000000000000, 0.000000000000000000, 1.000000000000000000 ) ) ;
#90904 = AXIS2_PLACEMENT_3D ( 'NONE', #27759, #118725, #18594 ) ;
#90905 = AXIS2_PLACEMENT_3D ( 'NONE', #96603, #67133, #56677 ) ;
#90906 = ADVANCED_FACE ( 'NONE', ( #50055 ), #125256, .T. ) ;
#90907 = DIRECTION ( 'NONE',  ( 0.000000000000000000, 0.000000000000000000, 1.000000000000000000 ) ) ;
#90908 = DIRECTION ( 'NONE',  ( 0.000000000000000000, 1.000000000000000000, 0.000000000000000000 ) ) ;
#90909 = ORIENTED_EDGE ( 'NONE', *, *, #109264, .F. ) ;
#90910 = AXIS2_PLACEMENT_3D ( 'NONE', #62390, #102313, #52554 ) ;
#90911 = AXIS2_PLACEMENT_3D ( 'NONE', #66033, #16897, #85024 ) ;
#90912 = AXIS2_PLACEMENT_3D ( 'NONE', #95222, #5530, #46114 ) ;
#90913 = ORIENTED_EDGE ( 'NONE', *, *, #34644, .T. ) ;
#90914 = ORIENTED_EDGE ( 'NONE', *, *, #27112, .T. ) ;
#90915 = ORIENTED_EDGE ( 'NONE', *, *, #83752, .F. ) ;
#90916 = DIRECTION ( 'NONE',  ( -0.000000000000000000, -1.000000000000000000, -0.000000000000000000 ) ) ;
#90917 = CIRCLE ( 'NONE', #5225, 0.06509327318403745899 ) ;
#90918 = DIRECTION ( 'NONE',  ( 0.000000000000000000, -0.9999939076577903929, 0.003490651415223739937 ) ) ;
#90919 = DIRECTION ( 'NONE',  ( 0.000000000000000000, 0.000000000000000000, -1.000000000000000000 ) ) ;
#90920 = AXIS2_PLACEMENT_3D ( 'NONE', #25340, #6328, #4394 ) ;
#90921 = CIRCLE ( 'NONE', #36658, 0.1000000000000000472 ) ;
#90922 = EDGE_CURVE ( 'NONE', #15358, #62185, #68821, .T. ) ;
#90924 = AXIS2_PLACEMENT_3D ( 'NONE', #5400, #105549, #96347 ) ;
#90923 = DIRECTION ( 'NONE',  ( 0.000000000000000000, 0.000000000000000000, 1.000000000000000000 ) ) ;
#90925 = ORIENTED_EDGE ( 'NONE', *, *, #64024, .F. ) ;
#90926 = CARTESIAN_POINT ( 'NONE',  ( 17.50000000000000000, 2.500000000000000000, 0.000000000000000000 ) ) ;
#90927 = DIRECTION ( 'NONE',  ( 0.000000000000000000, 0.000000000000000000, -1.000000000000000000 ) ) ;
#90928 = CARTESIAN_POINT ( 'NONE',  ( 9.149999999999916866, 2.500000000000000000, 5.902370205355745192 ) ) ;
#90929 = DIRECTION ( 'NONE',  ( -0.000000000000000000, 1.000000000000000000, -0.000000000000000000 ) ) ;
#90930 = ADVANCED_FACE ( 'NONE', ( #100418 ), #77230, .T. ) ;
#90931 = ORIENTED_EDGE ( 'NONE', *, *, #20289, .T. ) ;
#90932 = ORIENTED_EDGE ( 'NONE', *, *, #61238, .T. ) ;
#90933 = VERTEX_POINT ( 'NONE', #91239 ) ;
#90934 = DIRECTION ( 'NONE',  ( 0.000000000000000000, 0.000000000000000000, -1.000000000000000000 ) ) ;
#90935 = EDGE_CURVE ( 'NONE', #118779, #33308, #4065, .T. ) ;
#90936 = ADVANCED_FACE ( 'NONE', ( #99776 ), #87772, .T. ) ;
#90937 = DIRECTION ( 'NONE',  ( -4.274815082592931898E-19, -0.9999939076577903929, -0.003490651415223739937 ) ) ;
#90938 = EDGE_CURVE ( 'NONE', #9468, #14124, #38951, .T. ) ;
#90939 = FACE_BOUND ( 'NONE', #2699, .T. ) ;
#90940 = EDGE_CURVE ( 'NONE', #75204, #13568, #119093, .T. ) ;
#90941 = LINE ( 'NONE', #59578, #53500 ) ;
#90942 = AXIS2_PLACEMENT_3D ( 'NONE', #36893, #76813, #17876 ) ;
#90943 = FACE_OUTER_BOUND ( 'NONE', #14612, .T. ) ;
#90944 = CARTESIAN_POINT ( 'NONE',  ( -3.750000000000026201, 12.50000000000000000, 5.737276932171707422 ) ) ;
#90945 = EDGE_CURVE ( 'NONE', #24882, #28910, #64798, .T. ) ;
#90946 = CARTESIAN_POINT ( 'NONE',  ( -1.650000000000034772, 12.50000000000000000, 2.165063509461097713 ) ) ;
#90947 = EDGE_CURVE ( 'NONE', #93321, #34505, #14605, .T. ) ;
#90948 = CARTESIAN_POINT ( 'NONE',  ( 5.849999999999933920, 12.50000000000000000, -2.857883832488653741 ) ) ;
#90949 = EDGE_CURVE ( 'NONE', #79994, #33468, #10101, .T. ) ;
#90950 = CARTESIAN_POINT ( 'NONE',  ( 11.64999999999990621, 2.500000000000000000, -2.065063509461102065 ) ) ;
#90951 = EDGE_LOOP ( 'NONE', ( #91394, #110182, #36782, #19874 ) ) ;
#90952 = AXIS2_PLACEMENT_3D ( 'NONE', #113516, #21267, #23866 ) ;
#90953 = PLANE ( 'NONE',  #84626 ) ;
#90954 = EDGE_CURVE ( 'NONE', #121068, #15661, #50202, .T. ) ;
#90955 = EDGE_CURVE ( 'NONE', #120418, #72840, #35480, .T. ) ;
#90956 = DIRECTION ( 'NONE',  ( 0.000000000000000000, 0.000000000000000000, 1.000000000000000000 ) ) ;
#90957 = VERTEX_POINT ( 'NONE', #89303 ) ;
#90958 = EDGE_LOOP ( 'NONE', ( #37365, #47967 ) ) ;
#90959 = DIRECTION ( 'NONE',  ( -0.000000000000000000, -1.000000000000000000, -0.000000000000000000 ) ) ;
#90960 = FACE_OUTER_BOUND ( 'NONE', #108770, .T. ) ;
#90961 = FACE_BOUND ( 'NONE', #55083, .T. ) ;
#90962 = EDGE_CURVE ( 'NONE', #85218, #111831, #89941, .T. ) ;
#90963 = CARTESIAN_POINT ( 'NONE',  ( 14.93814514904464197, -2.499999999999999556, -6.173787961026617310 ) ) ;
#90964 = AXIS2_PLACEMENT_3D ( 'NONE', #1412, #59059, #21712 ) ;
#90965 = DIRECTION ( 'NONE',  ( -0.000000000000000000, -1.000000000000000000, -0.000000000000000000 ) ) ;
#90966 = CIRCLE ( 'NONE', #111897, 0.06509327318403745899 ) ;
#90967 = ORIENTED_EDGE ( 'NONE', *, *, #13824, .T. ) ;
#90968 = DIRECTION ( 'NONE',  ( 0.000000000000000000, 1.000000000000000000, 0.000000000000000000 ) ) ;
#90969 = CARTESIAN_POINT ( 'NONE',  ( 185.0833333333333144, -6.668395609140180369, 3.849999999999994760 ) ) ;
#90970 = ORIENTED_EDGE ( 'NONE', *, *, #6701, .T. ) ;
#90971 = CARTESIAN_POINT ( 'NONE',  ( -6.450000000000019718, 2.500000000000000000, -1.718653347947326049 ) ) ;
#90972 = DIRECTION ( 'NONE',  ( 0.000000000000000000, 1.000000000000000000, 0.000000000000000000 ) ) ;
#90973 = VECTOR ( 'NONE', #35737, 1000.000000000000000 ) ;
#90974 = CIRCLE ( 'NONE', #72110, 0.06509327318403745899 ) ;
#90975 = DIRECTION ( 'NONE',  ( 0.000000000000000000, 1.000000000000000000, 0.000000000000000000 ) ) ;
#90976 = DIRECTION ( 'NONE',  ( 0.000000000000000000, 0.000000000000000000, 1.000000000000000000 ) ) ;
#90977 = ORIENTED_EDGE ( 'NONE', *, *, #7037, .F. ) ;
#90978 = DIRECTION ( 'NONE',  ( -0.000000000000000000, 1.000000000000000000, -0.000000000000000000 ) ) ;
#90979 = DIRECTION ( 'NONE',  ( -4.274815082592931898E-19, -0.9999939076577903929, -0.003490651415223739937 ) ) ;
#90980 = CARTESIAN_POINT ( 'NONE',  ( 184.6145833340161175, 6.668395609140177704, -3.849999999999998312 ) ) ;
#90981 = ORIENTED_EDGE ( 'NONE', *, *, #48853, .F. ) ;
#90982 = EDGE_LOOP ( 'NONE', ( #74157, #112968, #23308, #39268 ) ) ;
#90983 = CARTESIAN_POINT ( 'NONE',  ( 4.149999999999941735, 2.500000000000000000, -5.802370205355749988 ) ) ;
#90984 = AXIS2_PLACEMENT_3D ( 'NONE', #104688, #23565, #103422 ) ;
#90985 = ORIENTED_EDGE ( 'NONE', *, *, #96126, .T. ) ;
#90986 = DIRECTION ( 'NONE',  ( 0.000000000000000000, 1.000000000000000000, 0.000000000000000000 ) ) ;
#90987 = DIRECTION ( 'NONE',  ( 0.000000000000000000, 0.000000000000000000, 1.000000000000000000 ) ) ;
#90988 = ADVANCED_FACE ( 'NONE', ( #61795 ), #129261, .T. ) ;
#90990 = DIRECTION ( 'NONE',  ( 0.000000000000000000, 1.000000000000000000, 0.000000000000000000 ) ) ;
#90989 = AXIS2_PLACEMENT_3D ( 'NONE', #317, #51403, #20641 ) ;
#90991 = ORIENTED_EDGE ( 'NONE', *, *, #126862, .F. ) ;
#90992 = CONICAL_SURFACE ( 'NONE', #9431, 0.09999999999999982514, 0.003490658503988666988 ) ;
#90994 = EDGE_CURVE ( 'NONE', #125586, #118617, #27150, .T. ) ;
#90993 = DIRECTION ( 'NONE',  ( 0.000000000000000000, 1.000000000000000000, 0.000000000000000000 ) ) ;
#90995 = DIRECTION ( 'NONE',  ( 0.000000000000000000, -0.9999939076577903929, 0.003490651415223739937 ) ) ;
#90996 = CARTESIAN_POINT ( 'NONE',  ( 9.599999999999914380, 2.500000000000000000, -3.537306695894649966 ) ) ;
#90997 = AXIS2_PLACEMENT_3D ( 'NONE', #66836, #76027, #106764 ) ;
#90998 = LINE ( 'NONE', #41911, #3571 ) ;
#90999 = CARTESIAN_POINT ( 'NONE',  ( 2.499999999999947153, 2.500000000000000000, -3.637306695894650055 ) ) ;
#91000 = CARTESIAN_POINT ( 'NONE',  ( -11.25000000000000000, 2.500000000000000000, 7.188010851410848723 ) ) ;
#91001 = EDGE_CURVE ( 'NONE', #22620, #67345, #43894, .T. ) ;
#91002 = ORIENTED_EDGE ( 'NONE', *, *, #34707, .T. ) ;
#91004 = ORIENTED_EDGE ( 'NONE', *, *, #43010, .T. ) ;
#91003 = CIRCLE ( 'NONE', #17833, 0.06509327318403745899 ) ;
#91006 = FACE_OUTER_BOUND ( 'NONE', #124364, .T. ) ;
#91005 = AXIS2_PLACEMENT_3D ( 'NONE', #13908, #63680, #125789 ) ;
#91007 = ORIENTED_EDGE ( 'NONE', *, *, #59248, .F. ) ;
#91008 = DIRECTION ( 'NONE',  ( 0.000000000000000000, 0.000000000000000000, -1.000000000000000000 ) ) ;
#91011 = ORIENTED_EDGE ( 'NONE', *, *, #110709, .F. ) ;
#91010 = VERTEX_POINT ( 'NONE', #63066 ) ;
#91009 = AXIS2_PLACEMENT_3D ( 'NONE', #105060, #15382, #125992 ) ;
#91012 = VERTEX_POINT ( 'NONE', #121995 ) ;
#91013 = DIRECTION ( 'NONE',  ( -0.000000000000000000, 1.000000000000000000, -0.000000000000000000 ) ) ;
#91014 = ADVANCED_FACE ( 'NONE', ( #22522 ), #110757, .T. ) ;
#91015 = AXIS2_PLACEMENT_3D ( 'NONE', #122130, #1684, #388 ) ;
#91017 = AXIS2_PLACEMENT_3D ( 'NONE', #59780, #61036, #99689 ) ;
#91016 = CARTESIAN_POINT ( 'NONE',  ( -3.350000000000028511, 2.500000000000000000, 2.857883832488649301 ) ) ;
#91018 = CARTESIAN_POINT ( 'NONE',  ( 3.949999999999939782, 2.500000000000000000, 2.511473670974873507 ) ) ;
#91019 = VECTOR ( 'NONE', #61061, 1000.000000000000000 ) ;
#91020 = FACE_OUTER_BOUND ( 'NONE', #104329, .T. ) ;
#91021 = DIRECTION ( 'NONE',  ( 0.000000000000000000, -0.000000000000000000, -1.000000000000000000 ) ) ;
#91022 = CARTESIAN_POINT ( 'NONE',  ( 3.349999999999944578, 2.500000000000000000, -5.802370205355749988 ) ) ;
#91023 = CIRCLE ( 'NONE', #65970, 0.1000000000000002554 ) ;
#91024 = CARTESIAN_POINT ( 'NONE',  ( -13.94999999999998863, 12.50000000000000000, -1.818653347947323917 ) ) ;
#91025 = DIRECTION ( 'NONE',  ( -4.274815082592931898E-19, -0.9999939076577903929, -0.003490651415223739937 ) ) ;
#91026 = DIRECTION ( 'NONE',  ( -4.274815082592931898E-19, -0.9999939076577903929, -0.003490651415223739937 ) ) ;
#91027 = ORIENTED_EDGE ( 'NONE', *, *, #40306, .F. ) ;
#91028 = CARTESIAN_POINT ( 'NONE',  ( -4.150000000000027889, 2.500000000000000000, -6.495190528383302464 ) ) ;
#91029 = ORIENTED_EDGE ( 'NONE', *, *, #111780, .T. ) ;
#91030 = ORIENTED_EDGE ( 'NONE', *, *, #66726, .T. ) ;
#91031 = DIRECTION ( 'NONE',  ( 0.000000000000000000, 0.000000000000000000, 1.000000000000000000 ) ) ;
#91032 = VECTOR ( 'NONE', #98858, 1000.000000000000000 ) ;
#91033 = DIRECTION ( 'NONE',  ( 0.000000000000000000, 0.000000000000000000, 1.000000000000000000 ) ) ;
#91034 = ADVANCED_FACE ( 'NONE', ( #43448 ), #10421, .T. ) ;
#91035 = LINE ( 'NONE', #98918, #60881 ) ;
#91036 = DIRECTION ( 'NONE',  ( 0.000000000000000000, 1.000000000000000000, 0.000000000000000000 ) ) ;
#91037 = DIRECTION ( 'NONE',  ( 0.000000000000000000, 0.000000000000000000, -1.000000000000000000 ) ) ;
#91038 = DIRECTION ( 'NONE',  ( -0.000000000000000000, 1.000000000000000000, -0.000000000000000000 ) ) ;
#91039 = ORIENTED_EDGE ( 'NONE', *, *, #111840, .T. ) ;
#91040 = CIRCLE ( 'NONE', #80585, 0.06509327318403745899 ) ;
#91041 = EDGE_CURVE ( 'NONE', #63523, #61895, #60620, .T. ) ;
#91042 = VECTOR ( 'NONE', #87272, 1000.000000000000000 ) ;
#91043 = CONICAL_SURFACE ( 'NONE', #68050, 0.09999999999999999167, 0.003490658503988666988 ) ;
#91044 = ORIENTED_EDGE ( 'NONE', *, *, #55092, .F. ) ;
#91045 = VERTEX_POINT ( 'NONE', #94445 ) ;
#91046 = CARTESIAN_POINT ( 'NONE',  ( 186.3750000000000000, 8.891194145520236347, 5.444286225454521982E-16 ) ) ;
#91047 = EDGE_LOOP ( 'NONE', ( #64596, #62205, #5726, #98618 ) ) ;
#91048 = EDGE_CURVE ( 'NONE', #53990, #4275, #50152, .T. ) ;
#91049 = ORIENTED_EDGE ( 'NONE', *, *, #112351, .F. ) ;
#91050 = LINE ( 'NONE', #12481, #29403 ) ;
#91051 = DIRECTION ( 'NONE',  ( -0.000000000000000000, 1.000000000000000000, -0.000000000000000000 ) ) ;
#91052 = AXIS2_PLACEMENT_3D ( 'NONE', #125061, #15068, #47152 ) ;
#91053 = DIRECTION ( 'NONE',  ( 0.000000000000000000, 1.000000000000000000, 0.000000000000000000 ) ) ;
#91054 = DIRECTION ( 'NONE',  ( 0.000000000000000000, 1.000000000000000000, 0.000000000000000000 ) ) ;
#91055 = CARTESIAN_POINT ( 'NONE',  ( 87.50000000000001421, -2.781865847474095155, 7.000342182495693066 ) ) ;
#91056 = ORIENTED_EDGE ( 'NONE', *, *, #4997, .T. ) ;
#91057 = DIRECTION ( 'NONE',  ( 0.000000000000000000, -0.000000000000000000, 1.000000000000000000 ) ) ;
#91058 = LINE ( 'NONE', #1376, #93343 ) ;
#91059 = EDGE_CURVE ( 'NONE', #100810, #38970, #8265, .T. ) ;
#91060 = CARTESIAN_POINT ( 'NONE',  ( -7.100000000000018296, 2.500000000000000000, -4.430127018922202176 ) ) ;
#91061 = FACE_OUTER_BOUND ( 'NONE', #78062, .T. ) ;
#91062 = DIRECTION ( 'NONE',  ( 0.000000000000000000, 0.000000000000000000, 1.000000000000000000 ) ) ;
#91063 = ORIENTED_EDGE ( 'NONE', *, *, #74650, .T. ) ;
#91064 = AXIS2_PLACEMENT_3D ( 'NONE', #94482, #5458, #124610 ) ;
#91065 = CIRCLE ( 'NONE', #55475, 0.1000000000000002554 ) ;
#91066 = EDGE_LOOP ( 'NONE', ( #12830, #73888, #103109, #2152 ) ) ;
#91067 = ORIENTED_EDGE ( 'NONE', *, *, #29059, .T. ) ;
#91068 = DIRECTION ( 'NONE',  ( 0.000000000000000000, 0.000000000000000000, -1.000000000000000000 ) ) ;
#91069 = ORIENTED_EDGE ( 'NONE', *, *, #122653, .F. ) ;
#91070 = CARTESIAN_POINT ( 'NONE',  ( -0.8500000000000386136, 2.500000000000000000, 1.372243186433545370 ) ) ;
#91071 = FACE_OUTER_BOUND ( 'NONE', #103175, .T. ) ;
#91072 = ORIENTED_EDGE ( 'NONE', *, *, #105325, .F. ) ;
#91073 = CARTESIAN_POINT ( 'NONE',  ( 12.29999999999990656, 2.500000000000000000, -4.676537180435977881 ) ) ;
#91074 = DIRECTION ( 'NONE',  ( -0.000000000000000000, 1.000000000000000000, -0.000000000000000000 ) ) ;
#91075 = DIRECTION ( 'NONE',  ( 0.000000000000000000, 0.000000000000000000, 1.000000000000000000 ) ) ;
#91076 = AXIS2_PLACEMENT_3D ( 'NONE', #70580, #1192, #60142 ) ;
#91077 = DIRECTION ( 'NONE',  ( 0.000000000000000000, 1.000000000000000000, 0.000000000000000000 ) ) ;
#91078 = EDGE_CURVE ( 'NONE', #122576, #82140, #123293, .T. ) ;
#91079 = AXIS2_PLACEMENT_3D ( 'NONE', #4833, #73579, #45434 ) ;
#91080 = CARTESIAN_POINT ( 'NONE',  ( 2.499999999999983569, 12.50000000000000000, -2.276824562219559311E-15 ) ) ;
#91081 = CIRCLE ( 'NONE', #109877, 0.1000000000000000056 ) ;
#91082 = ORIENTED_EDGE ( 'NONE', *, *, #110575, .F. ) ;
#91083 =( BOUNDED_CURVE ( )  B_SPLINE_CURVE ( 2, ( #56259, #126299, #47108, #28096, #27433, #58222, #36649 ),
 .UNSPECIFIED., .F., .F. ) 
 B_SPLINE_CURVE_WITH_KNOTS ( ( 3, 2, 2, 3 ),
 ( 0.6428571428571433488, 0.6666666666666670737, 0.6904761904761910207, 0.7142857142857148567 ),
 .UNSPECIFIED. ) 
 CURVE ( )  GEOMETRIC_REPRESENTATION_ITEM ( )  RATIONAL_B_SPLINE_CURVE ( ( 0.9999999999999974465, 0.8660254037844412611, 1.000000000000000000, 0.8660254037844387076, 1.000000000000000000, 0.8660254037844355990, 1.000000000000003109 ) ) 
 REPRESENTATION_ITEM ( '' )  );
#91084 = ORIENTED_EDGE ( 'NONE', *, *, #94784, .F. ) ;
#91085 = ADVANCED_FACE ( 'NONE', ( #91886 ), #72260, .T. ) ;
#91086 = CARTESIAN_POINT ( 'NONE',  ( 65.34957883054167382, 3.515385111700535692, -5.621992225044548874 ) ) ;
#91087 = CARTESIAN_POINT ( 'NONE',  ( 6.649999999999929301, 2.500000000000000000, 6.495190528383297135 ) ) ;
#91088 = EDGE_CURVE ( 'NONE', #84285, #111183, #81445, .T. ) ;
#91089 = DIRECTION ( 'NONE',  ( 0.000000000000000000, 1.000000000000000000, 0.000000000000000000 ) ) ;
#91090 = DIRECTION ( 'NONE',  ( 0.000000000000000000, 0.000000000000000000, -1.000000000000000000 ) ) ;
#91091 = VERTEX_POINT ( 'NONE', #33613 ) ;
#91092 = ADVANCED_FACE ( 'NONE', ( #3506 ), #127504, .T. ) ;
#91093 = CONICAL_SURFACE ( 'NONE', #40955, 0.1000000000000000472, 0.003490658503988666988 ) ;
#91094 = ADVANCED_FACE ( 'NONE', ( #112819 ), #77322, .T. ) ;
#91095 = ORIENTED_EDGE ( 'NONE', *, *, #120447, .F. ) ;
#91096 = CARTESIAN_POINT ( 'NONE',  ( 1.449999999999951328, 2.500000000000000000, -1.918653347947326004 ) ) ;
#91097 = DIRECTION ( 'NONE',  ( 0.000000000000000000, 1.000000000000000000, 0.000000000000000000 ) ) ;
#91098 = ADVANCED_FACE ( 'NONE', ( #92521 ), #71067, .T. ) ;
#91099 = DIRECTION ( 'NONE',  ( 0.000000000000000000, -0.000000000000000000, 1.000000000000000000 ) ) ;
#91100 = ORIENTED_EDGE ( 'NONE', *, *, #15376, .T. ) ;
#91101 = CIRCLE ( 'NONE', #11678, 2.000000000000000000 ) ;
#91102 = AXIS2_PLACEMENT_3D ( 'NONE', #79879, #20320, #77942 ) ;
#91103 = DIRECTION ( 'NONE',  ( -4.274815082592931898E-19, -0.9999939076577903929, -0.003490651415223739937 ) ) ;
#91104 = CIRCLE ( 'NONE', #51329, 0.1000000000000000472 ) ;
#91105 = EDGE_CURVE ( 'NONE', #97111, #108779, #79387, .T. ) ;
#91106 = DIRECTION ( 'NONE',  ( -0.000000000000000000, -1.000000000000000000, -0.000000000000000000 ) ) ;
#91107 = AXIS2_PLACEMENT_3D ( 'NONE', #37305, #117118, #127608 ) ;
#91108 = VERTEX_POINT ( 'NONE', #59660 ) ;
#91109 = DIRECTION ( 'NONE',  ( -4.274815082592931898E-19, -0.9999939076577903929, -0.003490651415223739937 ) ) ;
#91110 = EDGE_LOOP ( 'NONE', ( #97320, #97348 ) ) ;
#91111 = ADVANCED_FACE ( 'NONE', ( #2618 ), #109363, .T. ) ;
#91112 = DIRECTION ( 'NONE',  ( 0.000000000000000000, 0.000000000000000000, 1.000000000000000000 ) ) ;
#91113 = ORIENTED_EDGE ( 'NONE', *, *, #9857, .T. ) ;
#91114 = ORIENTED_EDGE ( 'NONE', *, *, #65092, .T. ) ;
#91115 = DIRECTION ( 'NONE',  ( 0.000000000000000000, 0.000000000000000000, 1.000000000000000000 ) ) ;
#91116 = CARTESIAN_POINT ( 'NONE',  ( -3.950000000000028155, 2.500000000000000000, -6.741600689897077281 ) ) ;
#91117 = EDGE_LOOP ( 'NONE', ( #109377, #47099 ) ) ;
#91118 = ORIENTED_EDGE ( 'NONE', *, *, #9785, .F. ) ;
#91119 = DIRECTION ( 'NONE',  ( 0.000000000000000000, -0.000000000000000000, 1.000000000000000000 ) ) ;
#91120 = DIRECTION ( 'NONE',  ( 0.000000000000000000, 0.000000000000000000, 1.000000000000000000 ) ) ;
#91121 = AXIS2_PLACEMENT_3D ( 'NONE', #65377, #126244, #76504 ) ;
#91122 = EDGE_LOOP ( 'NONE', ( #5471, #14026, #102876, #12499 ) ) ;
#91123 = CARTESIAN_POINT ( 'NONE',  ( 186.8802083336747444, 4.367472073101515306, 7.564683531250000925 ) ) ;
#91124 = CARTESIAN_POINT ( 'NONE',  ( 184.6927083336747160, 6.551208109652275624, -3.782341765624998686 ) ) ;
#91125 = CARTESIAN_POINT ( 'NONE',  ( 11.89999999999990798, 2.500000000000000000, 3.883716857408421319 ) ) ;
#91126 = DIRECTION ( 'NONE',  ( -0.000000000000000000, -1.000000000000000000, -0.000000000000000000 ) ) ;
#91127 = FACE_OUTER_BOUND ( 'NONE', #96446, .T. ) ;
#91128 = DIRECTION ( 'NONE',  ( -0.000000000000000000, 1.000000000000000000, -0.000000000000000000 ) ) ;
#91129 = CARTESIAN_POINT ( 'NONE',  ( -10.20000000000000462, 2.500000000000000000, 4.776537180435972196 ) ) ;
#91130 = CIRCLE ( 'NONE', #109923, 0.06509327318403745899 ) ;
#91131 = AXIS2_PLACEMENT_3D ( 'NONE', #15924, #95152, #55859 ) ;
#91132 = ORIENTED_EDGE ( 'NONE', *, *, #112791, .F. ) ;
#91133 = AXIS2_PLACEMENT_3D ( 'NONE', #7219, #86436, #126375 ) ;
#91134 = VERTEX_POINT ( 'NONE', #100818 ) ;
#91135 = DIRECTION ( 'NONE',  ( 0.000000000000000000, 1.000000000000000000, 0.000000000000000000 ) ) ;
#91136 = ORIENTED_EDGE ( 'NONE', *, *, #44884, .F. ) ;
#91137 = CARTESIAN_POINT ( 'NONE',  ( -9.150000000000009237, 12.50000000000000000, 2.792790559304612064 ) ) ;
#91138 = LINE ( 'NONE', #89840, #99358 ) ;
#91139 = CARTESIAN_POINT ( 'NONE',  ( 6.049999999999932321, 12.50000000000000000, 6.841600689897072485 ) ) ;
#91141 = EDGE_LOOP ( 'NONE', ( #66329, #54359 ) ) ;
#91140 = EDGE_LOOP ( 'NONE', ( #49582, #82033, #91162, #7621 ) ) ;
#91142 = FACE_BOUND ( 'NONE', #103574, .T. ) ;
#91143 = ORIENTED_EDGE ( 'NONE', *, *, #6487, .T. ) ;
#91144 = DIRECTION ( 'NONE',  ( -0.000000000000000000, 1.000000000000000000, -0.000000000000000000 ) ) ;
#91145 = CARTESIAN_POINT ( 'NONE',  ( -9.150000000000005684, 12.50000000000000000, 7.188010851410848723 ) ) ;
#91146 = VECTOR ( 'NONE', #57466, 1000.000000000000000 ) ;
#91147 = CARTESIAN_POINT ( 'NONE',  ( -3.350000000000028511, 2.500000000000000000, -1.572243186433550211 ) ) ;
#91148 = LINE ( 'NONE', #62973, #80698 ) ;
#91149 = EDGE_CURVE ( 'NONE', #39568, #18587, #70096, .T. ) ;
#91150 = DIRECTION ( 'NONE',  ( 0.000000000000000000, 0.000000000000000000, -1.000000000000000000 ) ) ;
#91152 = AXIS2_PLACEMENT_3D ( 'NONE', #93094, #81337, #4043 ) ;
#91151 = AXIS2_PLACEMENT_3D ( 'NONE', #92952, #124978, #47715 ) ;
#91153 = CARTESIAN_POINT ( 'NONE',  ( 187.5000000000000000, 0.000000000000000000, 8.699999999999999289 ) ) ;
#91154 = DIRECTION ( 'NONE',  ( 0.000000000000000000, 0.000000000000000000, -1.000000000000000000 ) ) ;
#91155 = DIRECTION ( 'NONE',  ( 0.000000000000000000, 0.000000000000000000, 1.000000000000000000 ) ) ;
#91156 = CARTESIAN_POINT ( 'NONE',  ( -3.100000000000028511, 2.500000000000000000, -0.3464101615137782364 ) ) ;
#91157 = CARTESIAN_POINT ( 'NONE',  ( 11.64999999999990443, 2.500000000000000000, 1.372243186433545370 ) ) ;
#91158 = CARTESIAN_POINT ( 'NONE',  ( -8.350000000000010303, 2.500000000000000000, 6.395190528383296602 ) ) ;
#91159 = EDGE_CURVE ( 'NONE', #30305, #20100, #100199, .T. ) ;
#91160 = EDGE_LOOP ( 'NONE', ( #125286, #68288, #117207, #121409 ) ) ;
#91161 = ORIENTED_EDGE ( 'NONE', *, *, #67516, .T. ) ;
#91162 = ORIENTED_EDGE ( 'NONE', *, *, #119224, .T. ) ;
#91163 = ORIENTED_EDGE ( 'NONE', *, *, #39284, .F. ) ;
#91164 = CARTESIAN_POINT ( 'NONE',  ( -1.250000000000037526, 12.50000000000000000, -5.867463478539787225 ) ) ;
#91165 = CARTESIAN_POINT ( 'NONE',  ( 6.449999999999930012, 12.50000000000000000, 1.818653347947321475 ) ) ;
#91167 = ORIENTED_EDGE ( 'NONE', *, *, #26814, .T. ) ;
#91166 = EDGE_LOOP ( 'NONE', ( #96114, #93301, #16465, #109955 ) ) ;
#91168 = ORIENTED_EDGE ( 'NONE', *, *, #113089, .T. ) ;
#91169 = CARTESIAN_POINT ( 'NONE',  ( 9.799999999999913669, 12.50000000000000000, -3.983716857408426293 ) ) ;
#91170 = DIRECTION ( 'NONE',  ( -0.000000000000000000, -1.000000000000000000, -0.000000000000000000 ) ) ;
#91171 = CARTESIAN_POINT ( 'NONE',  ( 187.2812500006828031, 0.000000000000000000, 7.700000000000000178 ) ) ;
#91172 = DIRECTION ( 'NONE',  ( 0.000000000000000000, 0.000000000000000000, 1.000000000000000000 ) ) ;
#91173 = DIRECTION ( 'NONE',  ( 0.000000000000000000, 0.000000000000000000, -1.000000000000000000 ) ) ;
#91174 = DIRECTION ( 'NONE',  ( 0.000000000000000000, -0.000000000000000000, 1.000000000000000000 ) ) ;
#91175 = CARTESIAN_POINT ( 'NONE',  ( -11.69999999999999929, 2.500000000000000000, -4.330127018922198978 ) ) ;
#91176 = ORIENTED_EDGE ( 'NONE', *, *, #30600, .T. ) ;
#91177 = DIRECTION ( 'NONE',  ( 0.000000000000000000, 0.000000000000000000, -1.000000000000000000 ) ) ;
#91178 = VERTEX_POINT ( 'NONE', #19705 ) ;
#91180 = ORIENTED_EDGE ( 'NONE', *, *, #90614, .F. ) ;
#91179 = AXIS2_PLACEMENT_3D ( 'NONE', #123819, #125744, #34181 ) ;
#91181 = ORIENTED_EDGE ( 'NONE', *, *, #490, .T. ) ;
#91182 = CONICAL_SURFACE ( 'NONE', #97428, 0.09999999999999982514, 0.003490658503988666988 ) ;
#91183 = CARTESIAN_POINT ( 'NONE',  ( -10.20000000000000284, 12.50000000000000000, -0.3464101615137782364 ) ) ;
#91184 = ORIENTED_EDGE ( 'NONE', *, *, #86363, .F. ) ;
#91185 = EDGE_LOOP ( 'NONE', ( #28321, #102703, #75860, #20648 ) ) ;
#91186 = VERTEX_POINT ( 'NONE', #111959 ) ;
#91188 = CONICAL_SURFACE ( 'NONE', #36821, 0.1000000000000002554, 0.003490658503988666988 ) ;
#91187 = CONICAL_SURFACE ( 'NONE', #24569, 0.09999999999999999167, 0.003490658503988666988 ) ;
#91189 = ADVANCED_FACE ( 'NONE', ( #32116 ), #51744, .T. ) ;
#91190 = SURFACE_STYLE_FILL_AREA ( #41470 ) ;
#91191 = DIRECTION ( 'NONE',  ( 0.000000000000000000, 0.000000000000000000, 1.000000000000000000 ) ) ;
#91192 = CARTESIAN_POINT ( 'NONE',  ( 12.49999999999990585, 2.500000000000000000, -4.922947341949753586 ) ) ;
#91193 = CARTESIAN_POINT ( 'NONE',  ( -12.49999999999995737, 12.50000000000000000, 4.330127018922196314 ) ) ;
#91194 = CARTESIAN_POINT ( 'NONE',  ( 5.199999999999931788, 12.50000000000000000, 4.676537180435972552 ) ) ;
#91195 = LINE ( 'NONE', #50623, #17736 ) ;
#91197 = AXIS2_PLACEMENT_3D ( 'NONE', #16378, #75969, #33493 ) ;
#91196 = AXIS2_PLACEMENT_3D ( 'NONE', #114079, #13281, #72237 ) ;
#91198 = EDGE_CURVE ( 'NONE', #69482, #60983, #70733, .T. ) ;
#91199 = ORIENTED_EDGE ( 'NONE', *, *, #48114, .F. ) ;
#91200 = DIRECTION ( 'NONE',  ( 0.000000000000000000, 0.000000000000000000, 1.000000000000000000 ) ) ;
#91201 = CIRCLE ( 'NONE', #124565, 0.06509327318403745899 ) ;
#91202 = EDGE_LOOP ( 'NONE', ( #101474, #22641 ) ) ;
#91203 = DIRECTION ( 'NONE',  ( 0.000000000000000000, 0.000000000000000000, -1.000000000000000000 ) ) ;
#91204 = DIRECTION ( 'NONE',  ( -4.274815082592931898E-19, -0.9999939076577903929, -0.003490651415223739937 ) ) ;
#91205 = EDGE_LOOP ( 'NONE', ( #18213, #24901 ) ) ;
#91207 = EDGE_CURVE ( 'NONE', #122002, #90822, #72034, .T. ) ;
#91206 = CARTESIAN_POINT ( 'NONE',  ( -8.350000000000013856, 2.500000000000000000, -6.495190528383297135 ) ) ;
#91208 = CARTESIAN_POINT ( 'NONE',  ( -11.84999999999999787, 2.500000000000000000, -6.048780366869523029 ) ) ;
#91209 = ADVANCED_FACE ( 'NONE', ( #1981 ), #92297, .T. ) ;
#91210 = ORIENTED_EDGE ( 'NONE', *, *, #14322, .T. ) ;
#91211 = CARTESIAN_POINT ( 'NONE',  ( 7.899999999999924860, 2.500000000000000000, 3.537306695894645081 ) ) ;
#91212 = EDGE_CURVE ( 'NONE', #119493, #58128, #102374, .T. ) ;
#91213 = LINE ( 'NONE', #61768, #27944 ) ;
#91214 = ORIENTED_EDGE ( 'NONE', *, *, #76454, .F. ) ;
#91215 = VERTEX_POINT ( 'NONE', #89726 ) ;
#91216 = CARTESIAN_POINT ( 'NONE',  ( 1.449999999999950440, 2.500000000000000000, 6.148780366869520009 ) ) ;
#91217 = DIRECTION ( 'NONE',  ( -0.000000000000000000, -1.000000000000000000, -0.000000000000000000 ) ) ;
#91218 = EDGE_CURVE ( 'NONE', #1029, #27988, #120479, .T. ) ;
#91219 = CARTESIAN_POINT ( 'NONE',  ( 184.7552083336747444, 6.551208109652275624, -3.782341765624998686 ) ) ;
#91220 = AXIS2_PLACEMENT_3D ( 'NONE', #88217, #39181, #80379 ) ;
#91221 = DIRECTION ( 'NONE',  ( -0.000000000000000000, 1.000000000000000000, -0.000000000000000000 ) ) ;
#91222 = FACE_OUTER_BOUND ( 'NONE', #83594, .T. ) ;
#91223 = ORIENTED_EDGE ( 'NONE', *, *, #93469, .T. ) ;
#91224 = CIRCLE ( 'NONE', #80858, 0.1000000000000002554 ) ;
#91225 = DIRECTION ( 'NONE',  ( 0.000000000000000000, 0.000000000000000000, 1.000000000000000000 ) ) ;
#91226 = AXIS2_PLACEMENT_3D ( 'NONE', #5806, #33376, #85022 ) ;
#91227 = AXIS2_PLACEMENT_3D ( 'NONE', #101926, #70520, #120912 ) ;
#91228 = EDGE_LOOP ( 'NONE', ( #98461, #127806 ) ) ;
#91229 = AXIS2_PLACEMENT_3D ( 'NONE', #109482, #118647, #129150 ) ;
#91230 = DIRECTION ( 'NONE',  ( 0.000000000000000000, 0.000000000000000000, 1.000000000000000000 ) ) ;
#91231 = FACE_OUTER_BOUND ( 'NONE', #93783, .T. ) ;
#91232 = VECTOR ( 'NONE', #78036, 1000.000000000000000 ) ;
#91233 = DIRECTION ( 'NONE',  ( 0.000000000000000000, 0.000000000000000000, 1.000000000000000000 ) ) ;
#91234 = CARTESIAN_POINT ( 'NONE',  ( -1.700000000000034817, 2.500000000000000000, 0.09999999999999761857 ) ) ;
#91235 = DIRECTION ( 'NONE',  ( 0.000000000000000000, -0.000000000000000000, 1.000000000000000000 ) ) ;
#91236 = CARTESIAN_POINT ( 'NONE',  ( 8.349999999999923261, 2.500000000000000000, -6.495190528383302464 ) ) ;
#91237 = LINE ( 'NONE', #53890, #78951 ) ;
#91238 = EDGE_LOOP ( 'NONE', ( #52025, #19153, #76234, #85015 ) ) ;
#91239 = CARTESIAN_POINT ( 'NONE',  ( 11.04999999999990656, 12.50000000000000000, 2.576566944158910744 ) ) ;
#91240 = ADVANCED_FACE ( 'NONE', ( #21637 ), #11156, .T. ) ;
#91242 = CIRCLE ( 'NONE', #126839, 0.06509327318403743123 ) ;
#91241 = CIRCLE ( 'NONE', #72466, 0.09999999999999982514 ) ;
#91243 = CARTESIAN_POINT ( 'NONE',  ( -1.050000000000038236, 2.500000000000000000, -6.148780366869526226 ) ) ;
#91244 = FACE_OUTER_BOUND ( 'NONE', #72988, .T. ) ;
#91245 = ORIENTED_EDGE ( 'NONE', *, *, #21326, .T. ) ;
#91246 = EDGE_CURVE ( 'NONE', #69453, #57912, #81207, .T. ) ;
#91247 = DIRECTION ( 'NONE',  ( -4.274815082592931898E-19, -0.9999939076577903929, -0.003490651415223739937 ) ) ;
#91248 = VERTEX_POINT ( 'NONE', #50444 ) ;
#91249 = ORIENTED_EDGE ( 'NONE', *, *, #98139, .F. ) ;
#91250 = DIRECTION ( 'NONE',  ( -0.000000000000000000, -1.000000000000000000, -0.000000000000000000 ) ) ;
#91251 = ADVANCED_FACE ( 'NONE', ( #61576 ), #16659, .T. ) ;
#91252 = ORIENTED_EDGE ( 'NONE', *, *, #1380, .F. ) ;
#91253 = CARTESIAN_POINT ( 'NONE',  ( 18.09676523921901037, -2.526776815558750222, -2.684906793687110049 ) ) ;
#91254 = CARTESIAN_POINT ( 'NONE',  ( 12.09999999999990195, 12.50000000000000000, -2.276824562219559311E-15 ) ) ;
#91255 = EDGE_CURVE ( 'NONE', #8978, #3854, #73123, .T. ) ;
#91256 = EDGE_CURVE ( 'NONE', #31928, #62165, #45, .T. ) ;
#91257 = ORIENTED_EDGE ( 'NONE', *, *, #86678, .F. ) ;
#91258 = CARTESIAN_POINT ( 'NONE',  ( -11.64999999999999680, 12.50000000000000000, -2.099970236277060476 ) ) ;
#91259 = EDGE_CURVE ( 'NONE', #129286, #38823, #50238, .T. ) ;
#91260 = DIRECTION ( 'NONE',  ( 0.000000000000000000, 0.000000000000000000, 1.000000000000000000 ) ) ;
#91261 = ORIENTED_EDGE ( 'NONE', *, *, #114105, .F. ) ;
#91262 = EDGE_CURVE ( 'NONE', #1061, #93646, #83680, .T. ) ;
#91263 = EDGE_CURVE ( 'NONE', #77376, #55889, #79487, .T. ) ;
#91264 = AXIS2_PLACEMENT_3D ( 'NONE', #14980, #94217, #105332 ) ;
#91265 = EDGE_LOOP ( 'NONE', ( #45116, #128913 ) ) ;
#91266 = AXIS2_PLACEMENT_3D ( 'NONE', #76581, #98783, #77223 ) ;
#91267 = ORIENTED_EDGE ( 'NONE', *, *, #109980, .F. ) ;
#91268 = CARTESIAN_POINT ( 'NONE',  ( -7.900000000000014566, 12.50000000000000000, 0.6928203230275494784 ) ) ;
#91269 = CARTESIAN_POINT ( 'NONE',  ( -6.900000000000019007, 12.50000000000000000, 0.3464101615137735735 ) ) ;
#91270 = FACE_OUTER_BOUND ( 'NONE', #31008, .T. ) ;
#91271 = FACE_BOUND ( 'NONE', #105692, .T. ) ;
#91272 = ORIENTED_EDGE ( 'NONE', *, *, #47476, .F. ) ;
#91273 = CARTESIAN_POINT ( 'NONE',  ( 7.899999999999923084, 2.500000000000000000, -0.6928203230275542523 ) ) ;
#91274 = FACE_OUTER_BOUND ( 'NONE', #56328, .T. ) ;
#91275 = ORIENTED_EDGE ( 'NONE', *, *, #59480, .T. ) ;
#91276 = AXIS2_PLACEMENT_3D ( 'NONE', #105773, #106409, #19816 ) ;
#91277 = DIRECTION ( 'NONE',  ( 0.000000000000000000, 0.000000000000000000, 1.000000000000000000 ) ) ;
#91278 = DIRECTION ( 'NONE',  ( 0.000000000000000000, 0.000000000000000000, 1.000000000000000000 ) ) ;
#91279 = FACE_OUTER_BOUND ( 'NONE', #38606, .T. ) ;
#91280 = CARTESIAN_POINT ( 'NONE',  ( 2.499999999999947153, 12.50000000000000000, 3.637306695894644726 ) ) ;
#91281 = DIRECTION ( 'NONE',  ( 0.000000000000000000, 0.000000000000000000, -1.000000000000000000 ) ) ;
#91282 = DIRECTION ( 'NONE',  ( 0.000000000000000000, 1.000000000000000000, 0.000000000000000000 ) ) ;
#91283 = FACE_OUTER_BOUND ( 'NONE', #106309, .T. ) ;
#91285 = AXIS2_PLACEMENT_3D ( 'NONE', #46502, #9170, #98828 ) ;
#91284 = AXIS2_PLACEMENT_3D ( 'NONE', #98947, #60333, #110061 ) ;
#91286 = VECTOR ( 'NONE', #54315, 1000.000000000000000 ) ;
#91287 = VERTEX_POINT ( 'NONE', #42583 ) ;
#91288 = ORIENTED_EDGE ( 'NONE', *, *, #10270, .T. ) ;
#91289 = EDGE_LOOP ( 'NONE', ( #75540, #88641 ) ) ;
#91290 = ORIENTED_EDGE ( 'NONE', *, *, #112579, .F. ) ;
#91291 = DIRECTION ( 'NONE',  ( 0.000000000000000000, 0.000000000000000000, 1.000000000000000000 ) ) ;
#91292 = DIRECTION ( 'NONE',  ( -0.000000000000000000, 1.000000000000000000, -0.000000000000000000 ) ) ;
#91293 = VERTEX_POINT ( 'NONE', #104060 ) ;
#91294 = FACE_BOUND ( 'NONE', #106430, .T. ) ;
#91295 = CARTESIAN_POINT ( 'NONE',  ( -9.150000000000011013, 2.500000000000000000, -5.902370205355745192 ) ) ;
#91296 = DIRECTION ( 'NONE',  ( 0.000000000000000000, 0.000000000000000000, 1.000000000000000000 ) ) ;
#91297 = DIRECTION ( 'NONE',  ( 0.000000000000000000, -0.9999939076577903929, 0.003490651415223739937 ) ) ;
#91298 = DIRECTION ( 'NONE',  ( 0.000000000000000000, 0.000000000000000000, -1.000000000000000000 ) ) ;
#91299 = CARTESIAN_POINT ( 'NONE',  ( -6.250000000000015987, 12.50000000000000000, 5.802370205355744659 ) ) ;
#91300 = CARTESIAN_POINT ( 'NONE',  ( 184.4999999999999716, -1.540470907863150662, 7.523675357873957914 ) ) ;
#91301 = CARTESIAN_POINT ( 'NONE',  ( 9.149999999999920419, 2.500000000000000000, 2.757883832488649656 ) ) ;
#91302 = FACE_OUTER_BOUND ( 'NONE', #72022, .T. ) ;
#91303 = CARTESIAN_POINT ( 'NONE',  ( -9.550000000000006040, 2.500000000000000000, -2.265063509461101798 ) ) ;
#91305 = EDGE_LOOP ( 'NONE', ( #16469, #127192, #55759, #10879 ) ) ;
#91304 = AXIS2_PLACEMENT_3D ( 'NONE', #55421, #36445, #65875 ) ;
#91306 = CIRCLE ( 'NONE', #47686, 0.06509327318403745899 ) ;
#91307 = CIRCLE ( 'NONE', #83197, 0.06509327318403743123 ) ;
#91308 = ORIENTED_EDGE ( 'NONE', *, *, #20357, .T. ) ;
#91309 = EDGE_CURVE ( 'NONE', #21008, #35122, #127595, .T. ) ;
#91310 = ORIENTED_EDGE ( 'NONE', *, *, #62293, .F. ) ;
#91312 = ORIENTED_EDGE ( 'NONE', *, *, #11322, .T. ) ;
#91311 = VECTOR ( 'NONE', #82749, 1000.000000000000000 ) ;
#91313 = VERTEX_POINT ( 'NONE', #75238 ) ;
#91314 = EDGE_LOOP ( 'NONE', ( #1816, #71935 ) ) ;
#91315 = CARTESIAN_POINT ( 'NONE',  ( 5.849999999999935696, 2.500000000000000000, -7.088010851410853519 ) ) ;
#91316 = VERTEX_POINT ( 'NONE', #53032 ) ;
#91317 = CIRCLE ( 'NONE', #34904, 0.1000000000000002554 ) ;
#91318 = CIRCLE ( 'NONE', #55812, 0.1000000000000002554 ) ;
#91319 = CONICAL_SURFACE ( 'NONE', #20309, 0.1000000000000002554, 0.003490658503988666988 ) ;
#91320 = CARTESIAN_POINT ( 'NONE',  ( 185.7500000000000000, 9.429780353434619030E-16, -7.700000000000000178 ) ) ;
#91321 = DIRECTION ( 'NONE',  ( 0.000000000000000000, -0.000000000000000000, 1.000000000000000000 ) ) ;
#91322 = DIRECTION ( 'NONE',  ( 0.000000000000000000, 1.000000000000000000, 0.000000000000000000 ) ) ;
#91323 = CARTESIAN_POINT ( 'NONE',  ( 5.649999999999936406, 2.500000000000000000, -6.941600689897077459 ) ) ;
#91324 = CIRCLE ( 'NONE', #34912, 0.06509327318403745899 ) ;
#91325 = ORIENTED_EDGE ( 'NONE', *, *, #93887, .T. ) ;
#91326 = LINE ( 'NONE', #10799, #75590 ) ;
#91327 = AXIS2_PLACEMENT_3D ( 'NONE', #9324, #21732, #19122 ) ;
#91328 = VERTEX_POINT ( 'NONE', #94233 ) ;
#91330 = CONICAL_SURFACE ( 'NONE', #89278, 0.1000000000000002554, 0.003490658503988666988 ) ;
#91329 = AXIS2_PLACEMENT_3D ( 'NONE', #37737, #77637, #38396 ) ;
#91331 = ORIENTED_EDGE ( 'NONE', *, *, #39020, .F. ) ;
#91332 = LINE ( 'NONE', #122093, #17552 ) ;
#91333 = CARTESIAN_POINT ( 'NONE',  ( -1.650000000000034328, 12.50000000000000000, -6.495190528383302464 ) ) ;
#91334 = DIRECTION ( 'NONE',  ( -0.000000000000000000, -1.000000000000000000, -0.000000000000000000 ) ) ;
#91335 = VERTEX_POINT ( 'NONE', #4534 ) ;
#91336 = ORIENTED_EDGE ( 'NONE', *, *, #100683, .F. ) ;
#91337 = CARTESIAN_POINT ( 'NONE',  ( 1.699999999999951994, 12.50000000000000000, -4.330127018922201643 ) ) ;
#91338 = DIRECTION ( 'NONE',  ( -4.274815082592931898E-19, -0.9999939076577903929, -0.003490651415223739937 ) ) ;
#91339 = CARTESIAN_POINT ( 'NONE',  ( 12.89999999999990266, 2.500000000000000000, 5.022947341949748790 ) ) ;
#91340 = CARTESIAN_POINT ( 'NONE',  ( 2.299999999999949640, 2.500000000000000000, -4.576537180435977348 ) ) ;
#91341 = VERTEX_POINT ( 'NONE', #85056 ) ;
#91342 = FACE_OUTER_BOUND ( 'NONE', #11144, .T. ) ;
#91343 = AXIS2_PLACEMENT_3D ( 'NONE', #63302, #114334, #3735 ) ;
#91344 = EDGE_LOOP ( 'NONE', ( #36253, #19326, #31683, #125416 ) ) ;
#91345 = DIRECTION ( 'NONE',  ( 0.000000000000000000, 0.000000000000000000, -1.000000000000000000 ) ) ;
#91346 = EDGE_CURVE ( 'NONE', #49349, #114386, #100407, .T. ) ;
#91347 = EDGE_LOOP ( 'NONE', ( #31007, #37259, #2029, #122800 ) ) ;
#91348 = DIRECTION ( 'NONE',  ( 0.000000000000000000, 0.000000000000000000, 1.000000000000000000 ) ) ;
#91349 = CARTESIAN_POINT ( 'NONE',  ( 32.25969734032662473, -3.190781473932518875, 3.146220229225281440 ) ) ;
#91350 = DIRECTION ( 'NONE',  ( 0.000000000000000000, -0.000000000000000000, 1.000000000000000000 ) ) ;
#91351 = EDGE_CURVE ( 'NONE', #35123, #122362, #106657, .T. ) ;
#91352 = DIRECTION ( 'NONE',  ( 0.000000000000000000, 1.000000000000000000, 0.000000000000000000 ) ) ;
#91353 = ADVANCED_FACE ( 'NONE', ( #94882 ), #29306, .T. ) ;
#91354 = ORIENTED_EDGE ( 'NONE', *, *, #112640, .F. ) ;
#91355 = DIRECTION ( 'NONE',  ( 0.000000000000000000, 0.000000000000000000, 1.000000000000000000 ) ) ;
#91356 = AXIS2_PLACEMENT_3D ( 'NONE', #37638, #24102, #77537 ) ;
#91357 = EDGE_CURVE ( 'NONE', #81317, #29090, #123380, .T. ) ;
#91358 = DIRECTION ( 'NONE',  ( 0.000000000000000000, 1.000000000000000000, 0.000000000000000000 ) ) ;
#91359 = ORIENTED_EDGE ( 'NONE', *, *, #121628, .T. ) ;
#91360 = EDGE_CURVE ( 'NONE', #39986, #54702, #43870, .T. ) ;
#91361 = ORIENTED_EDGE ( 'NONE', *, *, #122252, .F. ) ;
#91362 = EDGE_CURVE ( 'NONE', #96053, #84082, #35329, .T. ) ;
#91363 = EDGE_LOOP ( 'NONE', ( #8573, #111380, #27365, #94476 ) ) ;
#91364 = DIRECTION ( 'NONE',  ( 0.000000000000000000, 1.000000000000000000, 0.000000000000000000 ) ) ;
#91365 = DIRECTION ( 'NONE',  ( 0.000000000000000000, 1.000000000000000000, 0.000000000000000000 ) ) ;
#91366 = EDGE_CURVE ( 'NONE', #97899, #28983, #27232, .T. ) ;
#91367 = CARTESIAN_POINT ( 'NONE',  ( -0.4500000000000397571, 12.50000000000000000, -2.099970236277064473 ) ) ;
#91368 = FACE_OUTER_BOUND ( 'NONE', #65294, .T. ) ;
#91371 = CIRCLE ( 'NONE', #60087, 0.06509327318403745899 ) ;
#91370 = DIRECTION ( 'NONE',  ( 0.000000000000000000, 0.000000000000000000, 1.000000000000000000 ) ) ;
#91369 = CONICAL_SURFACE ( 'NONE', #5666, 0.1000000000000002554, 0.003490658503988666988 ) ;
#91372 = DIRECTION ( 'NONE',  ( 0.000000000000000000, 1.000000000000000000, 0.000000000000000000 ) ) ;
#91373 = DIRECTION ( 'NONE',  ( 0.000000000000000000, 1.000000000000000000, 0.000000000000000000 ) ) ;
#91374 = CARTESIAN_POINT ( 'NONE',  ( -1.850000000000033840, 2.500000000000000000, 2.411473670974873862 ) ) ;
#91376 = CIRCLE ( 'NONE', #34965, 0.06509327318403745899 ) ;
#91375 = AXIS2_PLACEMENT_3D ( 'NONE', #2335, #11530, #20075 ) ;
#91377 = VECTOR ( 'NONE', #308, 1000.000000000000000 ) ;
#91378 = ORIENTED_EDGE ( 'NONE', *, *, #98476, .F. ) ;
#91379 = CARTESIAN_POINT ( 'NONE',  ( 8.949999999999921130, 2.500000000000000000, -6.841600689897078702 ) ) ;
#91380 = CARTESIAN_POINT ( 'NONE',  ( -9.800000000000004263, 2.500000000000000000, -0.2464101615137783419 ) ) ;
#91381 = DIRECTION ( 'NONE',  ( -0.000000000000000000, -1.000000000000000000, -0.000000000000000000 ) ) ;
#91382 = DIRECTION ( 'NONE',  ( 0.000000000000000000, -0.000000000000000000, 1.000000000000000000 ) ) ;
#91383 = ORIENTED_EDGE ( 'NONE', *, *, #99495, .F. ) ;
#91384 = LINE ( 'NONE', #71757, #92701 ) ;
#91385 = CARTESIAN_POINT ( 'NONE',  ( 1.449999999999951772, 2.500000000000000000, -6.248780366869526759 ) ) ;
#91387 = EDGE_LOOP ( 'NONE', ( #17570, #65540, #44940, #61106 ) ) ;
#91386 = LINE ( 'NONE', #1713, #2381 ) ;
#91388 = EDGE_CURVE ( 'NONE', #25038, #9068, #123059, .T. ) ;
#91389 = AXIS2_PLACEMENT_3D ( 'NONE', #102727, #72654, #3262 ) ;
#91390 = ORIENTED_EDGE ( 'NONE', *, *, #8523, .T. ) ;
#91391 = AXIS2_PLACEMENT_3D ( 'NONE', #92436, #2766, #10628 ) ;
#91392 = DIRECTION ( 'NONE',  ( 0.000000000000000000, 0.000000000000000000, -1.000000000000000000 ) ) ;
#91393 = AXIS2_PLACEMENT_3D ( 'NONE', #116688, #69520, #109455 ) ;
#91394 = ORIENTED_EDGE ( 'NONE', *, *, #38682, .F. ) ;
#91395 = ORIENTED_EDGE ( 'NONE', *, *, #9212, .F. ) ;
#91396 = DIRECTION ( 'NONE',  ( 0.000000000000000000, 0.000000000000000000, 1.000000000000000000 ) ) ;
#91397 = EDGE_CURVE ( 'NONE', #54474, #32010, #77415, .T. ) ;
#91398 = ADVANCED_FACE ( 'NONE', ( #95536 ), #43974, .T. ) ;
#91399 = CONICAL_SURFACE ( 'NONE', #116528, 0.09999999999999999167, 0.003490658503988666988 ) ;
#91400 = DIRECTION ( 'NONE',  ( 0.000000000000000000, -0.9999939076577903929, 0.003490651415223739937 ) ) ;
#91402 = EDGE_CURVE ( 'NONE', #57508, #85963, #63567, .T. ) ;
#91401 = DIRECTION ( 'NONE',  ( -4.274815082592931898E-19, -0.9999939076577903929, -0.003490651415223739937 ) ) ;
#91403 = VECTOR ( 'NONE', #123483, 1000.000000000000000 ) ;
#91404 = LINE ( 'NONE', #70476, #106455 ) ;
#91405 = ORIENTED_EDGE ( 'NONE', *, *, #42678, .T. ) ;
#91406 = CIRCLE ( 'NONE', #85141, 7.700000000000000178 ) ;
#91407 = DIRECTION ( 'NONE',  ( 0.000000000000000000, 0.000000000000000000, 1.000000000000000000 ) ) ;
#91408 = ORIENTED_EDGE ( 'NONE', *, *, #3450, .T. ) ;
#91409 = EDGE_CURVE ( 'NONE', #71314, #89603, #71148, .T. ) ;
#91410 = DIRECTION ( 'NONE',  ( 0.000000000000000000, 1.000000000000000000, 0.000000000000000000 ) ) ;
#91411 = CONICAL_SURFACE ( 'NONE', #7785, 0.09999999999999982514, 0.003490658503988666988 ) ;
#91412 = EDGE_CURVE ( 'NONE', #113972, #19198, #114959, .T. ) ;
#91413 = DIRECTION ( 'NONE',  ( -0.000000000000000000, 1.000000000000000000, -0.000000000000000000 ) ) ;
#91414 = ADVANCED_FACE ( 'NONE', ( #93594 ), #62760, .T. ) ;
#91415 = ORIENTED_EDGE ( 'NONE', *, *, #93046, .T. ) ;
#91416 = EDGE_CURVE ( 'NONE', #20895, #123590, #2087, .T. ) ;
#91419 = ADVANCED_FACE ( 'NONE', ( #117081 ), #7781, .T. ) ;
#91418 = AXIS2_PLACEMENT_3D ( 'NONE', #48482, #30633, #81007 ) ;
#91417 = AXIS2_PLACEMENT_3D ( 'NONE', #93922, #74928, #86006 ) ;
#91420 = ORIENTED_EDGE ( 'NONE', *, *, #94787, .F. ) ;
#91421 = ORIENTED_EDGE ( 'NONE', *, *, #106189, .F. ) ;
#91422 = ORIENTED_EDGE ( 'NONE', *, *, #72772, .F. ) ;
#91423 = DIRECTION ( 'NONE',  ( 0.000000000000000000, 1.000000000000000000, 0.000000000000000000 ) ) ;
#91424 = CARTESIAN_POINT ( 'NONE',  ( 6.598553918452118694, 2.499999999999999112, 8.770211965177473701 ) ) ;
#91425 = LINE ( 'NONE', #121507, #111050 ) ;
#91426 = FACE_BOUND ( 'NONE', #83821, .T. ) ;
#91427 = CARTESIAN_POINT ( 'NONE',  ( 4.149999999999939959, 2.500000000000000000, 2.857883832488649301 ) ) ;
#91428 = CARTESIAN_POINT ( 'NONE',  ( 184.9895833340161175, -4.445597072760115509, -7.700000000000001954 ) ) ;
#91429 = ADVANCED_FACE ( 'NONE', ( #107277 ), #20979, .T. ) ;
#91430 = DIRECTION ( 'NONE',  ( 0.000000000000000000, 0.000000000000000000, 1.000000000000000000 ) ) ;
#91431 = LINE ( 'NONE', #71799, #8238 ) ;
#91432 = DIRECTION ( 'NONE',  ( -0.000000000000000000, 1.000000000000000000, -0.000000000000000000 ) ) ;
#91433 = CARTESIAN_POINT ( 'NONE',  ( -11.84999999999999787, 12.50000000000000000, -6.906693963081111498 ) ) ;
#91434 = CONICAL_SURFACE ( 'NONE', #45487, 0.09999999999999982514, 0.003490658503988666988 ) ;
#91435 = CARTESIAN_POINT ( 'NONE',  ( -10.45000000000000462, 2.500000000000000000, -2.165063509461097713 ) ) ;
#91436 = DIRECTION ( 'NONE',  ( 0.000000000000000000, -0.000000000000000000, 1.000000000000000000 ) ) ;
#91437 = VERTEX_POINT ( 'NONE', #68639 ) ;
#91438 = VERTEX_POINT ( 'NONE', #77177 ) ;
#91439 = ORIENTED_EDGE ( 'NONE', *, *, #34039, .F. ) ;
#91440 = ORIENTED_EDGE ( 'NONE', *, *, #74412, .T. ) ;
#91441 = EDGE_LOOP ( 'NONE', ( #57, #77765, #31059, #123803 ) ) ;
#91442 = DIRECTION ( 'NONE',  ( 0.000000000000000000, 0.000000000000000000, 1.000000000000000000 ) ) ;
#91443 = CARTESIAN_POINT ( 'NONE',  ( 129.5000000000000000, 0.6250000000000000000, 7.634788798650556707 ) ) ;
#91444 = VERTEX_POINT ( 'NONE', #125614 ) ;
#91445 = FACE_BOUND ( 'NONE', #44970, .T. ) ;
#91446 = DIRECTION ( 'NONE',  ( -0.000000000000000000, -1.000000000000000000, -0.000000000000000000 ) ) ;
#91447 = VECTOR ( 'NONE', #71529, 1000.000000000000000 ) ;
#91448 = CONICAL_SURFACE ( 'NONE', #39255, 0.1000000000000002554, 0.003490658503988666988 ) ;
#91449 = EDGE_LOOP ( 'NONE', ( #58554, #72612 ) ) ;
#91450 = FACE_OUTER_BOUND ( 'NONE', #91238, .T. ) ;
#91451 = PLANE ( 'NONE',  #91227 ) ;
#91452 = FACE_OUTER_BOUND ( 'NONE', #187, .T. ) ;
#91453 = DIRECTION ( 'NONE',  ( 0.000000000000000000, 0.000000000000000000, 1.000000000000000000 ) ) ;
#91454 = EDGE_LOOP ( 'NONE', ( #27096, #81576 ) ) ;
#91455 = CARTESIAN_POINT ( 'NONE',  ( -4.600000000000025402, 12.50000000000000000, 4.265033745738159077 ) ) ;
#91456 = VECTOR ( 'NONE', #93505, 1000.000000000000000 ) ;
#91457 = AXIS2_PLACEMENT_3D ( 'NONE', #123220, #31618, #83302 ) ;
#91458 = EDGE_CURVE ( 'NONE', #53767, #65379, #27411, .T. ) ;
#91459 = ORIENTED_EDGE ( 'NONE', *, *, #80122, .T. ) ;
#91460 = ORIENTED_EDGE ( 'NONE', *, *, #59462, .F. ) ;
#91461 = DIRECTION ( 'NONE',  ( 0.000000000000000000, 0.000000000000000000, -1.000000000000000000 ) ) ;
#91462 = DIRECTION ( 'NONE',  ( 0.000000000000000000, 0.000000000000000000, 1.000000000000000000 ) ) ;
#91463 = ORIENTED_EDGE ( 'NONE', *, *, #46156, .F. ) ;
#91464 = LINE ( 'NONE', #34506, #83118 ) ;
#91465 = CIRCLE ( 'NONE', #76805, 0.06509327318403745899 ) ;
#91466 = AXIS2_PLACEMENT_3D ( 'NONE', #13851, #53782, #95009 ) ;
#91467 = CARTESIAN_POINT ( 'NONE',  ( 12.29999999999990301, 12.50000000000000000, -0.2813168883297408329 ) ) ;
#91468 = CARTESIAN_POINT ( 'NONE',  ( -7.900000000000011013, 12.50000000000000000, 5.088040615133786027 ) ) ;
#91469 = DIRECTION ( 'NONE',  ( -0.000000000000000000, 1.000000000000000000, -0.000000000000000000 ) ) ;
#91470 = CARTESIAN_POINT ( 'NONE',  ( 187.1145833340161175, 6.668395609140177704, -3.849999999999998312 ) ) ;
#91471 = VERTEX_POINT ( 'NONE', #98098 ) ;
#91472 = EDGE_CURVE ( 'NONE', #63798, #59733, #7128, .T. ) ;
#91473 = CARTESIAN_POINT ( 'NONE',  ( 5.799999999999934985, 2.500000000000000000, -4.330127018922201643 ) ) ;
#91474 = ORIENTED_EDGE ( 'NONE', *, *, #127470, .T. ) ;
#91475 = CARTESIAN_POINT ( 'NONE',  ( 3.349999999999943689, 2.500000000000000000, 1.572243186433545548 ) ) ;
#91476 = AXIS2_PLACEMENT_3D ( 'NONE', #14654, #25133, #55254 ) ;
#91477 = ORIENTED_EDGE ( 'NONE', *, *, #14336, .T. ) ;
#91478 = DIRECTION ( 'NONE',  ( 0.000000000000000000, 0.000000000000000000, -1.000000000000000000 ) ) ;
#91479 = EDGE_LOOP ( 'NONE', ( #121765, #5185, #19365, #26313 ) ) ;
#91480 = CARTESIAN_POINT ( 'NONE',  ( -3.350000000000032507, 2.500000000000000000, -6.495190528383302464 ) ) ;
#91481 = AXIS2_PLACEMENT_3D ( 'NONE', #98870, #117194, #7908 ) ;
#91482 = CARTESIAN_POINT ( 'NONE',  ( 108.0000000000000142, 8.500000000000000000, 2.749999999999997335 ) ) ;
#91483 = LINE ( 'NONE', #41765, #88538 ) ;
#91484 = DIRECTION ( 'NONE',  ( 0.000000000000000000, 0.000000000000000000, -1.000000000000000000 ) ) ;
#91486 = CIRCLE ( 'NONE', #66348, 0.09999999999999982514 ) ;
#91485 = DIRECTION ( 'NONE',  ( 0.000000000000000000, 1.000000000000000000, 0.000000000000000000 ) ) ;
#91487 = ORIENTED_EDGE ( 'NONE', *, *, #39578, .F. ) ;
#91488 = VECTOR ( 'NONE', #127710, 1000.000000000000000 ) ;
#91489 = EDGE_LOOP ( 'NONE', ( #56549, #95481 ) ) ;
#91490 = VERTEX_POINT ( 'NONE', #85699 ) ;
#91491 = CARTESIAN_POINT ( 'NONE',  ( -0.6000000000000323963, 12.50000000000000000, 0.4115034346978133639 ) ) ;
#91492 = AXIS2_PLACEMENT_3D ( 'NONE', #118113, #28467, #89944 ) ;
#91493 = DIRECTION ( 'NONE',  ( -0.000000000000000000, 1.000000000000000000, -0.000000000000000000 ) ) ;
#91494 = DIRECTION ( 'NONE',  ( 0.000000000000000000, 0.000000000000000000, 1.000000000000000000 ) ) ;
#91496 = ORIENTED_EDGE ( 'NONE', *, *, #44871, .T. ) ;
#91495 = ORIENTED_EDGE ( 'NONE', *, *, #86045, .T. ) ;
#91497 = VERTEX_POINT ( 'NONE', #67320 ) ;
#91498 = DIRECTION ( 'NONE',  ( 0.000000000000000000, 1.000000000000000000, 0.000000000000000000 ) ) ;
#91499 = CONICAL_SURFACE ( 'NONE', #3764, 0.1000000000000002554, 0.003490658503988666988 ) ;
#91500 = CIRCLE ( 'NONE', #85242, 0.06509327318403745899 ) ;
#91501 = EDGE_LOOP ( 'NONE', ( #45890, #71245 ) ) ;
#91502 = CARTESIAN_POINT ( 'NONE',  ( 7.099999999999926814, 2.500000000000000000, 0.09999999999999772959 ) ) ;
#91503 = CARTESIAN_POINT ( 'NONE',  ( 10.84999999999990905, 2.500000000000000000, 2.757883832488649656 ) ) ;
#91504 = CIRCLE ( 'NONE', #64310, 0.06509327318403745899 ) ;
#91505 = EDGE_CURVE ( 'NONE', #22140, #7809, #47087, .T. ) ;
#91506 = CARTESIAN_POINT ( 'NONE',  ( -11.44999999999999751, 2.500000000000000000, -6.841600689897074261 ) ) ;
#91507 = DIRECTION ( 'NONE',  ( 0.000000000000000000, 0.000000000000000000, 1.000000000000000000 ) ) ;
#91508 = CARTESIAN_POINT ( 'NONE',  ( 12.29999999999990479, 2.500000000000000000, -3.983716857408426293 ) ) ;
#91509 = LINE ( 'NONE', #52238, #3255 ) ;
#91510 = DIRECTION ( 'NONE',  ( 0.000000000000000000, -0.9999939076577903929, 0.003490651415223739937 ) ) ;
#91511 = CIRCLE ( 'NONE', #122914, 0.06509327318403745899 ) ;
#91512 = CARTESIAN_POINT ( 'NONE',  ( 0.4499999999999552136, 12.50000000000000000, 6.495190528383297135 ) ) ;
#91513 = ADVANCED_FACE ( 'NONE', ( #57542 ), #41838, .T. ) ;
#91514 = ORIENTED_EDGE ( 'NONE', *, *, #57832, .F. ) ;
#91515 = DIRECTION ( 'NONE',  ( 0.000000000000000000, 1.000000000000000000, 0.000000000000000000 ) ) ;
#91516 = CIRCLE ( 'NONE', #47611, 0.06509327318403745899 ) ;
#91517 = CARTESIAN_POINT ( 'NONE',  ( 43.31961220463779938, -2.029667686306299235, 5.113275312221519542 ) ) ;
#91518 = ADVANCED_FACE ( 'NONE', ( #38568 ), #85721, .T. ) ;
#91519 = ORIENTED_EDGE ( 'NONE', *, *, #646, .F. ) ;
#91520 = ADVANCED_FACE ( 'NONE', ( #58199 ), #110850, .T. ) ;
#91521 = EDGE_LOOP ( 'NONE', ( #85689, #100727, #106138, #122157 ) ) ;
#91523 = EDGE_CURVE ( 'NONE', #100782, #96782, #119184, .T. ) ;
#91522 =( REPRESENTATION_RELATIONSHIP ('NONE','NONE', #102928, #107120 ) REPRESENTATION_RELATIONSHIP_WITH_TRANSFORMATION ( #38566 )SHAPE_REPRESENTATION_RELATIONSHIP( ) );
#91524 = CARTESIAN_POINT ( 'NONE',  ( 186.4218750003414016, 0.000000000000000000, 7.564683531250000925 ) ) ;
#91526 = EDGE_CURVE ( 'NONE', #113663, #123590, #75881, .T. ) ;
#91525 = DIRECTION ( 'NONE',  ( 0.000000000000000000, 0.000000000000000000, 1.000000000000000000 ) ) ;
#91527 = EDGE_CURVE ( 'NONE', #45295, #60915, #36628, .T. ) ;
#91528 = CARTESIAN_POINT ( 'NONE',  ( -3.550000000000028244, 2.500000000000000000, 2.511473670974873507 ) ) ;
#91529 = DIRECTION ( 'NONE',  ( 0.000000000000000000, 1.000000000000000000, 0.000000000000000000 ) ) ;
#91530 = CARTESIAN_POINT ( 'NONE',  ( 12.04999999999990479, 12.50000000000000000, -6.495190528383302464 ) ) ;
#91531 = DIRECTION ( 'NONE',  ( 0.000000000000000000, 0.000000000000000000, -1.000000000000000000 ) ) ;
#91532 = FACE_OUTER_BOUND ( 'NONE', #31557, .T. ) ;
#91533 = FACE_OUTER_BOUND ( 'NONE', #39429, .T. ) ;
#91534 = EDGE_CURVE ( 'NONE', #61946, #18239, #73217, .T. ) ;
#91536 = ADVANCED_FACE ( 'NONE', ( #18249 ), #118382, .T. ) ;
#91535 = DIRECTION ( 'NONE',  ( 0.000000000000000000, 0.000000000000000000, 1.000000000000000000 ) ) ;
#91537 = ORIENTED_EDGE ( 'NONE', *, *, #123318, .T. ) ;
#91538 = EDGE_CURVE ( 'NONE', #75118, #109041, #38350, .T. ) ;
#91539 = ORIENTED_EDGE ( 'NONE', *, *, #11037, .T. ) ;
#91540 = VERTEX_POINT ( 'NONE', #108746 ) ;
#91541 = AXIS2_PLACEMENT_3D ( 'NONE', #80075, #70905, #120004 ) ;
#91542 = ORIENTED_EDGE ( 'NONE', *, *, #39379, .T. ) ;
#91543 = CARTESIAN_POINT ( 'NONE',  ( -8.550000000000009592, 12.50000000000000000, 6.776507416713035248 ) ) ;
#91544 = DIRECTION ( 'NONE',  ( 0.000000000000000000, 0.000000000000000000, 1.000000000000000000 ) ) ;
#91545 = ORIENTED_EDGE ( 'NONE', *, *, #44067, .F. ) ;
#91546 = CIRCLE ( 'NONE', #39341, 0.06509327318403745899 ) ;
#91547 = DIRECTION ( 'NONE',  ( 0.000000000000000000, 0.000000000000000000, -1.000000000000000000 ) ) ;
#91549 = LINE ( 'NONE', #19587, #113518 ) ;
#91548 = AXIS2_PLACEMENT_3D ( 'NONE', #127778, #118601, #49245 ) ;
#91550 = DIRECTION ( 'NONE',  ( 0.000000000000000000, 1.000000000000000000, 0.000000000000000000 ) ) ;
#91552 = ORIENTED_EDGE ( 'NONE', *, *, #38009, .T. ) ;
#91551 = CARTESIAN_POINT ( 'NONE',  ( 5.399999999999933742, 12.50000000000000000, -2.385244779468109755E-15 ) ) ;
#91553 = CARTESIAN_POINT ( 'NONE',  ( -7.900000000000011013, 2.500000000000000000, 4.922947341949748257 ) ) ;
#91554 = CIRCLE ( 'NONE', #24658, 0.09999999999999999167 ) ;
#91555 = FACE_OUTER_BOUND ( 'NONE', #110590, .T. ) ;
#91556 = ORIENTED_EDGE ( 'NONE', *, *, #48222, .F. ) ;
#91557 = AXIS2_PLACEMENT_3D ( 'NONE', #117887, #128391, #38731 ) ;
#91558 = ORIENTED_EDGE ( 'NONE', *, *, #83308, .T. ) ;
#91559 = ORIENTED_EDGE ( 'NONE', *, *, #37928, .T. ) ;
#91560 = ORIENTED_EDGE ( 'NONE', *, *, #19227, .T. ) ;
#91561 = DIRECTION ( 'NONE',  ( -0.000000000000000000, 1.000000000000000000, -0.000000000000000000 ) ) ;
#91562 = DIRECTION ( 'NONE',  ( 0.000000000000000000, 0.000000000000000000, 1.000000000000000000 ) ) ;
#91563 = LINE ( 'NONE', #23461, #60808 ) ;
#91564 = ORIENTED_EDGE ( 'NONE', *, *, #40064, .T. ) ;
#91565 = DIRECTION ( 'NONE',  ( -0.000000000000000000, -1.000000000000000000, -0.000000000000000000 ) ) ;
#91566 = EDGE_LOOP ( 'NONE', ( #81567, #78397 ) ) ;
#91567 = CONICAL_SURFACE ( 'NONE', #49729, 0.09999999999999982514, 0.003490658503988666988 ) ;
#91568 = CARTESIAN_POINT ( 'NONE',  ( -7.300000000000016698, 2.500000000000000000, -4.576537180435978236 ) ) ;
#91569 = FACE_OUTER_BOUND ( 'NONE', #70883, .T. ) ;
#91570 = DIRECTION ( 'NONE',  ( -0.000000000000000000, -1.000000000000000000, -0.000000000000000000 ) ) ;
#91571 = CARTESIAN_POINT ( 'NONE',  ( -2.499999999999996003, 2.500000000000000000, -4.430127018922202176 ) ) ;
#91572 = EDGE_CURVE ( 'NONE', #25412, #53467, #33513, .T. ) ;
#91573 = EDGE_CURVE ( 'NONE', #70439, #6072, #108106, .T. ) ;
#91574 = EDGE_LOOP ( 'NONE', ( #57263, #36037, #75265, #50339 ) ) ;
#91575 = CONICAL_SURFACE ( 'NONE', #16239, 0.1000000000000000472, 0.003490658503988666988 ) ;
#91576 = ADVANCED_FACE ( 'NONE', ( #76722 ), #25252, .T. ) ;
#91577 = MECHANICAL_DESIGN_GEOMETRIC_PRESENTATION_REPRESENTATION (  '', ( #33110 ), #129263 ) ;
#91578 = EDGE_LOOP ( 'NONE', ( #42475, #3273 ) ) ;
#91579 = ORIENTED_EDGE ( 'NONE', *, *, #48422, .T. ) ;
#91580 = CARTESIAN_POINT ( 'NONE',  ( -8.150000000000012790, 12.50000000000000000, 2.511473670974873507 ) ) ;
#91581 = CARTESIAN_POINT ( 'NONE',  ( -6.050000000000017586, 2.500000000000000000, 1.818653347947321475 ) ) ;
#91582 = FACE_BOUND ( 'NONE', #101585, .T. ) ;
#91583 = AXIS2_PLACEMENT_3D ( 'NONE', #118693, #110804, #61062 ) ;
#91584 = CARTESIAN_POINT ( 'NONE',  ( 0.3999999999999555023, 2.500000000000000000, 4.230127018922196669 ) ) ;
#91585 = LINE ( 'NONE', #61497, #63315 ) ;
#91586 = AXIS2_PLACEMENT_3D ( 'NONE', #39995, #692, #79904 ) ;
#91587 = ADVANCED_FACE ( 'NONE', ( #27597 ), #58387, .T. ) ;
#91588 = DIRECTION ( 'NONE',  ( -0.000000000000000000, 1.000000000000000000, -0.000000000000000000 ) ) ;
#91589 = AXIS2_PLACEMENT_3D ( 'NONE', #84643, #67557, #118608 ) ;
#91590 = CARTESIAN_POINT ( 'NONE',  ( -4.076600168545496672E-14, 12.50000000000000000, -5.022947341949754119 ) ) ;
#91592 = LINE ( 'NONE', #64063, #86373 ) ;
#91591 = CONICAL_SURFACE ( 'NONE', #28912, 0.1000000000000002554, 0.003490658503988666988 ) ;
#91593 = LINE ( 'NONE', #61506, #65721 ) ;
#91594 = VERTEX_POINT ( 'NONE', #17113 ) ;
#91595 = FACE_OUTER_BOUND ( 'NONE', #52608, .T. ) ;
#91596 = CARTESIAN_POINT ( 'NONE',  ( 4.999999999999938716, 2.500000000000000000, -4.922947341949753586 ) ) ;
#91597 = EDGE_LOOP ( 'NONE', ( #81169, #43660 ) ) ;
#91598 = VERTEX_POINT ( 'NONE', #47271 ) ;
#91599 = DIRECTION ( 'NONE',  ( 0.000000000000000000, 1.000000000000000000, 0.000000000000000000 ) ) ;
#91600 = AXIS2_PLACEMENT_3D ( 'NONE', #7067, #126873, #37208 ) ;
#91601 = DIRECTION ( 'NONE',  ( 0.000000000000000000, 0.000000000000000000, 1.000000000000000000 ) ) ;
#91602 = ADVANCED_FACE ( 'NONE', ( #26985 ), #121414, .T. ) ;
#91603 = FACE_BOUND ( 'NONE', #88243, .T. ) ;
#91604 = DIRECTION ( 'NONE',  ( 0.000000000000000000, 1.000000000000000000, 0.000000000000000000 ) ) ;
#91606 = AXIS2_PLACEMENT_3D ( 'NONE', #69499, #19778, #90420 ) ;
#91605 = AXIS2_PLACEMENT_3D ( 'NONE', #90870, #90208, #48536 ) ;
#91607 = VERTEX_POINT ( 'NONE', #66887 ) ;
#91608 = CARTESIAN_POINT ( 'NONE',  ( 8.949999999999919353, 2.500000000000000000, -6.148780366869526226 ) ) ;
#91609 = CARTESIAN_POINT ( 'NONE',  ( 185.1250000000000284, -8.891194145520236347, -1.633285867636356693E-15 ) ) ;
#91610 = EDGE_LOOP ( 'NONE', ( #95741, #69457 ) ) ;
#91611 = CARTESIAN_POINT ( 'NONE',  ( -13.14999999999999147, 2.500000000000000000, -1.718653347947323828 ) ) ;
#91612 = EDGE_CURVE ( 'NONE', #85023, #106593, #108791, .T. ) ;
#91613 = VERTEX_POINT ( 'NONE', #97003 ) ;
#91614 = AXIS2_PLACEMENT_3D ( 'NONE', #24161, #73900, #42533 ) ;
#91615 = CARTESIAN_POINT ( 'NONE',  ( 13.14999999999989733, 12.50000000000000000, -1.818653347947325916 ) ) ;
#91616 = CARTESIAN_POINT ( 'NONE',  ( 1.449999999999949551, 2.500000000000000000, 6.841600689897072485 ) ) ;
#91617 = ORIENTED_EDGE ( 'NONE', *, *, #105416, .T. ) ;
#91618 = AXIS2_PLACEMENT_3D ( 'NONE', #91709, #104106, #1385 ) ;
#91619 = CARTESIAN_POINT ( 'NONE',  ( -10.60000000000000320, 12.50000000000000000, -4.676537180435973440 ) ) ;
#91620 = DIRECTION ( 'NONE',  ( -0.000000000000000000, -1.000000000000000000, -0.000000000000000000 ) ) ;
#91621 = CONICAL_SURFACE ( 'NONE', #99946, 0.1000000000000000472, 0.003490658503988666988 ) ;
#91622 = AXIS2_PLACEMENT_3D ( 'NONE', #5189, #34690, #27402 ) ;
#91623 = DIRECTION ( 'NONE',  ( 0.000000000000000000, 0.000000000000000000, 1.000000000000000000 ) ) ;
#91624 = VERTEX_POINT ( 'NONE', #48555 ) ;
#91625 = ORIENTED_EDGE ( 'NONE', *, *, #72682, .F. ) ;
#91626 = EDGE_CURVE ( 'NONE', #24362, #56014, #78670, .T. ) ;
#91627 = DIRECTION ( 'NONE',  ( 0.000000000000000000, 0.000000000000000000, -1.000000000000000000 ) ) ;
#91629 = EDGE_LOOP ( 'NONE', ( #34856, #20835 ) ) ;
#91628 = AXIS2_PLACEMENT_3D ( 'NONE', #115956, #76680, #55742 ) ;
#91630 = DIRECTION ( 'NONE',  ( 0.000000000000000000, 0.000000000000000000, -1.000000000000000000 ) ) ;
#91631 = DIRECTION ( 'NONE',  ( 0.000000000000000000, 1.000000000000000000, 0.000000000000000000 ) ) ;
#91632 = CIRCLE ( 'NONE', #33159, 0.06509327318403743123 ) ;
#91633 = CIRCLE ( 'NONE', #16387, 0.09999999999999999167 ) ;
#91634 = DIRECTION ( 'NONE',  ( 0.000000000000000000, -0.9999939076577903929, 0.003490651415223739937 ) ) ;
#91635 = ORIENTED_EDGE ( 'NONE', *, *, #90188, .T. ) ;
#91636 = DIRECTION ( 'NONE',  ( 0.000000000000000000, 0.000000000000000000, 1.000000000000000000 ) ) ;
#91637 = CARTESIAN_POINT ( 'NONE',  ( 12.09999999999990550, 2.500000000000000000, 4.330127018922196314 ) ) ;
#91638 = DIRECTION ( 'NONE',  ( 0.000000000000000000, 0.000000000000000000, 1.000000000000000000 ) ) ;
#91639 = LINE ( 'NONE', #30811, #99817 ) ;
#91640 = FACE_OUTER_BOUND ( 'NONE', #6965, .T. ) ;
#91641 = DIRECTION ( 'NONE',  ( 0.000000000000000000, 1.000000000000000000, 0.000000000000000000 ) ) ;
#91642 = AXIS2_PLACEMENT_3D ( 'NONE', #75166, #3839, #35252 ) ;
#91643 = ORIENTED_EDGE ( 'NONE', *, *, #106022, .T. ) ;
#91645 = EDGE_LOOP ( 'NONE', ( #26691, #24636, #45544, #53855 ) ) ;
#91644 = CONICAL_SURFACE ( 'NONE', #100063, 0.1000000000000002554, 0.003490658503988666988 ) ;
#91646 = FACE_OUTER_BOUND ( 'NONE', #25138, .T. ) ;
#91647 = VERTEX_POINT ( 'NONE', #87170 ) ;
#91648 = CARTESIAN_POINT ( 'NONE',  ( 103.4640010755897919, 7.406936539094362892, 2.109949502027294255 ) ) ;
#91650 = VERTEX_POINT ( 'NONE', #98282 ) ;
#91649 = ORIENTED_EDGE ( 'NONE', *, *, #124232, .T. ) ;
#91651 = VERTEX_POINT ( 'NONE', #68175 ) ;
#91652 = CARTESIAN_POINT ( 'NONE',  ( 8.549999999999918998, 12.50000000000000000, 6.906693963081109722 ) ) ;
#91654 = CARTESIAN_POINT ( 'NONE',  ( 7.099999999999928590, 12.50000000000000000, -5.022947341949754119 ) ) ;
#91653 = CONICAL_SURFACE ( 'NONE', #89505, 0.1000000000000002554, 0.003490658503988666988 ) ;
#91655 = CARTESIAN_POINT ( 'NONE',  ( 3.349999999999944578, 12.50000000000000000, -1.472243186433550122 ) ) ;
#91656 = EDGE_CURVE ( 'NONE', #78690, #14821, #25176, .T. ) ;
#91657 = FILL_AREA_STYLE ('',( #100816 ) ) ;
#91658 = DIRECTION ( 'NONE',  ( 0.000000000000000000, 0.000000000000000000, 1.000000000000000000 ) ) ;
#91659 = DIRECTION ( 'NONE',  ( 0.000000000000000000, 1.000000000000000000, 0.000000000000000000 ) ) ;
#91660 = DIRECTION ( 'NONE',  ( 0.000000000000000000, 1.000000000000000000, 0.000000000000000000 ) ) ;
#91661 = DIRECTION ( 'NONE',  ( 0.000000000000000000, -0.000000000000000000, 1.000000000000000000 ) ) ;
#91662 = CIRCLE ( 'NONE', #35241, 0.1000000000000002554 ) ;
#91663 = CARTESIAN_POINT ( 'NONE',  ( -10.65000000000000213, 2.500000000000000000, 2.511473670974873507 ) ) ;
#91664 = DIRECTION ( 'NONE',  ( 0.000000000000000000, 1.000000000000000000, 0.000000000000000000 ) ) ;
#91665 = EDGE_CURVE ( 'NONE', #15249, #70431, #117255, .T. ) ;
#91666 = AXIS2_PLACEMENT_3D ( 'NONE', #111825, #41810, #92166 ) ;
#91667 = VERTEX_POINT ( 'NONE', #8597 ) ;
#91668 = STYLED_ITEM ( 'NONE', ( #13727 ), #50879 ) ;
#91669 = DIRECTION ( 'NONE',  ( -4.274815082592931898E-19, -0.9999939076577903929, -0.003490651415223739937 ) ) ;
#91670 = EDGE_CURVE ( 'NONE', #2963, #121075, #118567, .T. ) ;
#91671 = ORIENTED_EDGE ( 'NONE', *, *, #67113, .F. ) ;
#91672 = ADVANCED_FACE ( 'NONE', ( #67518 ), #67020, .T. ) ;
#91673 = ORIENTED_EDGE ( 'NONE', *, *, #93893, .F. ) ;
#91674 = EDGE_CURVE ( 'NONE', #51834, #585, #9271, .T. ) ;
#91675 = FACE_OUTER_BOUND ( 'NONE', #124975, .T. ) ;
#91677 = ADVANCED_FACE ( 'NONE', ( #129069 ), #87810, .T. ) ;
#91676 = CARTESIAN_POINT ( 'NONE',  ( 10.19999999999991402, 2.500000000000000000, 0.3464101615137735735 ) ) ;
#91678 = DIRECTION ( 'NONE',  ( -0.000000000000000000, 1.000000000000000000, -0.000000000000000000 ) ) ;
#91679 = CARTESIAN_POINT ( 'NONE',  ( 11.64999999999990443, 2.500000000000000000, 1.472243186433545459 ) ) ;
#91680 = CARTESIAN_POINT ( 'NONE',  ( 1.899999999999951283, 2.500000000000000000, -4.576537180435977348 ) ) ;
#91681 = CARTESIAN_POINT ( 'NONE',  ( 2.499999999999983569, 2.500000000000000000, -4.430127018922202176 ) ) ;
#91682 = EDGE_CURVE ( 'NONE', #45181, #73774, #33603, .T. ) ;
#91683 = CARTESIAN_POINT ( 'NONE',  ( 5.599999999999934808, 12.50000000000000000, -3.983716857408426293 ) ) ;
#91684 = EDGE_LOOP ( 'NONE', ( #93010, #128617, #41633, #115553 ) ) ;
#91685 = ADVANCED_FACE ( 'NONE', ( #39402 ), #19747, .T. ) ;
#91686 = AXIS2_PLACEMENT_3D ( 'NONE', #47205, #56362, #106117 ) ;
#91687 = EDGE_CURVE ( 'NONE', #23602, #119523, #104680, .T. ) ;
#91688 = EDGE_CURVE ( 'NONE', #126431, #65030, #91050, .T. ) ;
#91689 = VERTEX_POINT ( 'NONE', #40691 ) ;
#91690 = ADVANCED_FACE ( 'NONE', ( #92329 ), #31541, .T. ) ;
#91691 = ORIENTED_EDGE ( 'NONE', *, *, #24132, .T. ) ;
#91692 = CONICAL_SURFACE ( 'NONE', #51991, 0.09999999999999982514, 0.003490658503988666988 ) ;
#91693 = ORIENTED_EDGE ( 'NONE', *, *, #43928, .F. ) ;
#91694 = AXIS2_PLACEMENT_3D ( 'NONE', #32559, #109139, #119613 ) ;
#91695 = EDGE_LOOP ( 'NONE', ( #115687, #114503, #17588, #116124 ) ) ;
#91696 = EDGE_CURVE ( 'NONE', #39901, #114154, #115048, .T. ) ;
#91697 = CARTESIAN_POINT ( 'NONE',  ( -1.900000000000034106, 12.50000000000000000, -3.918623584224389056 ) ) ;
#91698 = DIRECTION ( 'NONE',  ( 0.000000000000000000, 0.000000000000000000, -1.000000000000000000 ) ) ;
#91700 = CIRCLE ( 'NONE', #56178, 0.06509327318403745899 ) ;
#91699 = CONICAL_SURFACE ( 'NONE', #22764, 0.09999999999999999167, 0.003490658503988666988 ) ;
#91701 = CARTESIAN_POINT ( 'NONE',  ( -7.100000000000018296, 2.500000000000000000, -4.330127018922201643 ) ) ;
#91702 = CARTESIAN_POINT ( 'NONE',  ( -3.350000000000028511, 2.500000000000000000, 1.372243186433545370 ) ) ;
#91703 = CARTESIAN_POINT ( 'NONE',  ( 12.29999999999990479, 2.500000000000000000, 4.576537180435972019 ) ) ;
#91704 = VERTEX_POINT ( 'NONE', #91697 ) ;
#91705 = DIRECTION ( 'NONE',  ( -0.000000000000000000, 1.000000000000000000, -0.000000000000000000 ) ) ;
#91706 = CARTESIAN_POINT ( 'NONE',  ( -7.700000000000012612, 2.500000000000000000, 4.676537180435972552 ) ) ;
#91707 = DIRECTION ( 'NONE',  ( 0.000000000000000000, 0.000000000000000000, 1.000000000000000000 ) ) ;
#91708 = DIRECTION ( 'NONE',  ( -0.000000000000000000, 1.000000000000000000, -0.000000000000000000 ) ) ;
#91709 = CARTESIAN_POINT ( 'NONE',  ( 3.349999999999945466, 12.50000000000000000, -2.857883832488653741 ) ) ;
#91710 = ORIENTED_EDGE ( 'NONE', *, *, #94040, .T. ) ;
#91711 = ORIENTED_EDGE ( 'NONE', *, *, #108801, .F. ) ;
#91712 = VERTEX_POINT ( 'NONE', #111306 ) ;
#91713 = FACE_OUTER_BOUND ( 'NONE', #120129, .T. ) ;
#91714 = ORIENTED_EDGE ( 'NONE', *, *, #55153, .T. ) ;
#91715 = LINE ( 'NONE', #71411, #109375 ) ;
#91716 = CARTESIAN_POINT ( 'NONE',  ( 13.29999999999989946, 2.500000000000000000, 0.09999999999999761857 ) ) ;
#91717 = AXIS2_PLACEMENT_3D ( 'NONE', #79175, #39895, #39263 ) ;
#91718 = CIRCLE ( 'NONE', #112652, 0.09999999999999982514 ) ;
#91719 = CIRCLE ( 'NONE', #35297, 0.1000000000000002554 ) ;
#91720 = ORIENTED_EDGE ( 'NONE', *, *, #23703, .T. ) ;
#91721 = DIRECTION ( 'NONE',  ( 0.000000000000000000, 1.000000000000000000, 0.000000000000000000 ) ) ;
#91722 = CARTESIAN_POINT ( 'NONE',  ( 3.549999999999943867, 2.500000000000000000, -1.818653347947326138 ) ) ;
#91723 = FACE_OUTER_BOUND ( 'NONE', #121885, .T. ) ;
#91724 = LINE ( 'NONE', #123122, #110327 ) ;
#91725 = AXIS2_PLACEMENT_3D ( 'NONE', #11659, #10999, #100048 ) ;
#91726 = ADVANCED_FACE ( 'NONE', ( #11187 ), #113007, .T. ) ;
#91727 = CIRCLE ( 'NONE', #29055, 0.06509327318403745899 ) ;
#91728 = CARTESIAN_POINT ( 'NONE',  ( 7.099999999999928590, 12.50000000000000000, 3.637306695894644726 ) ) ;
#91729 = ADVANCED_FACE ( 'NONE', ( #62885 ), #100230, .T. ) ;
#91730 = ORIENTED_EDGE ( 'NONE', *, *, #38142, .T. ) ;
#91731 = VERTEX_POINT ( 'NONE', #79936 ) ;
#91732 = CARTESIAN_POINT ( 'NONE',  ( -6.650000000000018119, 2.500000000000000000, -6.495190528383302464 ) ) ;
#91733 = AXIS2_PLACEMENT_3D ( 'NONE', #17347, #76295, #8186 ) ;
#91734 = CARTESIAN_POINT ( 'NONE',  ( -7.500000000000015099, 12.50000000000000000, -0.6928203230275541413 ) ) ;
#91735 = ADVANCED_FACE ( 'NONE', ( #42616 ), #96264, .T. ) ;
#91736 = CARTESIAN_POINT ( 'NONE',  ( 1.849999999999948130, 2.500000000000000000, 6.148780366869520009 ) ) ;
#91737 = VERTEX_POINT ( 'NONE', #61607 ) ;
#91738 = EDGE_CURVE ( 'NONE', #72025, #71464, #82535, .T. ) ;
#91739 = ORIENTED_EDGE ( 'NONE', *, *, #42936, .F. ) ;
#91740 = CARTESIAN_POINT ( 'NONE',  ( 8.149999999999923972, 2.500000000000000000, 1.818653347947321475 ) ) ;
#91741 = DIRECTION ( 'NONE',  ( -0.000000000000000000, -1.000000000000000000, -0.000000000000000000 ) ) ;
#91742 = DIRECTION ( 'NONE',  ( 0.000000000000000000, 1.000000000000000000, 0.000000000000000000 ) ) ;
#91743 = CARTESIAN_POINT ( 'NONE',  ( 108.0000000000000142, 8.500000000000000000, 0.000000000000000000 ) ) ;
#91744 = ORIENTED_EDGE ( 'NONE', *, *, #20285, .F. ) ;
#91745 = AXIS2_PLACEMENT_3D ( 'NONE', #58794, #9031, #88897 ) ;
#91746 = DIRECTION ( 'NONE',  ( 0.000000000000000000, 0.000000000000000000, 1.000000000000000000 ) ) ;
#91747 = DIRECTION ( 'NONE',  ( 0.000000000000000000, -0.9999939076577903929, 0.003490651415223739937 ) ) ;
#91748 = VECTOR ( 'NONE', #127450, 1000.000000000000000 ) ;
#91749 = EDGE_LOOP ( 'NONE', ( #66262, #92635, #115972, #128213 ) ) ;
#91750 = CARTESIAN_POINT ( 'NONE',  ( -6.700000000000016165, 12.50000000000000000, 4.395220292106234439 ) ) ;
#91751 = EDGE_LOOP ( 'NONE', ( #9107, #54848, #58050, #52422 ) ) ;
#91752 = PLANE ( 'NONE',  #18157 ) ;
#91753 = ORIENTED_EDGE ( 'NONE', *, *, #95399, .T. ) ;
#91754 = CIRCLE ( 'NONE', #87542, 0.1000000000000002554 ) ;
#91755 = CARTESIAN_POINT ( 'NONE',  ( 13.34999999999990017, 12.50000000000000000, 2.165063509461097713 ) ) ;
#91756 = DIRECTION ( 'NONE',  ( 0.000000000000000000, 0.000000000000000000, -1.000000000000000000 ) ) ;
#91757 = EDGE_LOOP ( 'NONE', ( #57693, #102746, #97944, #44820 ) ) ;
#91758 = ORIENTED_EDGE ( 'NONE', *, *, #19265, .F. ) ;
#91759 = DIRECTION ( 'NONE',  ( -0.000000000000000000, 1.000000000000000000, -0.000000000000000000 ) ) ;
#91760 = FACE_OUTER_BOUND ( 'NONE', #50740, .T. ) ;
#91761 = VECTOR ( 'NONE', #47408, 1000.000000000000000 ) ;
#91763 = EDGE_CURVE ( 'NONE', #54102, #118, #127671, .T. ) ;
#91762 = CARTESIAN_POINT ( 'NONE',  ( 186.7552083336747444, 6.551208109652275624, -3.782341765624998686 ) ) ;
#91764 = CARTESIAN_POINT ( 'NONE',  ( 184.6093750003413732, 9.264065473108010111E-16, -7.564683531250000925 ) ) ;
#91765 = CIRCLE ( 'NONE', #112617, 3.000000000000000444 ) ;
#91766 = FACE_OUTER_BOUND ( 'NONE', #120854, .T. ) ;
#91767 = CARTESIAN_POINT ( 'NONE',  ( 9.399999999999915090, 12.50000000000000000, -4.676537180435977881 ) ) ;
#91768 = CARTESIAN_POINT ( 'NONE',  ( -2.900000000000029665, 2.500000000000000000, 4.430127018922196847 ) ) ;
#91769 = CARTESIAN_POINT ( 'NONE',  ( 2.299999999999947864, 12.50000000000000000, 3.983716857408420964 ) ) ;
#91770 = DIRECTION ( 'NONE',  ( 0.000000000000000000, 0.000000000000000000, -1.000000000000000000 ) ) ;
#91771 = VECTOR ( 'NONE', #90015, 1000.000000000000000 ) ;
#91772 = VERTEX_POINT ( 'NONE', #30219 ) ;
#91773 = VERTEX_POINT ( 'NONE', #50478 ) ;
#91774 = CARTESIAN_POINT ( 'NONE',  ( 108.0000000000000142, 8.500000000000000000, 0.2500000000000000000 ) ) ;
#91776 = VECTOR ( 'NONE', #99485, 1000.000000000000000 ) ;
#91775 = CIRCLE ( 'NONE', #81321, 0.06509327318403745899 ) ;
#91777 = VERTEX_POINT ( 'NONE', #30860 ) ;
#91778 = CARTESIAN_POINT ( 'NONE',  ( 6.649999999999928413, 12.50000000000000000, 2.792790559304612064 ) ) ;
#91779 = DIRECTION ( 'NONE',  ( 0.000000000000000000, 0.000000000000000000, 1.000000000000000000 ) ) ;
#91780 = EDGE_CURVE ( 'NONE', #85421, #9409, #37797, .T. ) ;
#91781 = DIRECTION ( 'NONE',  ( 0.000000000000000000, -0.9999939076577903929, 0.003490651415223739937 ) ) ;
#91782 = CIRCLE ( 'NONE', #79285, 0.06509327318403745899 ) ;
#91784 = VERTEX_POINT ( 'NONE', #122455 ) ;
#91783 = ORIENTED_EDGE ( 'NONE', *, *, #26133, .T. ) ;
#91785 = FACE_BOUND ( 'NONE', #94070, .T. ) ;
#91786 = ORIENTED_EDGE ( 'NONE', *, *, #99580, .F. ) ;
#91787 = ADVANCED_FACE ( 'NONE', ( #726 ), #120515, .T. ) ;
#91788 = CARTESIAN_POINT ( 'NONE',  ( 13.09999999999990195, 2.500000000000000000, 4.676537180435972552 ) ) ;
#91789 = DIRECTION ( 'NONE',  ( -0.000000000000000000, 1.000000000000000000, -0.000000000000000000 ) ) ;
#91790 = DIRECTION ( 'NONE',  ( 0.000000000000000000, -0.000000000000000000, 1.000000000000000000 ) ) ;
#91793 = CARTESIAN_POINT ( 'NONE',  ( 10.84999999999990905, 2.500000000000000000, 2.957883832488649389 ) ) ;
#91792 = CIRCLE ( 'NONE', #4042, 0.09999999999999982514 ) ;
#91791 = CIRCLE ( 'NONE', #108507, 0.1000000000000002554 ) ;
#91794 = FACE_OUTER_BOUND ( 'NONE', #105666, .T. ) ;
#91795 = DIRECTION ( 'NONE',  ( 0.000000000000000000, 0.000000000000000000, -1.000000000000000000 ) ) ;
#91796 = FACE_OUTER_BOUND ( 'NONE', #90569, .T. ) ;
#91797 = DIRECTION ( 'NONE',  ( 1.000000000000000000, 0.000000000000000000, 0.000000000000000000 ) ) ;
#91798 = EDGE_CURVE ( 'NONE', #11533, #86367, #6367, .T. ) ;
#91799 = DIRECTION ( 'NONE',  ( 0.000000000000000000, 0.000000000000000000, 1.000000000000000000 ) ) ;
#91800 = DIRECTION ( 'NONE',  ( -0.000000000000000000, -1.000000000000000000, -0.000000000000000000 ) ) ;
#91801 = DIRECTION ( 'NONE',  ( 0.000000000000000000, 0.000000000000000000, -1.000000000000000000 ) ) ;
#91802 = ORIENTED_EDGE ( 'NONE', *, *, #59633, .T. ) ;
#91803 = ORIENTED_EDGE ( 'NONE', *, *, #15376, .F. ) ;
#91804 = ORIENTED_EDGE ( 'NONE', *, *, #126536, .T. ) ;
#91805 = CARTESIAN_POINT ( 'NONE',  ( 9.399999999999918643, 2.500000000000000000, -0.3464101615137782364 ) ) ;
#91806 = EDGE_LOOP ( 'NONE', ( #24992, #12096, #89079, #2993 ) ) ;
#91807 = FACE_OUTER_BOUND ( 'NONE', #35660, .T. ) ;
#91808 = CARTESIAN_POINT ( 'NONE',  ( -3.749999999999991118, 12.50000000000000000, 2.165063509461097713 ) ) ;
#91810 = ORIENTED_EDGE ( 'NONE', *, *, #16427, .F. ) ;
#91809 = VERTEX_POINT ( 'NONE', #110680 ) ;
#91811 = ORIENTED_EDGE ( 'NONE', *, *, #21326, .F. ) ;
#91812 = DIRECTION ( 'NONE',  ( -0.000000000000000000, 1.000000000000000000, -0.000000000000000000 ) ) ;
#91813 = AXIS2_PLACEMENT_3D ( 'NONE', #61469, #1875, #121647 ) ;
#91814 = CIRCLE ( 'NONE', #75088, 0.06509327318403745899 ) ;
#91815 = CARTESIAN_POINT ( 'NONE',  ( 7.949999999999925571, 2.500000000000000000, 2.065063509461097624 ) ) ;
#91816 = SURFACE_STYLE_USAGE ( .BOTH. , #111439 ) ;
#91817 = FACE_OUTER_BOUND ( 'NONE', #99306, .T. ) ;
#91818 = CARTESIAN_POINT ( 'NONE',  ( 3.949999999999941558, 2.500000000000000000, -1.918653347947326004 ) ) ;
#91819 = LINE ( 'NONE', #44655, #47677 ) ;
#91820 = DIRECTION ( 'NONE',  ( 0.000000000000000000, 0.000000000000000000, 1.000000000000000000 ) ) ;
#91821 = VERTEX_POINT ( 'NONE', #21015 ) ;
#91822 = AXIS2_PLACEMENT_3D ( 'NONE', #7493, #47437, #127290 ) ;
#91824 = CARTESIAN_POINT ( 'NONE',  ( 7.299999999999926104, 2.500000000000000000, -0.3464101615137782364 ) ) ;
#91823 = VECTOR ( 'NONE', #6964, 1000.000000000000000 ) ;
#91825 = ORIENTED_EDGE ( 'NONE', *, *, #54605, .T. ) ;
#91826 = EDGE_CURVE ( 'NONE', #123530, #81523, #2010, .T. ) ;
#91827 = AXIS2_PLACEMENT_3D ( 'NONE', #83765, #113213, #121749 ) ;
#91828 = ORIENTED_EDGE ( 'NONE', *, *, #108089, .F. ) ;
#91829 = ORIENTED_EDGE ( 'NONE', *, *, #39988, .F. ) ;
#91830 = CARTESIAN_POINT ( 'NONE',  ( 14.99999999999989164, 2.500000000000000000, 0.6928203230275494784 ) ) ;
#91831 = EDGE_LOOP ( 'NONE', ( #12322, #15971, #101394, #39933 ) ) ;
#91832 = ADVANCED_FACE ( 'NONE', ( #100853 ), #121784, .F. ) ;
#91833 = EDGE_LOOP ( 'NONE', ( #22285, #3754, #90112, #13470 ) ) ;
#91834 = ADVANCED_FACE ( 'NONE', ( #111988 ), #87947, .T. ) ;
#91835 = ORIENTED_EDGE ( 'NONE', *, *, #49588, .F. ) ;
#91837 = EDGE_CURVE ( 'NONE', #82761, #62966, #39876, .T. ) ;
#91836 = CIRCLE ( 'NONE', #108553, 0.1000000000000000472 ) ;
#91838 = AXIS2_PLACEMENT_3D ( 'NONE', #32339, #123896, #123265 ) ;
#91839 = FACE_OUTER_BOUND ( 'NONE', #5269, .T. ) ;
#91840 = DIRECTION ( 'NONE',  ( 0.000000000000000000, 0.000000000000000000, 1.000000000000000000 ) ) ;
#91841 = DIRECTION ( 'NONE',  ( -4.274815082592931898E-19, -0.9999939076577903929, -0.003490651415223739937 ) ) ;
#91842 = CARTESIAN_POINT ( 'NONE',  ( 6.249999999999930722, 12.50000000000000000, 7.188010851410848723 ) ) ;
#91843 = EDGE_CURVE ( 'NONE', #20339, #60435, #45826, .T. ) ;
#91844 = FACE_OUTER_BOUND ( 'NONE', #127100, .T. ) ;
#91845 = EDGE_CURVE ( 'NONE', #20279, #78706, #3950, .T. ) ;
#91846 = EDGE_CURVE ( 'NONE', #100903, #65296, #83766, .T. ) ;
#91847 = CARTESIAN_POINT ( 'NONE',  ( -6.700000000000019718, 2.500000000000000000, -2.385244779468109755E-15 ) ) ;
#91848 = ORIENTED_EDGE ( 'NONE', *, *, #37363, .T. ) ;
#91849 = DIRECTION ( 'NONE',  ( 0.000000000000000000, -0.9999939076577903929, 0.003490651415223739937 ) ) ;
#91850 = EDGE_CURVE ( 'NONE', #59573, #113873, #71238, .T. ) ;
#91851 = ORIENTED_EDGE ( 'NONE', *, *, #60211, .T. ) ;
#91852 = CARTESIAN_POINT ( 'NONE',  ( -8.300000000000009592, 2.500000000000000000, 4.230127018922196669 ) ) ;
#91853 = AXIS2_PLACEMENT_3D ( 'NONE', #15959, #17239, #55269 ) ;
#91854 = EDGE_LOOP ( 'NONE', ( #16056, #10837, #28090, #125817 ) ) ;
#91855 = CARTESIAN_POINT ( 'NONE',  ( 4.999999999999933387, 12.50000000000000000, 4.957854068765711553 ) ) ;
#91856 = ADVANCED_FACE ( 'NONE', ( #35362 ), #44058, .T. ) ;
#91857 = ORIENTED_EDGE ( 'NONE', *, *, #126370, .T. ) ;
#91858 = EDGE_CURVE ( 'NONE', #102274, #46680, #60787, .T. ) ;
#91859 = CARTESIAN_POINT ( 'NONE',  ( 184.6510416670080588, 4.367472073101518859, -7.564683531249999149 ) ) ;
#91860 = CARTESIAN_POINT ( 'NONE',  ( 11.84999999999990372, 2.500000000000000000, -6.048780366869526581 ) ) ;
#91861 = VERTEX_POINT ( 'NONE', #55637 ) ;
#91862 = ORIENTED_EDGE ( 'NONE', *, *, #23975, .T. ) ;
#91863 =( BOUNDED_CURVE ( )  B_SPLINE_CURVE ( 2, ( #57201, #76850, #107593, #6778, #116753, #27102, #127244 ),
 .UNSPECIFIED., .F., .F. ) 
 B_SPLINE_CURVE_WITH_KNOTS ( ( 3, 2, 2, 3 ),
 ( 0.000000000000000000, 0.02380952380952383249, 0.04761904761904766498, 0.07142857142857149400 ),
 .UNSPECIFIED. ) 
 CURVE ( )  GEOMETRIC_REPRESENTATION_ITEM ( )  RATIONAL_B_SPLINE_CURVE ( ( 1.000000000000000000, 0.8660254037844387076, 1.000000000000000000, 0.8660254037844387076, 1.000000000000000000, 0.8660254037844383745, 1.000000000000000444 ) ) 
 REPRESENTATION_ITEM ( '' )  );
#91864 = LINE ( 'NONE', #2178, #125016 ) ;
#91865 = CARTESIAN_POINT ( 'NONE',  ( -9.350000000000008527, 2.500000000000000000, -6.741600689897071952 ) ) ;
#91866 = CARTESIAN_POINT ( 'NONE',  ( 11.24999999999991118, 2.500000000000000000, -2.857883832488653741 ) ) ;
#91868 = AXIS2_PLACEMENT_3D ( 'NONE', #10056, #1509, #41471 ) ;
#91867 = CARTESIAN_POINT ( 'NONE',  ( -7.100000000000014744, 12.50000000000000000, 4.330127018922196314 ) ) ;
#91869 = CARTESIAN_POINT ( 'NONE',  ( 10.59999999999991260, 2.500000000000000000, 0.2464101615137735679 ) ) ;
#91870 = ORIENTED_EDGE ( 'NONE', *, *, #95048, .T. ) ;
#91871 = DIRECTION ( 'NONE',  ( 0.000000000000000000, 0.000000000000000000, 1.000000000000000000 ) ) ;
#91872 = AXIS2_PLACEMENT_3D ( 'NONE', #108861, #8716, #27727 ) ;
#91873 = ORIENTED_EDGE ( 'NONE', *, *, #54390, .F. ) ;
#91874 = DIRECTION ( 'NONE',  ( 0.000000000000000000, -0.000000000000000000, 1.000000000000000000 ) ) ;
#91875 = CARTESIAN_POINT ( 'NONE',  ( -2.050000000000033129, 2.500000000000000000, 2.265063509461097357 ) ) ;
#91876 = AXIS2_PLACEMENT_3D ( 'NONE', #96673, #49546, #128763 ) ;
#91877 = AXIS2_PLACEMENT_3D ( 'NONE', #105635, #66339, #15936 ) ;
#91878 = DIRECTION ( 'NONE',  ( -0.000000000000000000, 1.000000000000000000, -0.000000000000000000 ) ) ;
#91879 = CARTESIAN_POINT ( 'NONE',  ( 8.349999999999919709, 2.500000000000000000, 7.088010851410848190 ) ) ;
#91880 = CARTESIAN_POINT ( 'NONE',  ( -9.350000000000006750, 12.50000000000000000, -1.818653347947325916 ) ) ;
#91881 = DIRECTION ( 'NONE',  ( 0.000000000000000000, 0.000000000000000000, 1.000000000000000000 ) ) ;
#91882 = DIRECTION ( 'NONE',  ( 0.000000000000000000, 0.000000000000000000, 1.000000000000000000 ) ) ;
#91883 = ORIENTED_EDGE ( 'NONE', *, *, #75701, .F. ) ;
#91885 = VECTOR ( 'NONE', #111351, 1000.000000000000000 ) ;
#91884 = STYLED_ITEM ( 'NONE', ( #2320 ), #100344 ) ;
#91887 = EDGE_CURVE ( 'NONE', #96815, #49458, #111021, .T. ) ;
#91886 = FACE_OUTER_BOUND ( 'NONE', #63896, .T. ) ;
#91888 = CARTESIAN_POINT ( 'NONE',  ( 13.09999999999990195, 12.50000000000000000, 4.741630453620009789 ) ) ;
#91889 = DIRECTION ( 'NONE',  ( 0.000000000000000000, 0.000000000000000000, -1.000000000000000000 ) ) ;
#91890 = EDGE_CURVE ( 'NONE', #54921, #103269, #73989, .T. ) ;
#91891 = ORIENTED_EDGE ( 'NONE', *, *, #56497, .F. ) ;
#91892 = ORIENTED_EDGE ( 'NONE', *, *, #72327, .T. ) ;
#91893 = CARTESIAN_POINT ( 'NONE',  ( 5.649999999999936406, 12.50000000000000000, -6.776507416713039689 ) ) ;
#91894 = ORIENTED_EDGE ( 'NONE', *, *, #47474, .F. ) ;
#91895 = ORIENTED_EDGE ( 'NONE', *, *, #66107, .F. ) ;
#91896 = DIRECTION ( 'NONE',  ( 0.000000000000000000, 0.000000000000000000, 1.000000000000000000 ) ) ;
#91897 = VECTOR ( 'NONE', #36257, 1000.000000000000000 ) ;
#91898 = ORIENTED_EDGE ( 'NONE', *, *, #76769, .F. ) ;
#91899 = CARTESIAN_POINT ( 'NONE',  ( -6.250000000000021316, 12.50000000000000000, -5.867463478539787225 ) ) ;
#91900 = LINE ( 'NONE', #42157, #59198 ) ;
#91901 = DIRECTION ( 'NONE',  ( 0.000000000000000000, 0.000000000000000000, 1.000000000000000000 ) ) ;
#91902 = ORIENTED_EDGE ( 'NONE', *, *, #24505, .F. ) ;
#91903 = AXIS2_PLACEMENT_3D ( 'NONE', #83362, #53895, #123279 ) ;
#91904 = FACE_OUTER_BOUND ( 'NONE', #37648, .T. ) ;
#91905 = CIRCLE ( 'NONE', #108619, 0.09999999999999982514 ) ;
#91906 = DIRECTION ( 'NONE',  ( -0.000000000000000000, -1.000000000000000000, -0.000000000000000000 ) ) ;
#91907 = CIRCLE ( 'NONE', #39615, 0.1000000000000002554 ) ;
#91908 = VERTEX_POINT ( 'NONE', #64804 ) ;
#91910 = CIRCLE ( 'NONE', #37640, 0.06509327318403745899 ) ;
#91909 = AXIS2_PLACEMENT_3D ( 'NONE', #92002, #94568, #24550 ) ;
#91911 = ORIENTED_EDGE ( 'NONE', *, *, #110806, .T. ) ;
#91912 = ORIENTED_EDGE ( 'NONE', *, *, #30549, .T. ) ;
#91913 = PLANE ( 'NONE',  #102824 ) ;
#91914 = DIRECTION ( 'NONE',  ( 0.000000000000000000, -0.000000000000000000, 1.000000000000000000 ) ) ;
#91915 = CARTESIAN_POINT ( 'NONE',  ( 2.699999999999947331, 2.500000000000000000, -4.576537180435978236 ) ) ;
#91916 = FACE_BOUND ( 'NONE', #94533, .T. ) ;
#91917 = EDGE_LOOP ( 'NONE', ( #91214, #55576 ) ) ;
#91918 = VECTOR ( 'NONE', #49925, 1000.000000000000000 ) ;
#91919 = CARTESIAN_POINT ( 'NONE',  ( 7.699999999999923794, 2.500000000000000000, 4.676537180435972552 ) ) ;
#91920 = DIRECTION ( 'NONE',  ( 0.000000000000000000, 0.000000000000000000, 1.000000000000000000 ) ) ;
#91921 = EDGE_LOOP ( 'NONE', ( #12099, #33551 ) ) ;
#91924 = ADVANCED_FACE ( 'NONE', ( #36005 ), #73384, .T. ) ;
#91923 = DIRECTION ( 'NONE',  ( 0.000000000000000000, 1.000000000000000000, 0.000000000000000000 ) ) ;
#91922 = AXIS2_PLACEMENT_3D ( 'NONE', #112807, #23129, #13293 ) ;
#91925 = FACE_OUTER_BOUND ( 'NONE', #59967, .T. ) ;
#91926 = AXIS2_PLACEMENT_3D ( 'NONE', #53908, #14601, #124584 ) ;
#91927 = CARTESIAN_POINT ( 'NONE',  ( -9.600000000000008527, 12.50000000000000000, 4.330127018922196314 ) ) ;
#91928 = LINE ( 'NONE', #53304, #59678 ) ;
#91929 = CARTESIAN_POINT ( 'NONE',  ( 129.5000000000000000, 0.000000000000000000, 6.000000000000000000 ) ) ;
#91930 = DIRECTION ( 'NONE',  ( 0.000000000000000000, -0.000000000000000000, 1.000000000000000000 ) ) ;
#91931 = CARTESIAN_POINT ( 'NONE',  ( 10.19999999999991225, 2.500000000000000000, 3.983716857408420076 ) ) ;
#91932 = VECTOR ( 'NONE', #24279, 1000.000000000000000 ) ;
#91933 = EDGE_CURVE ( 'NONE', #115197, #28423, #75913, .T. ) ;
#91934 = EDGE_LOOP ( 'NONE', ( #31044, #31410 ) ) ;
#91935 = ORIENTED_EDGE ( 'NONE', *, *, #39860, .F. ) ;
#91936 = ORIENTED_EDGE ( 'NONE', *, *, #5337, .F. ) ;
#91937 = VERTEX_POINT ( 'NONE', #93630 ) ;
#91938 = CONICAL_SURFACE ( 'NONE', #16613, 0.1000000000000000472, 0.003490658503988666988 ) ;
#91939 = DIRECTION ( 'NONE',  ( 0.000000000000000000, 0.000000000000000000, -1.000000000000000000 ) ) ;
#91940 = ADVANCED_FACE ( 'NONE', ( #92995 ), #104717, .T. ) ;
#91941 = DIRECTION ( 'NONE',  ( 0.000000000000000000, 0.000000000000000000, -1.000000000000000000 ) ) ;
#91942 = ORIENTED_EDGE ( 'NONE', *, *, #44430, .F. ) ;
#91943 = FACE_BOUND ( 'NONE', #102300, .T. ) ;
#91944 = EDGE_CURVE ( 'NONE', #101605, #12823, #64159, .T. ) ;
#91945 = CARTESIAN_POINT ( 'NONE',  ( -8.350000000000012079, 2.500000000000000000, 1.472243186433545459 ) ) ;
#91946 = DIRECTION ( 'NONE',  ( 0.000000000000000000, 0.000000000000000000, -1.000000000000000000 ) ) ;
#91947 = CARTESIAN_POINT ( 'NONE',  ( -8.350000000000008527, 12.50000000000000000, 5.802370205355744659 ) ) ;
#91948 = DIRECTION ( 'NONE',  ( 0.000000000000000000, 0.000000000000000000, 1.000000000000000000 ) ) ;
#91949 = DIRECTION ( 'NONE',  ( 0.000000000000000000, 0.000000000000000000, -1.000000000000000000 ) ) ;
#91950 = CARTESIAN_POINT ( 'NONE',  ( 185.4583333333333428, 4.445597072760175905, 7.699999999999896261 ) ) ;
#91951 = CARTESIAN_POINT ( 'NONE',  ( -7.300000000000016698, 12.50000000000000000, -4.676537180435978769 ) ) ;
#91952 = DIRECTION ( 'NONE',  ( 0.000000000000000000, 0.000000000000000000, 1.000000000000000000 ) ) ;
#91953 = EDGE_CURVE ( 'NONE', #122362, #35123, #88031, .T. ) ;
#91954 = CARTESIAN_POINT ( 'NONE',  ( -4.600000000000024514, 2.500000000000000000, 5.022947341949748790 ) ) ;
#91955 = ORIENTED_EDGE ( 'NONE', *, *, #68212, .T. ) ;
#91956 = ORIENTED_EDGE ( 'NONE', *, *, #28841, .T. ) ;
#91957 = EDGE_LOOP ( 'NONE', ( #20230, #69470, #118356, #8082 ) ) ;
#91958 = VERTEX_POINT ( 'NONE', #74628 ) ;
#91959 = ORIENTED_EDGE ( 'NONE', *, *, #73435, .F. ) ;
#91960 = ORIENTED_EDGE ( 'NONE', *, *, #9375, .T. ) ;
#91961 = CARTESIAN_POINT ( 'NONE',  ( -4.150000000000025224, 12.50000000000000000, 5.802370205355744659 ) ) ;
#91962 = AXIS2_PLACEMENT_3D ( 'NONE', #27396, #67309, #35955 ) ;
#91963 = VERTEX_POINT ( 'NONE', #34072 ) ;
#91964 = ORIENTED_EDGE ( 'NONE', *, *, #50410, .F. ) ;
#91967 = CIRCLE ( 'NONE', #71041, 0.06509327318403745899 ) ;
#91966 = FACE_OUTER_BOUND ( 'NONE', #104985, .T. ) ;
#91965 = AXIS2_PLACEMENT_3D ( 'NONE', #107660, #17974, #116168 ) ;
#91968 = DIRECTION ( 'NONE',  ( 0.000000000000000000, 0.000000000000000000, -1.000000000000000000 ) ) ;
#91969 = CARTESIAN_POINT ( 'NONE',  ( 179.5000000000000000, 0.000000000000000000, 0.000000000000000000 ) ) ;
#91970 = PLANE ( 'NONE',  #42590 ) ;
#91971 = ORIENTED_EDGE ( 'NONE', *, *, #53531, .T. ) ;
#91972 = CARTESIAN_POINT ( 'NONE',  ( 12.49999999999990585, 12.50000000000000000, -5.022947341949754119 ) ) ;
#91973 = AXIS2_PLACEMENT_3D ( 'NONE', #7331, #106817, #26354 ) ;
#91974 = ORIENTED_EDGE ( 'NONE', *, *, #125179, .T. ) ;
#91975 = ADVANCED_FACE ( 'NONE', ( #125018 ), #6455, .T. ) ;
#91976 = EDGE_LOOP ( 'NONE', ( #128949, #54940 ) ) ;
#91977 = PLANE ( 'NONE',  #86515 ) ;
#91978 = CARTESIAN_POINT ( 'NONE',  ( -2.100000000000033840, 2.500000000000000000, 3.637306695894644726 ) ) ;
#91979 = EDGE_CURVE ( 'NONE', #40490, #124385, #25350, .T. ) ;
#91980 = VERTEX_POINT ( 'NONE', #15033 ) ;
#91982 = EDGE_CURVE ( 'NONE', #24753, #43343, #67096, .T. ) ;
#91981 = EDGE_LOOP ( 'NONE', ( #74142, #48596, #11694, #36247 ) ) ;
#91983 = LINE ( 'NONE', #72359, #23403 ) ;
#91984 = DIRECTION ( 'NONE',  ( 0.000000000000000000, 0.000000000000000000, -1.000000000000000000 ) ) ;
#91985 = DIRECTION ( 'NONE',  ( 0.000000000000000000, 0.000000000000000000, 1.000000000000000000 ) ) ;
#91986 = FACE_OUTER_BOUND ( 'NONE', #103944, .T. ) ;
#91987 = ADVANCED_FACE ( 'NONE', ( #98774 ), #107309, .T. ) ;
#91988 = EDGE_CURVE ( 'NONE', #27272, #75731, #106827, .T. ) ;
#91989 = DIRECTION ( 'NONE',  ( -4.274815082592931898E-19, -0.9999939076577903929, -0.003490651415223739937 ) ) ;
#91990 = ADVANCED_FACE ( 'NONE', ( #47120 ), #6495, .T. ) ;
#91991 = EDGE_CURVE ( 'NONE', #45160, #47559, #81784, .T. ) ;
#91992 = ORIENTED_EDGE ( 'NONE', *, *, #98565, .T. ) ;
#91993 = CARTESIAN_POINT ( 'NONE',  ( 13.91976764350727080, -2.500000000000000888, 6.779443706236988554 ) ) ;
#91994 = VECTOR ( 'NONE', #108569, 1000.000000000000000 ) ;
#91995 = AXIS2_PLACEMENT_3D ( 'NONE', #99045, #38196, #97107 ) ;
#91996 = ORIENTED_EDGE ( 'NONE', *, *, #90200, .T. ) ;
#91997 = CARTESIAN_POINT ( 'NONE',  ( -6.450000000000019718, 2.500000000000000000, -6.148780366869526226 ) ) ;
#91998 = EDGE_CURVE ( 'NONE', #53510, #108831, #10674, .T. ) ;
#91999 = CARTESIAN_POINT ( 'NONE',  ( 65.38812792108305416, -3.824344329442378676, 5.305601465418086526 ) ) ;
#92000 = DIRECTION ( 'NONE',  ( -4.274815082592931898E-19, -0.9999939076577903929, -0.003490651415223739937 ) ) ;
#92001 = DIRECTION ( 'NONE',  ( 0.000000000000000000, 1.000000000000000000, 0.000000000000000000 ) ) ;
#92002 = CARTESIAN_POINT ( 'NONE',  ( 6.649999999999927525, 2.500000000000000000, 2.165063509461097713 ) ) ;
#92003 = ORIENTED_EDGE ( 'NONE', *, *, #27937, .F. ) ;
#92005 = EDGE_CURVE ( 'NONE', #102522, #93617, #44150, .T. ) ;
#92004 = CIRCLE ( 'NONE', #35575, 0.1000000000000002554 ) ;
#92006 = DIRECTION ( 'NONE',  ( -0.000000000000000000, 1.000000000000000000, -0.000000000000000000 ) ) ;
#92007 = DIRECTION ( 'NONE',  ( 0.000000000000000000, -0.000000000000000000, 1.000000000000000000 ) ) ;
#92008 = EDGE_LOOP ( 'NONE', ( #92481, #38127, #92603, #13898 ) ) ;
#92009 = VERTEX_POINT ( 'NONE', #56273 ) ;
#92010 = ORIENTED_EDGE ( 'NONE', *, *, #99043, .T. ) ;
#92011 = DIRECTION ( 'NONE',  ( -0.000000000000000000, -1.000000000000000000, -0.000000000000000000 ) ) ;
#92012 = DIRECTION ( 'NONE',  ( -4.274815082592931898E-19, -0.9999939076577903929, -0.003490651415223739937 ) ) ;
#92013 = DIRECTION ( 'NONE',  ( -0.000000000000000000, -1.000000000000000000, -0.000000000000000000 ) ) ;
#92014 = AXIS2_PLACEMENT_3D ( 'NONE', #23664, #4009, #43957 ) ;
#92015 = DIRECTION ( 'NONE',  ( 0.000000000000000000, 1.000000000000000000, 0.000000000000000000 ) ) ;
#92016 = CARTESIAN_POINT ( 'NONE',  ( -10.85000000000000142, 2.500000000000000000, 2.265063509461097357 ) ) ;
#92017 = VECTOR ( 'NONE', #108130, 1000.000000000000000 ) ;
#92018 = CIRCLE ( 'NONE', #85658, 0.1000000000000000472 ) ;
#92019 = DIRECTION ( 'NONE',  ( 0.000000000000000000, 0.000000000000000000, 1.000000000000000000 ) ) ;
#92020 = DIRECTION ( 'NONE',  ( -4.274815082592931898E-19, -0.9999939076577903929, -0.003490651415223739937 ) ) ;
#92021 = DIRECTION ( 'NONE',  ( -0.000000000000000000, -1.000000000000000000, -0.000000000000000000 ) ) ;
#92022 = VECTOR ( 'NONE', #90937, 1000.000000000000000 ) ;
#92023 = EDGE_LOOP ( 'NONE', ( #23765, #13819, #41983, #7206 ) ) ;
#92024 = CIRCLE ( 'NONE', #18857, 0.1000000000000002554 ) ;
#92025 = LINE ( 'NONE', #120842, #83951 ) ;
#92026 = PLANE ( 'NONE',  #5679 ) ;
#92027 = DIRECTION ( 'NONE',  ( -0.000000000000000000, 1.000000000000000000, -0.000000000000000000 ) ) ;
#92028 = DIRECTION ( 'NONE',  ( 0.000000000000000000, 1.000000000000000000, 0.000000000000000000 ) ) ;
#92029 = EDGE_LOOP ( 'NONE', ( #69637, #56916 ) ) ;
#92030 = FACE_OUTER_BOUND ( 'NONE', #106848, .T. ) ;
#92031 = ADVANCED_FACE ( 'NONE', ( #77844 ), #127771, .T. ) ;
#92032 = CARTESIAN_POINT ( 'NONE',  ( 13.09999999999990195, 12.50000000000000000, -3.918623584224389056 ) ) ;
#92034 = ORIENTED_EDGE ( 'NONE', *, *, #42138, .T. ) ;
#92033 = DIRECTION ( 'NONE',  ( -0.000000000000000000, 1.000000000000000000, -0.000000000000000000 ) ) ;
#92035 = ORIENTED_EDGE ( 'NONE', *, *, #94195, .T. ) ;
#92036 = CARTESIAN_POINT ( 'NONE',  ( 3.749999999999938716, 12.50000000000000000, 7.188010851410848723 ) ) ;
#92037 = EDGE_CURVE ( 'NONE', #93758, #10983, #7164, .T. ) ;
#92038 = ORIENTED_EDGE ( 'NONE', *, *, #16740, .F. ) ;
#92039 = VERTEX_POINT ( 'NONE', #48396 ) ;
#92040 = DIRECTION ( 'NONE',  ( 0.000000000000000000, -0.000000000000000000, 1.000000000000000000 ) ) ;
#92041 = CONICAL_SURFACE ( 'NONE', #106699, 0.1000000000000002554, 0.003490658503988666988 ) ;
#92042 = AXIS2_PLACEMENT_3D ( 'NONE', #41776, #93433, #92800 ) ;
#92043 = CARTESIAN_POINT ( 'NONE',  ( 20.69433222468020972, 2.585316282069821892, -4.139109617385188677 ) ) ;
#92044 = DIRECTION ( 'NONE',  ( 0.000000000000000000, 0.000000000000000000, 1.000000000000000000 ) ) ;
#92045 = DIRECTION ( 'NONE',  ( -0.000000000000000000, -1.000000000000000000, -0.000000000000000000 ) ) ;
#92046 = VERTEX_POINT ( 'NONE', #28113 ) ;
#92047 = AXIS2_PLACEMENT_3D ( 'NONE', #44762, #84671, #93218 ) ;
#92048 = CARTESIAN_POINT ( 'NONE',  ( -3.350000000000032507, 12.50000000000000000, -6.495190528383302464 ) ) ;
#92049 = ORIENTED_EDGE ( 'NONE', *, *, #117782, .T. ) ;
#92050 = PLANE ( 'NONE',  #61066 ) ;
#92051 = CARTESIAN_POINT ( 'NONE',  ( 12.69999999999989981, 2.500000000000000000, -0.2464101615137783419 ) ) ;
#92052 = ORIENTED_EDGE ( 'NONE', *, *, #43197, .F. ) ;
#92053 = VERTEX_POINT ( 'NONE', #78525 ) ;
#92054 = ORIENTED_EDGE ( 'NONE', *, *, #95178, .T. ) ;
#92055 = ORIENTED_EDGE ( 'NONE', *, *, #60683, .T. ) ;
#92056 = DIRECTION ( 'NONE',  ( 0.000000000000000000, 0.000000000000000000, 1.000000000000000000 ) ) ;
#92057 = CARTESIAN_POINT ( 'NONE',  ( 16.56576425165006583, 1.499999999999999334, 6.084390597445812787 ) ) ;
#92058 = CARTESIAN_POINT ( 'NONE',  ( 4.399999999999940847, 12.50000000000000000, -3.983716857408426293 ) ) ;
#92059 = FACE_BOUND ( 'NONE', #56552, .T. ) ;
#92060 = VERTEX_POINT ( 'NONE', #27446 ) ;
#92061 = CARTESIAN_POINT ( 'NONE',  ( 185.3229166673494888, -4.445597072760122614, 7.699999999999998401 ) ) ;
#92062 = FACE_OUTER_BOUND ( 'NONE', #45313, .T. ) ;
#92063 = CARTESIAN_POINT ( 'NONE',  ( 187.5000000000000000, 9.429780353434619030E-16, -7.700000000000000178 ) ) ;
#92064 = EDGE_CURVE ( 'NONE', #105417, #87541, #117275, .T. ) ;
#92065 = DIRECTION ( 'NONE',  ( -0.000000000000000000, -1.000000000000000000, -0.000000000000000000 ) ) ;
#92066 = CARTESIAN_POINT ( 'NONE',  ( -9.550000000000006040, 2.500000000000000000, -2.165063509461101710 ) ) ;
#92067 = FACE_OUTER_BOUND ( 'NONE', #42150, .T. ) ;
#92068 = VECTOR ( 'NONE', #7319, 1000.000000000000000 ) ;
#92069 = EDGE_CURVE ( 'NONE', #30053, #94650, #46449, .T. ) ;
#92070 = AXIS2_PLACEMENT_3D ( 'NONE', #94722, #63982, #103909 ) ;
#92071 = FACE_OUTER_BOUND ( 'NONE', #118520, .T. ) ;
#92072 = ORIENTED_EDGE ( 'NONE', *, *, #100378, .T. ) ;
#92073 = VERTEX_POINT ( 'NONE', #107960 ) ;
#92074 = ORIENTED_EDGE ( 'NONE', *, *, #55143, .T. ) ;
#92075 = ORIENTED_EDGE ( 'NONE', *, *, #11089, .F. ) ;
#92076 = EDGE_LOOP ( 'NONE', ( #52284, #104723, #21483, #102281 ) ) ;
#92077 = FACE_OUTER_BOUND ( 'NONE', #29854, .T. ) ;
#92078 = ADVANCED_FACE ( 'NONE', ( #86374 ), #36663, .T. ) ;
#92079 = FACE_OUTER_BOUND ( 'NONE', #108477, .T. ) ;
#92080 = VERTEX_POINT ( 'NONE', #126960 ) ;
#92081 = FACE_BOUND ( 'NONE', #118103, .T. ) ;
#92082 = EDGE_CURVE ( 'NONE', #32290, #126580, #66734, .T. ) ;
#92083 = AXIS2_PLACEMENT_3D ( 'NONE', #3672, #24609, #33773 ) ;
#92084 = DIRECTION ( 'NONE',  ( 1.000000000000000000, 0.000000000000000000, 0.000000000000000000 ) ) ;
#92085 = EDGE_CURVE ( 'NONE', #19127, #82397, #104761, .T. ) ;
#92086 = ORIENTED_EDGE ( 'NONE', *, *, #22881, .F. ) ;
#92087 = CARTESIAN_POINT ( 'NONE',  ( -3.750000000000031086, 2.500000000000000000, -5.802370205355749988 ) ) ;
#92088 = DIRECTION ( 'NONE',  ( -0.000000000000000000, 1.000000000000000000, -0.000000000000000000 ) ) ;
#92089 = EDGE_CURVE ( 'NONE', #126865, #21052, #98130, .T. ) ;
#92090 = DIRECTION ( 'NONE',  ( -0.000000000000000000, 1.000000000000000000, -0.000000000000000000 ) ) ;
#92091 = VERTEX_POINT ( 'NONE', #88295 ) ;
#92092 = CARTESIAN_POINT ( 'NONE',  ( -4.600000000000028066, 2.500000000000000000, -3.737306695894649700 ) ) ;
#92093 = VECTOR ( 'NONE', #34751, 1000.000000000000000 ) ;
#92094 = ORIENTED_EDGE ( 'NONE', *, *, #62405, .F. ) ;
#92095 = AXIS2_PLACEMENT_3D ( 'NONE', #121673, #22862, #89800 ) ;
#92096 = PRODUCT_DEFINITION_SHAPE ( 'NONE', 'NONE',  #14818 ) ;
#92097 = EDGE_LOOP ( 'NONE', ( #120875, #43039, #110344, #68160 ) ) ;
#92098 = EDGE_LOOP ( 'NONE', ( #67617, #74875 ) ) ;
#92099 = DIRECTION ( 'NONE',  ( 0.000000000000000000, 0.000000000000000000, -1.000000000000000000 ) ) ;
#92100 = CARTESIAN_POINT ( 'NONE',  ( 11.24999999999990585, 2.500000000000000000, -5.802370205355749988 ) ) ;
#92101 = ORIENTED_EDGE ( 'NONE', *, *, #105703, .T. ) ;
#92102 = LINE ( 'NONE', #112407, #62194 ) ;
#92103 = AXIS2_PLACEMENT_3D ( 'NONE', #107189, #105917, #35885 ) ;
#92104 = DIRECTION ( 'NONE',  ( -0.000000000000000000, -1.000000000000000000, -0.000000000000000000 ) ) ;
#92105 = CARTESIAN_POINT ( 'NONE',  ( -1.650000000000035216, 12.50000000000000000, -1.407149913249512663 ) ) ;
#92106 = CARTESIAN_POINT ( 'NONE',  ( 0.1999999999999636513, 2.500000000000000000, -0.4464101615137760493 ) ) ;
#92107 = CIRCLE ( 'NONE', #39906, 0.09999999999999982514 ) ;
#92108 = CARTESIAN_POINT ( 'NONE',  ( 10.64999999999991331, 12.50000000000000000, -2.511473670974877948 ) ) ;
#92109 = VERTEX_POINT ( 'NONE', #28767 ) ;
#92110 = CARTESIAN_POINT ( 'NONE',  ( 2.499999999999947153, 2.500000000000000000, -3.737306695894649700 ) ) ;
#92111 = ORIENTED_EDGE ( 'NONE', *, *, #9037, .T. ) ;
#92112 = DIRECTION ( 'NONE',  ( 0.000000000000000000, 0.000000000000000000, 1.000000000000000000 ) ) ;
#92113 = ORIENTED_EDGE ( 'NONE', *, *, #26378, .T. ) ;
#92114 = FACE_OUTER_BOUND ( 'NONE', #32067, .T. ) ;
#92115 = ORIENTED_EDGE ( 'NONE', *, *, #34968, .F. ) ;
#92116 = DIRECTION ( 'NONE',  ( -0.000000000000000000, -1.000000000000000000, -0.000000000000000000 ) ) ;
#92117 = CARTESIAN_POINT ( 'NONE',  ( -10.84999999999999964, 12.50000000000000000, 2.792790559304612064 ) ) ;
#92118 = CARTESIAN_POINT ( 'NONE',  ( 12.09999999999990550, 2.500000000000000000, -4.330127018922201643 ) ) ;
#92119 = CARTESIAN_POINT ( 'NONE',  ( 179.5000000000000000, -0.6250000000000003331, 6.000000000000000000 ) ) ;
#92120 = FACE_OUTER_BOUND ( 'NONE', #70627, .T. ) ;
#92121 = VERTEX_POINT ( 'NONE', #37930 ) ;
#92122 = ORIENTED_EDGE ( 'NONE', *, *, #26645, .F. ) ;
#92123 = FACE_OUTER_BOUND ( 'NONE', #71728, .T. ) ;
#92124 = DIRECTION ( 'NONE',  ( 0.000000000000000000, -0.000000000000000000, -1.000000000000000000 ) ) ;
#92127 = EDGE_CURVE ( 'NONE', #57128, #121644, #121491, .T. ) ;
#92126 = DIRECTION ( 'NONE',  ( 0.000000000000000000, -0.000000000000000000, 1.000000000000000000 ) ) ;
#92125 = AXIS2_PLACEMENT_3D ( 'NONE', #88440, #83158, #14382 ) ;
#92129 = ORIENTED_EDGE ( 'NONE', *, *, #113289, .T. ) ;
#92128 = VERTEX_POINT ( 'NONE', #49058 ) ;
#92130 = ORIENTED_EDGE ( 'NONE', *, *, #101497, .T. ) ;
#92131 = CIRCLE ( 'NONE', #23176, 0.1000000000000002554 ) ;
#92132 = EDGE_CURVE ( 'NONE', #5978, #37903, #88968, .T. ) ;
#92133 = AXIS2_PLACEMENT_3D ( 'NONE', #17425, #37099, #116918 ) ;
#92134 = DIRECTION ( 'NONE',  ( 0.000000000000000000, 1.000000000000000000, 0.000000000000000000 ) ) ;
#92135 = ADVANCED_FACE ( 'NONE', ( #31993 ), #1224, .T. ) ;
#92136 = ADVANCED_FACE ( 'NONE', ( #59535 ), #219, .T. ) ;
#92137 = VERTEX_POINT ( 'NONE', #19580 ) ;
#92138 = CARTESIAN_POINT ( 'NONE',  ( -12.29999999999999361, 2.500000000000000000, 3.983716857408420076 ) ) ;
#92139 = LINE ( 'NONE', #90859, #95848 ) ;
#92140 = AXIS2_PLACEMENT_3D ( 'NONE', #75448, #127151, #35550 ) ;
#92141 = CARTESIAN_POINT ( 'NONE',  ( -7.900000000000014566, 2.500000000000000000, -4.330127018922201643 ) ) ;
#92142 = ORIENTED_EDGE ( 'NONE', *, *, #129092, .T. ) ;
#92143 = DIRECTION ( 'NONE',  ( 0.000000000000000000, 0.000000000000000000, -1.000000000000000000 ) ) ;
#92145 = EDGE_CURVE ( 'NONE', #108759, #129486, #18994, .T. ) ;
#92144 = DIRECTION ( 'NONE',  ( 0.000000000000000000, 0.000000000000000000, -1.000000000000000000 ) ) ;
#92146 = CARTESIAN_POINT ( 'NONE',  ( 11.24999999999990763, 2.500000000000000000, 1.472243186433545459 ) ) ;
#92147 = DIRECTION ( 'NONE',  ( 0.000000000000000000, -0.9999939076577903929, 0.003490651415223739937 ) ) ;
#92148 = AXIS2_PLACEMENT_3D ( 'NONE', #72984, #100502, #72355 ) ;
#92149 = CARTESIAN_POINT ( 'NONE',  ( -13.74999999999998757, 12.50000000000000000, -2.792790559304614284 ) ) ;
#92150 = ORIENTED_EDGE ( 'NONE', *, *, #124593, .F. ) ;
#92151 = ADVANCED_FACE ( 'NONE', ( #9758 ), #56644, .T. ) ;
#92152 = CARTESIAN_POINT ( 'NONE',  ( -6.850000000000017408, 12.50000000000000000, -6.148780366869526226 ) ) ;
#92153 = EDGE_CURVE ( 'NONE', #94042, #86969, #2494, .T. ) ;
#92154 = CARTESIAN_POINT ( 'NONE',  ( 21.23528140090950700, -2.699413673072311504, 2.293764360948885805 ) ) ;
#92155 = ORIENTED_EDGE ( 'NONE', *, *, #91846, .T. ) ;
#92156 = VERTEX_POINT ( 'NONE', #71247 ) ;
#92157 = CARTESIAN_POINT ( 'NONE',  ( 186.7968750003414300, 8.734944146203032389, 5.348610694689227483E-16 ) ) ;
#92158 = DIRECTION ( 'NONE',  ( 0.000000000000000000, 0.000000000000000000, -1.000000000000000000 ) ) ;
#92159 = DIRECTION ( 'NONE',  ( 0.000000000000000000, 0.000000000000000000, -1.000000000000000000 ) ) ;
#92160 = EDGE_CURVE ( 'NONE', #41592, #71750, #2277, .T. ) ;
#92161 = CARTESIAN_POINT ( 'NONE',  ( -2.300000000000032685, 2.500000000000000000, -4.576537180435978236 ) ) ;
#92162 = DIRECTION ( 'NONE',  ( -0.000000000000000000, 1.000000000000000000, -0.000000000000000000 ) ) ;
#92163 = AXIS2_PLACEMENT_3D ( 'NONE', #34010, #24193, #93577 ) ;
#92164 = DIRECTION ( 'NONE',  ( 0.000000000000000000, 0.000000000000000000, 1.000000000000000000 ) ) ;
#92165 = CARTESIAN_POINT ( 'NONE',  ( -6.850000000000013856, 2.500000000000000000, 1.918653347947321564 ) ) ;
#92166 = DIRECTION ( 'NONE',  ( 0.000000000000000000, -0.000000000000000000, 1.000000000000000000 ) ) ;
#92167 = LINE ( 'NONE', #80435, #50153 ) ;
#92168 = AXIS2_PLACEMENT_3D ( 'NONE', #121001, #40533, #110533 ) ;
#92169 = ORIENTED_EDGE ( 'NONE', *, *, #28576, .F. ) ;
#92171 = VERTEX_POINT ( 'NONE', #111833 ) ;
#92170 = AXIS2_PLACEMENT_3D ( 'NONE', #4239, #4884, #81536 ) ;
#92172 = ORIENTED_EDGE ( 'NONE', *, *, #124899, .F. ) ;
#92173 = ORIENTED_EDGE ( 'NONE', *, *, #24132, .F. ) ;
#92174 = DIRECTION ( 'NONE',  ( 0.000000000000000000, 1.000000000000000000, 0.000000000000000000 ) ) ;
#92175 = DIRECTION ( 'NONE',  ( -0.000000000000000000, -1.000000000000000000, -0.000000000000000000 ) ) ;
#92176 = CONICAL_SURFACE ( 'NONE', #85908, 0.1000000000000002554, 0.003490658503988666988 ) ;
#92177 = CIRCLE ( 'NONE', #54519, 0.06509327318403745899 ) ;
#92178 = VERTEX_POINT ( 'NONE', #22181 ) ;
#92179 = PLANE ( 'NONE',  #125953 ) ;
#92180 = CARTESIAN_POINT ( 'NONE',  ( 11.89999999999990443, 12.50000000000000000, 0.3464101615137736845 ) ) ;
#92182 = VERTEX_POINT ( 'NONE', #60167 ) ;
#92181 = DIRECTION ( 'NONE',  ( -0.000000000000000000, 1.000000000000000000, -0.000000000000000000 ) ) ;
#92183 = DIRECTION ( 'NONE',  ( -4.274815082592931898E-19, -0.9999939076577903929, -0.003490651415223739937 ) ) ;
#92184 = DIRECTION ( 'NONE',  ( 0.000000000000000000, 0.000000000000000000, 1.000000000000000000 ) ) ;
#92185 = AXIS2_PLACEMENT_3D ( 'NONE', #126823, #34600, #64036 ) ;
#92186 = ORIENTED_EDGE ( 'NONE', *, *, #54244, .F. ) ;
#92187 = VECTOR ( 'NONE', #57460, 1000.000000000000000 ) ;
#92188 = EDGE_CURVE ( 'NONE', #121009, #29184, #35743, .T. ) ;
#92189 = ORIENTED_EDGE ( 'NONE', *, *, #30089, .F. ) ;
#92190 = ORIENTED_EDGE ( 'NONE', *, *, #76923, .F. ) ;
#92191 = VERTEX_POINT ( 'NONE', #20227 ) ;
#92192 = CARTESIAN_POINT ( 'NONE',  ( 10.19999999999991047, 2.500000000000000000, 4.576537180435972019 ) ) ;
#92193 = AXIS2_PLACEMENT_3D ( 'NONE', #3685, #51511, #73075 ) ;
#92194 = DIRECTION ( 'NONE',  ( 0.000000000000000000, -0.9999939076577903929, 0.003490651415223739937 ) ) ;
#92195 = DIRECTION ( 'NONE',  ( -0.000000000000000000, -1.000000000000000000, -0.000000000000000000 ) ) ;
#92196 = CARTESIAN_POINT ( 'NONE',  ( 3.549999999999941203, 12.50000000000000000, 6.213873640053559022 ) ) ;
#92197 = ORIENTED_EDGE ( 'NONE', *, *, #97909, .F. ) ;
#92198 = CIRCLE ( 'NONE', #46235, 0.1000000000000002554 ) ;
#92199 = AXIS2_PLACEMENT_3D ( 'NONE', #22792, #73163, #24706 ) ;
#92200 = CARTESIAN_POINT ( 'NONE',  ( -11.44999999999999751, 12.50000000000000000, 1.883746621131358934 ) ) ;
#92201 = VERTEX_POINT ( 'NONE', #31349 ) ;
#92202 = CARTESIAN_POINT ( 'NONE',  ( 10.59999999999990905, 2.500000000000000000, -3.883716857408426648 ) ) ;
#92203 = DIRECTION ( 'NONE',  ( 0.000000000000000000, 0.000000000000000000, -1.000000000000000000 ) ) ;
#92204 = CARTESIAN_POINT ( 'NONE',  ( 4.149999999999941735, 2.500000000000000000, -5.702370205355749455 ) ) ;
#92205 = CARTESIAN_POINT ( 'NONE',  ( -4.800000000000024691, 2.500000000000000000, 0.3464101615137735735 ) ) ;
#92206 = ORIENTED_EDGE ( 'NONE', *, *, #79763, .T. ) ;
#92207 = VERTEX_POINT ( 'NONE', #91543 ) ;
#92208 = ORIENTED_EDGE ( 'NONE', *, *, #64941, .F. ) ;
#92209 = CARTESIAN_POINT ( 'NONE',  ( 8.349999999999919709, 12.50000000000000000, -2.230156782645139391 ) ) ;
#92210 = LINE ( 'NONE', #122980, #8011 ) ;
#92211 = CARTESIAN_POINT ( 'NONE',  ( 2.699999999999946443, 2.500000000000000000, 0.4464101615137735513 ) ) ;
#92212 = FACE_BOUND ( 'NONE', #108192, .T. ) ;
#92213 = DIRECTION ( 'NONE',  ( -0.000000000000000000, -1.000000000000000000, -0.000000000000000000 ) ) ;
#92214 = DIRECTION ( 'NONE',  ( -0.000000000000000000, 1.000000000000000000, -0.000000000000000000 ) ) ;
#92215 = DIRECTION ( 'NONE',  ( 0.000000000000000000, 1.000000000000000000, 0.000000000000000000 ) ) ;
#92216 = CIRCLE ( 'NONE', #75490, 0.09999999999999999167 ) ;
#92217 = CIRCLE ( 'NONE', #35802, 0.06509327318403745899 ) ;
#92219 = CONICAL_SURFACE ( 'NONE', #4464, 0.1000000000000000472, 0.003490658503988666988 ) ;
#92218 = DIRECTION ( 'NONE',  ( 0.000000000000000000, -0.9999939076577903929, 0.003490651415223739937 ) ) ;
#92220 = DIRECTION ( 'NONE',  ( -0.000000000000000000, 1.000000000000000000, -0.000000000000000000 ) ) ;
#92221 = FACE_OUTER_BOUND ( 'NONE', #76713, .T. ) ;
#92222 = VERTEX_POINT ( 'NONE', #20871 ) ;
#92223 = CARTESIAN_POINT ( 'NONE',  ( 11.24999999999994316, 2.500000000000000000, -6.595190528383302109 ) ) ;
#92224 = EDGE_CURVE ( 'NONE', #2627, #106863, #52456, .T. ) ;
#92225 = CIRCLE ( 'NONE', #56705, 0.1000000000000002554 ) ;
#92226 = DIRECTION ( 'NONE',  ( 0.000000000000000000, 1.000000000000000000, 0.000000000000000000 ) ) ;
#92227 = AXIS2_PLACEMENT_3D ( 'NONE', #15481, #5656, #16114 ) ;
#92228 = EDGE_LOOP ( 'NONE', ( #58720, #98987 ) ) ;
#92229 = ORIENTED_EDGE ( 'NONE', *, *, #97919, .T. ) ;
#92230 = AXIS2_PLACEMENT_3D ( 'NONE', #84733, #65731, #25161 ) ;
#92231 = DIRECTION ( 'NONE',  ( 0.000000000000000000, 1.000000000000000000, 0.000000000000000000 ) ) ;
#92232 = EDGE_CURVE ( 'NONE', #14173, #24264, #102008, .T. ) ;
#92233 = CARTESIAN_POINT ( 'NONE',  ( -11.24999999999999822, 2.500000000000000000, 5.902370205355745192 ) ) ;
#92234 = FACE_BOUND ( 'NONE', #75893, .T. ) ;
#92235 = EDGE_CURVE ( 'NONE', #10651, #41348, #82383, .T. ) ;
#92236 = CARTESIAN_POINT ( 'NONE',  ( 10.39999999999991154, 2.500000000000000000, -5.022947341949754119 ) ) ;
#92237 = ADVANCED_FACE ( 'NONE', ( #52266 ), #50330, .T. ) ;
#92238 = ADVANCED_FACE ( 'NONE', ( #30713 ), #4492, .T. ) ;
#92239 = ORIENTED_EDGE ( 'NONE', *, *, #118613, .F. ) ;
#92240 = LINE ( 'NONE', #79849, #36180 ) ;
#92241 = ADVANCED_FACE ( 'NONE', ( #11030 ), #50990, .T. ) ;
#92242 = EDGE_CURVE ( 'NONE', #46755, #4130, #2454, .T. ) ;
#92243 = CARTESIAN_POINT ( 'NONE',  ( -13.74999999999998934, 12.50000000000000000, 2.922977105672690534 ) ) ;
#92244 = EDGE_CURVE ( 'NONE', #117178, #1307, #41818, .T. ) ;
#92245 = ORIENTED_EDGE ( 'NONE', *, *, #48531, .T. ) ;
#92246 = CARTESIAN_POINT ( 'NONE',  ( 12.29999999999990123, 2.500000000000000000, 0.3464101615137735735 ) ) ;
#92247 = FACE_OUTER_BOUND ( 'NONE', #100425, .T. ) ;
#92248 = ORIENTED_EDGE ( 'NONE', *, *, #90622, .T. ) ;
#92249 = CARTESIAN_POINT ( 'NONE',  ( -3.150000000000033218, 2.500000000000000000, -6.741600689897078169 ) ) ;
#92251 = ADVANCED_FACE ( 'NONE', ( #95411 ), #35837, .T. ) ;
#92250 = PLANE ( 'NONE',  #65648 ) ;
#92252 = CIRCLE ( 'NONE', #71412, 0.06509327318403741736 ) ;
#92253 = AXIS2_PLACEMENT_3D ( 'NONE', #18591, #8748, #8117 ) ;
#92254 = ORIENTED_EDGE ( 'NONE', *, *, #104752, .F. ) ;
#92255 = DIRECTION ( 'NONE',  ( 0.000000000000000000, 0.000000000000000000, -1.000000000000000000 ) ) ;
#92256 = LINE ( 'NONE', #42548, #99980 ) ;
#92257 = DIRECTION ( 'NONE',  ( 0.000000000000000000, 0.000000000000000000, -1.000000000000000000 ) ) ;
#92258 = ORIENTED_EDGE ( 'NONE', *, *, #35927, .F. ) ;
#92259 = ORIENTED_EDGE ( 'NONE', *, *, #6252, .T. ) ;
#92260 = FACE_OUTER_BOUND ( 'NONE', #1232, .T. ) ;
#92261 = CIRCLE ( 'NONE', #81884, 0.09999999999999982514 ) ;
#92262 = EDGE_LOOP ( 'NONE', ( #113274, #60073 ) ) ;
#92263 = DIRECTION ( 'NONE',  ( 0.000000000000000000, 0.000000000000000000, 1.000000000000000000 ) ) ;
#92264 = AXIS2_PLACEMENT_3D ( 'NONE', #124369, #126946, #34718 ) ;
#92265 = DIRECTION ( 'NONE',  ( -0.000000000000000000, -1.000000000000000000, -0.000000000000000000 ) ) ;
#92266 = PLANE ( 'NONE',  #46678 ) ;
#92267 = ORIENTED_EDGE ( 'NONE', *, *, #129566, .F. ) ;
#92268 = DIRECTION ( 'NONE',  ( -4.274815082592931898E-19, -0.9999939076577903929, -0.003490651415223739937 ) ) ;
#92269 = DIRECTION ( 'NONE',  ( 0.000000000000000000, 0.000000000000000000, -1.000000000000000000 ) ) ;
#92270 = DIRECTION ( 'NONE',  ( 0.000000000000000000, 0.000000000000000000, 1.000000000000000000 ) ) ;
#92271 = DIRECTION ( 'NONE',  ( 0.000000000000000000, 0.000000000000000000, 1.000000000000000000 ) ) ;
#92272 = DIRECTION ( 'NONE',  ( 0.000000000000000000, 0.000000000000000000, -1.000000000000000000 ) ) ;
#92273 = DIRECTION ( 'NONE',  ( 0.000000000000000000, 0.000000000000000000, 1.000000000000000000 ) ) ;
#92274 = VECTOR ( 'NONE', #91401, 1000.000000000000000 ) ;
#92275 = EDGE_LOOP ( 'NONE', ( #15599, #85410 ) ) ;
#92276 = PRODUCT_DEFINITION_FORMATION_WITH_SPECIFIED_SOURCE ( 'ANY', '', #52397, .NOT_KNOWN. ) ;
#92277 = AXIS2_PLACEMENT_3D ( 'NONE', #112198, #287, #50695 ) ;
#92278 = EDGE_LOOP ( 'NONE', ( #45728, #101736, #56313, #70970 ) ) ;
#92279 = DIRECTION ( 'NONE',  ( 0.000000000000000000, 0.000000000000000000, -1.000000000000000000 ) ) ;
#92280 = EDGE_LOOP ( 'NONE', ( #86962, #30100, #54931, #34294 ) ) ;
#92281 = DIRECTION ( 'NONE',  ( 0.000000000000000000, 0.000000000000000000, 1.000000000000000000 ) ) ;
#92282 = VECTOR ( 'NONE', #114887, 1000.000000000000000 ) ;
#92283 = ADVANCED_FACE ( 'NONE', ( #112480 ), #22821, .T. ) ;
#92285 = EDGE_LOOP ( 'NONE', ( #55692, #40898, #94039, #57645 ) ) ;
#92284 = ORIENTED_EDGE ( 'NONE', *, *, #4771, .T. ) ;
#92286 = EDGE_LOOP ( 'NONE', ( #86662, #17006, #126472, #111320 ) ) ;
#92287 = ADVANCED_FACE ( 'NONE', ( #52912 ), #100659, .T. ) ;
#92288 = DIRECTION ( 'NONE',  ( 0.000000000000000000, -0.9999939076577903929, 0.003490651415223739937 ) ) ;
#92289 = CONICAL_SURFACE ( 'NONE', #127898, 0.1000000000000000472, 0.003490658503988666988 ) ;
#92290 = EDGE_CURVE ( 'NONE', #79082, #76513, #27489, .T. ) ;
#92291 = DIRECTION ( 'NONE',  ( 0.000000000000000000, -0.000000000000000000, 1.000000000000000000 ) ) ;
#92292 = DIRECTION ( 'NONE',  ( -0.000000000000000000, 1.000000000000000000, -0.000000000000000000 ) ) ;
#92293 = EDGE_CURVE ( 'NONE', #54837, #98287, #37977, .T. ) ;
#92294 = CARTESIAN_POINT ( 'NONE',  ( 12.29999999999990479, 2.500000000000000000, 4.776537180435972196 ) ) ;
#92295 = AXIS2_PLACEMENT_3D ( 'NONE', #129151, #107551, #68904 ) ;
#92296 = VECTOR ( 'NONE', #3618, 1000.000000000000000 ) ;
#92297 = PLANE ( 'NONE',  #29225 ) ;
#92298 = DIRECTION ( 'NONE',  ( 0.000000000000000000, -0.000000000000000000, 1.000000000000000000 ) ) ;
#92299 = DIRECTION ( 'NONE',  ( -0.000000000000000000, -1.000000000000000000, -0.000000000000000000 ) ) ;
#92300 = FACE_OUTER_BOUND ( 'NONE', #42155, .T. ) ;
#92301 = ADVANCED_FACE ( 'NONE', ( #93481 ), #54201, .T. ) ;
#92302 = DIRECTION ( 'NONE',  ( 0.000000000000000000, -0.000000000000000000, 1.000000000000000000 ) ) ;
#92303 = ADVANCED_FACE ( 'NONE', ( #122305 ), #56729, .T. ) ;
#92305 = ORIENTED_EDGE ( 'NONE', *, *, #69098, .T. ) ;
#92304 = EDGE_CURVE ( 'NONE', #75397, #82798, #31724, .T. ) ;
#92306 = EDGE_CURVE ( 'NONE', #3120, #31226, #302, .T. ) ;
#92307 = DIRECTION ( 'NONE',  ( 0.000000000000000000, 1.000000000000000000, 0.000000000000000000 ) ) ;
#92308 = ORIENTED_EDGE ( 'NONE', *, *, #43261, .T. ) ;
#92309 = EDGE_LOOP ( 'NONE', ( #52967, #29756 ) ) ;
#92310 = DIRECTION ( 'NONE',  ( -0.000000000000000000, -1.000000000000000000, -0.000000000000000000 ) ) ;
#92311 = CARTESIAN_POINT ( 'NONE',  ( 0.3999999999999563904, 12.50000000000000000, 3.637306695894644726 ) ) ;
#92312 = DIRECTION ( 'NONE',  ( 0.000000000000000000, 1.000000000000000000, 0.000000000000000000 ) ) ;
#92313 = ADVANCED_FACE ( 'NONE', ( #23439 ), #104863, .T. ) ;
#92314 = CARTESIAN_POINT ( 'NONE',  ( 186.6666666666666856, -6.668395609140176816, -3.850000000000003642 ) ) ;
#92315 = DIRECTION ( 'NONE',  ( 0.000000000000000000, 0.000000000000000000, -1.000000000000000000 ) ) ;
#92316 = AXIS2_PLACEMENT_3D ( 'NONE', #120412, #21563, #60842 ) ;
#92317 = DIRECTION ( 'NONE',  ( 0.000000000000000000, 1.000000000000000000, 0.000000000000000000 ) ) ;
#92318 = ORIENTED_EDGE ( 'NONE', *, *, #41938, .T. ) ;
#92319 = CIRCLE ( 'NONE', #8672, 0.06509327318403745899 ) ;
#92320 = AXIS2_PLACEMENT_3D ( 'NONE', #57048, #7955, #126460 ) ;
#92321 = ORIENTED_EDGE ( 'NONE', *, *, #119744, .T. ) ;
#92322 = VECTOR ( 'NONE', #7030, 1000.000000000000000 ) ;
#92323 = ORIENTED_EDGE ( 'NONE', *, *, #9624, .T. ) ;
#92324 = CONICAL_SURFACE ( 'NONE', #2425, 0.1000000000000000472, 0.003490658503988666988 ) ;
#92325 = ORIENTED_EDGE ( 'NONE', *, *, #54390, .T. ) ;
#92326 = CIRCLE ( 'NONE', #121567, 0.09999999999999999167 ) ;
#92327 = EDGE_CURVE ( 'NONE', #98142, #48660, #92252, .T. ) ;
#92328 = ORIENTED_EDGE ( 'NONE', *, *, #4470, .T. ) ;
#92329 = FACE_OUTER_BOUND ( 'NONE', #80253, .T. ) ;
#92330 = DIRECTION ( 'NONE',  ( 0.000000000000000000, -0.9999939076577903929, 0.003490651415223739937 ) ) ;
#92331 = DIRECTION ( 'NONE',  ( 0.000000000000000000, 0.000000000000000000, 1.000000000000000000 ) ) ;
#92332 = DIRECTION ( 'NONE',  ( -0.000000000000000000, -1.000000000000000000, -0.000000000000000000 ) ) ;
#92333 = CARTESIAN_POINT ( 'NONE',  ( -9.999999999999969802, 2.500000000000000000, 4.430127018922196847 ) ) ;
#92334 = EDGE_LOOP ( 'NONE', ( #112890, #35528 ) ) ;
#92335 = DIRECTION ( 'NONE',  ( -0.000000000000000000, 1.000000000000000000, -0.000000000000000000 ) ) ;
#92336 = DIRECTION ( 'NONE',  ( 0.000000000000000000, 0.000000000000000000, -1.000000000000000000 ) ) ;
#92337 = DIRECTION ( 'NONE',  ( 0.000000000000000000, 1.000000000000000000, 0.000000000000000000 ) ) ;
#92338 = FACE_OUTER_BOUND ( 'NONE', #14132, .T. ) ;
#92339 = ORIENTED_EDGE ( 'NONE', *, *, #19553, .T. ) ;
#92340 = ADVANCED_FACE ( 'NONE', ( #35217 ), #125695, .T. ) ;
#92341 = ORIENTED_EDGE ( 'NONE', *, *, #10568, .T. ) ;
#92342 = VERTEX_POINT ( 'NONE', #63375 ) ;
#92343 = DIRECTION ( 'NONE',  ( -0.000000000000000000, -1.000000000000000000, -0.000000000000000000 ) ) ;
#92344 = VERTEX_POINT ( 'NONE', #113768 ) ;
#92345 = DIRECTION ( 'NONE',  ( 0.000000000000000000, 0.000000000000000000, 1.000000000000000000 ) ) ;
#92346 = CIRCLE ( 'NONE', #4583, 0.1000000000000002554 ) ;
#92347 = CARTESIAN_POINT ( 'NONE',  ( -6.850000000000013856, 12.50000000000000000, 1.818653347947321475 ) ) ;
#92348 = AXIS2_PLACEMENT_3D ( 'NONE', #98932, #40021, #79930 ) ;
#92349 = ORIENTED_EDGE ( 'NONE', *, *, #3585, .T. ) ;
#92350 = CARTESIAN_POINT ( 'NONE',  ( 133.2169897921533845, 2.500000000000000000, -0.01898911740318533561 ) ) ;
#92351 = DIRECTION ( 'NONE',  ( 0.000000000000000000, 0.000000000000000000, -1.000000000000000000 ) ) ;
#92352 = EDGE_CURVE ( 'NONE', #34347, #65457, #121592, .T. ) ;
#92353 = CARTESIAN_POINT ( 'NONE',  ( 5.399999999999934630, 12.50000000000000000, 0.6928203230275494784 ) ) ;
#92354 = DIRECTION ( 'NONE',  ( 0.000000000000000000, -0.000000000000000000, 1.000000000000000000 ) ) ;
#92355 = VECTOR ( 'NONE', #66613, 1000.000000000000000 ) ;
#92356 = VECTOR ( 'NONE', #74284, 1000.000000000000000 ) ;
#92357 = AXIS2_PLACEMENT_3D ( 'NONE', #69463, #128428, #99594 ) ;
#92358 = CARTESIAN_POINT ( 'NONE',  ( -9.400000000000007461, 2.500000000000000000, 3.983716857408420076 ) ) ;
#92359 = CONICAL_SURFACE ( 'NONE', #109070, 0.1000000000000000056, 0.003490658503988666988 ) ;
#92360 = CIRCLE ( 'NONE', #75627, 0.06509327318403745899 ) ;
#92361 = ORIENTED_EDGE ( 'NONE', *, *, #88900, .F. ) ;
#92362 = ORIENTED_EDGE ( 'NONE', *, *, #61659, .F. ) ;
#92363 = CARTESIAN_POINT ( 'NONE',  ( 187.1249999999999716, -8.891194145520236347, -1.633285867636356299E-15 ) ) ;
#92364 = DIRECTION ( 'NONE',  ( 0.000000000000000000, 0.000000000000000000, -1.000000000000000000 ) ) ;
#92365 = CARTESIAN_POINT ( 'NONE',  ( -9.150000000000005684, 2.500000000000000000, 6.595190528383296780 ) ) ;
#92366 = CIRCLE ( 'NONE', #104884, 0.1000000000000002554 ) ;
#92368 = PLANE ( 'NONE',  #39682 ) ;
#92367 = AXIS2_PLACEMENT_3D ( 'NONE', #95140, #93213, #15255 ) ;
#92369 = VERTEX_POINT ( 'NONE', #13610 ) ;
#92370 = AXIS2_PLACEMENT_3D ( 'NONE', #15259, #87235, #15917 ) ;
#92371 = VECTOR ( 'NONE', #124521, 1000.000000000000000 ) ;
#92372 = AXIS2_PLACEMENT_3D ( 'NONE', #78933, #126068, #117513 ) ;
#92373 = ORIENTED_EDGE ( 'NONE', *, *, #116646, .F. ) ;
#92374 = FACE_OUTER_BOUND ( 'NONE', #98495, .T. ) ;
#92375 = LINE ( 'NONE', #72113, #53016 ) ;
#92376 = CONICAL_SURFACE ( 'NONE', #79866, 0.1000000000000000472, 0.003490658503988666988 ) ;
#92377 = CARTESIAN_POINT ( 'NONE',  ( 11.04999999999990834, 12.50000000000000000, 1.818653347947321475 ) ) ;
#92378 = CARTESIAN_POINT ( 'NONE',  ( 3.149999999999942624, 2.500000000000000000, 6.941600689897073018 ) ) ;
#92379 = ORIENTED_EDGE ( 'NONE', *, *, #40232, .F. ) ;
#92380 = CARTESIAN_POINT ( 'NONE',  ( 3.949999999999939782, 12.50000000000000000, 2.576566944158910744 ) ) ;
#92381 = EDGE_CURVE ( 'NONE', #30567, #117617, #102709, .T. ) ;
#92382 = DIRECTION ( 'NONE',  ( 0.000000000000000000, 0.000000000000000000, 1.000000000000000000 ) ) ;
#92383 = VECTOR ( 'NONE', #13843, 1000.000000000000000 ) ;
#92384 = ORIENTED_EDGE ( 'NONE', *, *, #56967, .T. ) ;
#92385 = CARTESIAN_POINT ( 'NONE',  ( 115.5000000000000000, 2.000000000000000000, -4.999999999999997335 ) ) ;
#92386 = ORIENTED_EDGE ( 'NONE', *, *, #20023, .T. ) ;
#92387 = CARTESIAN_POINT ( 'NONE',  ( 6.049999999999935874, 12.50000000000000000, -6.841600689897077814 ) ) ;
#92388 = VERTEX_POINT ( 'NONE', #43117 ) ;
#92389 = DIRECTION ( 'NONE',  ( 0.000000000000000000, 0.000000000000000000, 1.000000000000000000 ) ) ;
#92390 = CARTESIAN_POINT ( 'NONE',  ( 2.499999999999983569, 2.500000000000000000, -2.276824562219559311E-15 ) ) ;
#92391 = EDGE_CURVE ( 'NONE', #60385, #90590, #96456, .T. ) ;
#92392 = VERTEX_POINT ( 'NONE', #15539 ) ;
#92393 = EDGE_CURVE ( 'NONE', #114671, #5769, #119441, .T. ) ;
#92394 = ORIENTED_EDGE ( 'NONE', *, *, #29784, .F. ) ;
#92395 = ADVANCED_FACE ( 'NONE', ( #83662 ), #98596, .T. ) ;
#92396 = EDGE_CURVE ( 'NONE', #80227, #117538, #21247, .T. ) ;
#92397 = DIRECTION ( 'NONE',  ( -0.000000000000000000, 1.000000000000000000, -0.000000000000000000 ) ) ;
#92398 = CARTESIAN_POINT ( 'NONE',  ( 6.049999999999930544, 12.50000000000000000, 2.446380397790835826 ) ) ;
#92399 = DIRECTION ( 'NONE',  ( 0.000000000000000000, 0.000000000000000000, 1.000000000000000000 ) ) ;
#92400 = CARTESIAN_POINT ( 'NONE',  ( 185.4010416670080872, -4.367472073101520635, 7.564683531249999149 ) ) ;
#92401 = PLANE ( 'NONE',  #129051 ) ;
#92402 = CONICAL_SURFACE ( 'NONE', #56882, 0.1000000000000002554, 0.003490658503988666988 ) ;
#92403 = FACE_OUTER_BOUND ( 'NONE', #54659, .T. ) ;
#92404 = CARTESIAN_POINT ( 'NONE',  ( -2.500000000000030642, 12.50000000000000000, -5.022947341949754119 ) ) ;
#92405 = AXIS2_PLACEMENT_3D ( 'NONE', #38124, #116035, #46657 ) ;
#92406 = CONICAL_SURFACE ( 'NONE', #109119, 0.1000000000000002554, 0.003490658503988666988 ) ;
#92407 = FACE_OUTER_BOUND ( 'NONE', #1012, .T. ) ;
#92408 = CARTESIAN_POINT ( 'NONE',  ( 6.849999999999929479, 2.500000000000000000, -2.611473670974877592 ) ) ;
#92409 = ADVANCED_FACE ( 'NONE', ( #96672 ), #78361, .T. ) ;
#92410 = EDGE_CURVE ( 'NONE', #107267, #113689, #58915, .T. ) ;
#92411 = EDGE_CURVE ( 'NONE', #64286, #27855, #111112, .T. ) ;
#92413 = ORIENTED_EDGE ( 'NONE', *, *, #92393, .F. ) ;
#92412 = AXIS2_PLACEMENT_3D ( 'NONE', #96193, #6498, #77219 ) ;
#92414 = EDGE_LOOP ( 'NONE', ( #105031, #128574, #21121, #539 ) ) ;
#92415 = CARTESIAN_POINT ( 'NONE',  ( 8.149999999999920419, 12.50000000000000000, 6.148780366869520897 ) ) ;
#92416 = ORIENTED_EDGE ( 'NONE', *, *, #74525, .F. ) ;
#92417 = DIRECTION ( 'NONE',  ( 0.000000000000000000, 0.000000000000000000, 1.000000000000000000 ) ) ;
#92418 = DIRECTION ( 'NONE',  ( 0.000000000000000000, 0.000000000000000000, 1.000000000000000000 ) ) ;
#92419 = CIRCLE ( 'NONE', #40204, 0.09999999999999982514 ) ;
#92420 = DIRECTION ( 'NONE',  ( -0.000000000000000000, 1.000000000000000000, -0.000000000000000000 ) ) ;
#92423 = ORIENTED_EDGE ( 'NONE', *, *, #54716, .F. ) ;
#92422 = ORIENTED_EDGE ( 'NONE', *, *, #10561, .T. ) ;
#92421 = CIRCLE ( 'NONE', #23466, 0.09999999999999982514 ) ;
#92424 = PRODUCT_DEFINITION ( 'UNKNOWN', '', #77694, #55901 ) ;
#92425 = FACE_BOUND ( 'NONE', #21530, .T. ) ;
#92426 = ORIENTED_EDGE ( 'NONE', *, *, #29071, .T. ) ;
#92427 = CARTESIAN_POINT ( 'NONE',  ( 11.04999999999990656, 2.500000000000000000, -6.148780366869526226 ) ) ;
#92428 = CARTESIAN_POINT ( 'NONE',  ( 18.09027855933886997, -2.526462839860863507, 2.685672775344717156 ) ) ;
#92429 = VECTOR ( 'NONE', #75739, 1000.000000000000000 ) ;
#92430 = LINE ( 'NONE', #32890, #65965 ) ;
#92431 = CARTESIAN_POINT ( 'NONE',  ( 10.64999999999990976, 2.500000000000000000, 1.818653347947321475 ) ) ;
#92432 = FACE_OUTER_BOUND ( 'NONE', #34748, .T. ) ;
#92433 = DIRECTION ( 'NONE',  ( -0.000000000000000000, -1.000000000000000000, -0.000000000000000000 ) ) ;
#92434 = CARTESIAN_POINT ( 'NONE',  ( -10.84999999999999964, 12.50000000000000000, 7.188010851410848723 ) ) ;
#92435 = CARTESIAN_POINT ( 'NONE',  ( -11.84999999999999787, 12.50000000000000000, -6.841600689897074261 ) ) ;
#92436 = CARTESIAN_POINT ( 'NONE',  ( 7.699999999999923794, 12.50000000000000000, -0.3464101615137783474 ) ) ;
#92437 = CARTESIAN_POINT ( 'NONE',  ( -3.750000000000025757, 12.50000000000000000, -2.857883832488653741 ) ) ;
#92438 = DIRECTION ( 'NONE',  ( -0.000000000000000000, 1.000000000000000000, -0.000000000000000000 ) ) ;
#92439 = ORIENTED_EDGE ( 'NONE', *, *, #28433, .F. ) ;
#92440 = ORIENTED_EDGE ( 'NONE', *, *, #97191, .T. ) ;
#92441 = ORIENTED_EDGE ( 'NONE', *, *, #81594, .T. ) ;
#92442 = DIRECTION ( 'NONE',  ( -0.000000000000000000, 1.000000000000000000, -0.000000000000000000 ) ) ;
#92443 = EDGE_LOOP ( 'NONE', ( #102818, #116392, #28687, #36876 ) ) ;
#92444 = CARTESIAN_POINT ( 'NONE',  ( -1.250000000000037526, 12.50000000000000000, -5.802370205355749988 ) ) ;
#92445 = CARTESIAN_POINT ( 'NONE',  ( -8.550000000000009592, 2.500000000000000000, 6.741600689897071952 ) ) ;
#92447 = ORIENTED_EDGE ( 'NONE', *, *, #10991, .T. ) ;
#92446 = ORIENTED_EDGE ( 'NONE', *, *, #103233, .T. ) ;
#92448 = ORIENTED_EDGE ( 'NONE', *, *, #111341, .F. ) ;
#92449 = CARTESIAN_POINT ( 'NONE',  ( -11.44999999999999751, 12.50000000000000000, 6.148780366869520897 ) ) ;
#92450 = DIRECTION ( 'NONE',  ( 0.000000000000000000, 0.000000000000000000, -1.000000000000000000 ) ) ;
#92451 =( LENGTH_UNIT ( ) NAMED_UNIT ( * ) SI_UNIT ( .MILLI., .METRE. ) );
#92452 = DIRECTION ( 'NONE',  ( 0.000000000000000000, 0.000000000000000000, 1.000000000000000000 ) ) ;
#92453 = DIRECTION ( 'NONE',  ( 0.000000000000000000, 1.000000000000000000, 0.000000000000000000 ) ) ;
#92454 = PLANE ( 'NONE',  #78961 ) ;
#92455 = ORIENTED_EDGE ( 'NONE', *, *, #6715, .F. ) ;
#92456 = CONICAL_SURFACE ( 'NONE', #59013, 0.1000000000000002554, 0.003490658503988666988 ) ;
#92457 = CIRCLE ( 'NONE', #27699, 0.1000000000000002554 ) ;
#92458 = FACE_OUTER_BOUND ( 'NONE', #92023, .T. ) ;
#92459 = ORIENTED_EDGE ( 'NONE', *, *, #42622, .T. ) ;
#92460 = ADVANCED_FACE ( 'NONE', ( #97977 ), #77682, .T. ) ;
#92461 = AXIS2_PLACEMENT_3D ( 'NONE', #78772, #119967, #49318 ) ;
#92462 = VERTEX_POINT ( 'NONE', #126806 ) ;
#92463 = AXIS2_PLACEMENT_3D ( 'NONE', #28451, #125349, #77529 ) ;
#92464 = ORIENTED_EDGE ( 'NONE', *, *, #1237, .T. ) ;
#92465 = EDGE_CURVE ( 'NONE', #25375, #70406, #14954, .T. ) ;
#92466 = ORIENTED_EDGE ( 'NONE', *, *, #104111, .F. ) ;
#92467 = ORIENTED_EDGE ( 'NONE', *, *, #8777, .T. ) ;
#92468 = ORIENTED_EDGE ( 'NONE', *, *, #12754, .F. ) ;
#92469 = AXIS2_PLACEMENT_3D ( 'NONE', #77253, #97526, #47153 ) ;
#92470 = CARTESIAN_POINT ( 'NONE',  ( 9.399999999999915090, 2.500000000000000000, 3.883716857408421319 ) ) ;
#92471 = ADVANCED_FACE ( 'NONE', ( #87500 ), #75529, .T. ) ;
#92472 = CIRCLE ( 'NONE', #6666, 0.06509327318403743123 ) ;
#92473 = DIRECTION ( 'NONE',  ( 0.000000000000000000, 1.000000000000000000, 0.000000000000000000 ) ) ;
#92474 = DIRECTION ( 'NONE',  ( 0.000000000000000000, 1.000000000000000000, 0.000000000000000000 ) ) ;
#92475 = CIRCLE ( 'NONE', #121711, 0.1000000000000002554 ) ;
#92476 = PLANE ( 'NONE',  #124368 ) ;
#92477 = CONICAL_SURFACE ( 'NONE', #6765, 0.1000000000000000472, 0.003490658503988666988 ) ;
#92478 = VECTOR ( 'NONE', #102893, 1000.000000000000000 ) ;
#92479 = FACE_OUTER_BOUND ( 'NONE', #73345, .T. ) ;
#92480 = DIRECTION ( 'NONE',  ( -0.000000000000000000, -1.000000000000000000, -0.000000000000000000 ) ) ;
#92481 = ORIENTED_EDGE ( 'NONE', *, *, #17914, .F. ) ;
#92482 = DIRECTION ( 'NONE',  ( 0.000000000000000000, 1.000000000000000000, 0.000000000000000000 ) ) ;
#92483 = ORIENTED_EDGE ( 'NONE', *, *, #26685, .T. ) ;
#92484 = AXIS2_PLACEMENT_3D ( 'NONE', #35291, #54274, #24813 ) ;
#92485 = CARTESIAN_POINT ( 'NONE',  ( 5.599999999999934808, 2.500000000000000000, -4.776537180435978414 ) ) ;
#92486 = ORIENTED_EDGE ( 'NONE', *, *, #98480, .T. ) ;
#92487 = DIRECTION ( 'NONE',  ( -0.000000000000000000, -1.000000000000000000, -0.000000000000000000 ) ) ;
#92488 = ORIENTED_EDGE ( 'NONE', *, *, #49759, .T. ) ;
#92489 = DIRECTION ( 'NONE',  ( -0.000000000000000000, 1.000000000000000000, -0.000000000000000000 ) ) ;
#92490 = DIRECTION ( 'NONE',  ( 0.000000000000000000, 0.000000000000000000, 1.000000000000000000 ) ) ;
#92491 = ORIENTED_EDGE ( 'NONE', *, *, #65772, .T. ) ;
#92492 = ORIENTED_EDGE ( 'NONE', *, *, #107516, .T. ) ;
#92493 = CARTESIAN_POINT ( 'NONE',  ( 1.249999999999952038, 2.500000000000000000, 5.802370205355744659 ) ) ;
#92494 = LINE ( 'NONE', #4106, #11764 ) ;
#92495 = AXIS2_PLACEMENT_3D ( 'NONE', #114074, #104254, #4102 ) ;
#92496 = FACE_OUTER_BOUND ( 'NONE', #48508, .T. ) ;
#92497 = DIRECTION ( 'NONE',  ( 0.000000000000000000, 0.000000000000000000, 1.000000000000000000 ) ) ;
#92498 = CARTESIAN_POINT ( 'NONE',  ( 3.549999999999941203, 12.50000000000000000, 6.083687093685483660 ) ) ;
#92499 = ORIENTED_EDGE ( 'NONE', *, *, #67985, .F. ) ;
#92500 = EDGE_CURVE ( 'NONE', #45029, #18481, #79747, .T. ) ;
#92501 = FACE_OUTER_BOUND ( 'NONE', #58382, .T. ) ;
#92502 = AXIS2_PLACEMENT_3D ( 'NONE', #14626, #4812, #23838 ) ;
#92503 = AXIS2_PLACEMENT_3D ( 'NONE', #44468, #85029, #95504 ) ;
#92504 = AXIS2_PLACEMENT_3D ( 'NONE', #93614, #112618, #43246 ) ;
#92505 = ORIENTED_EDGE ( 'NONE', *, *, #99513, .F. ) ;
#92506 = CARTESIAN_POINT ( 'NONE',  ( -3.100000000000028511, 2.500000000000000000, -4.083716857408426826 ) ) ;
#92507 = DIRECTION ( 'NONE',  ( 0.000000000000000000, 1.000000000000000000, 0.000000000000000000 ) ) ;
#92508 = AXIS2_PLACEMENT_3D ( 'NONE', #47741, #38582, #117736 ) ;
#92509 = CONICAL_SURFACE ( 'NONE', #82150, 0.09999999999999982514, 0.003490658503988666988 ) ;
#92511 = EDGE_CURVE ( 'NONE', #24530, #110285, #33770, .T. ) ;
#92510 = VECTOR ( 'NONE', #77159, 1000.000000000000000 ) ;
#92512 = VECTOR ( 'NONE', #47721, 1000.000000000000000 ) ;
#92513 = CARTESIAN_POINT ( 'NONE',  ( 187.2083333333333428, -4.445597072760115509, -7.700000000000001954 ) ) ;
#92514 = DIRECTION ( 'NONE',  ( 0.000000000000000000, 0.000000000000000000, 1.000000000000000000 ) ) ;
#92515 = DIRECTION ( 'NONE',  ( 0.000000000000000000, 0.000000000000000000, -1.000000000000000000 ) ) ;
#92516 = ADVANCED_FACE ( 'NONE', ( #26672 ), #117451, .T. ) ;
#92517 = DIRECTION ( 'NONE',  ( 0.000000000000000000, 0.000000000000000000, -1.000000000000000000 ) ) ;
#92518 = DIRECTION ( 'NONE',  ( -0.000000000000000000, -1.000000000000000000, -0.000000000000000000 ) ) ;
#92519 = ORIENTED_EDGE ( 'NONE', *, *, #48253, .T. ) ;
#92520 = VECTOR ( 'NONE', #63202, 1000.000000000000000 ) ;
#92521 = FACE_OUTER_BOUND ( 'NONE', #62328, .T. ) ;
#92522 = CARTESIAN_POINT ( 'NONE',  ( 3.099999999999945022, 2.500000000000000000, -4.676537180435978769 ) ) ;
#92523 = LINE ( 'NONE', #41523, #129180 ) ;
#92524 = VERTEX_POINT ( 'NONE', #126156 ) ;
#92525 = EDGE_CURVE ( 'NONE', #110490, #88966, #38442, .T. ) ;
#92526 = ORIENTED_EDGE ( 'NONE', *, *, #99074, .F. ) ;
#92527 = DIRECTION ( 'NONE',  ( 0.000000000000000000, 0.000000000000000000, 1.000000000000000000 ) ) ;
#92528 = ORIENTED_EDGE ( 'NONE', *, *, #13888, .F. ) ;
#92529 = VERTEX_POINT ( 'NONE', #77057 ) ;
#92530 = DIRECTION ( 'NONE',  ( 0.000000000000000000, 0.000000000000000000, 1.000000000000000000 ) ) ;
#92531 = ORIENTED_EDGE ( 'NONE', *, *, #3279, .F. ) ;
#92532 = CARTESIAN_POINT ( 'NONE',  ( 17.17539648375208472, -2.541523116373817892, -5.507477068185379743 ) ) ;
#92533 = DIRECTION ( 'NONE',  ( 0.000000000000000000, -0.000000000000000000, 1.000000000000000000 ) ) ;
#92534 = DIRECTION ( 'NONE',  ( -0.000000000000000000, 1.000000000000000000, -0.000000000000000000 ) ) ;
#92535 = CIRCLE ( 'NONE', #90375, 0.1000000000000000472 ) ;
#92536 = ORIENTED_EDGE ( 'NONE', *, *, #56503, .T. ) ;
#92537 = AXIS2_PLACEMENT_3D ( 'NONE', #74372, #96570, #114292 ) ;
#92538 = CIRCLE ( 'NONE', #117554, 0.06509327318403745899 ) ;
#92539 = DIRECTION ( 'NONE',  ( 0.000000000000000000, 0.000000000000000000, 1.000000000000000000 ) ) ;
#92540 = EDGE_CURVE ( 'NONE', #10375, #65577, #104947, .T. ) ;
#92541 = CARTESIAN_POINT ( 'NONE',  ( 9.149999999999918643, 2.500000000000000000, 2.265063509461097357 ) ) ;
#92542 = AXIS2_PLACEMENT_3D ( 'NONE', #53750, #3362, #101080 ) ;
#92543 = ORIENTED_EDGE ( 'NONE', *, *, #126610, .F. ) ;
#92544 = AXIS2_PLACEMENT_3D ( 'NONE', #73169, #82360, #3145 ) ;
#92546 = EDGE_CURVE ( 'NONE', #72305, #81664, #73560, .T. ) ;
#92545 = CONICAL_SURFACE ( 'NONE', #94695, 0.09999999999999999167, 0.003490658503988666988 ) ;
#92547 = VECTOR ( 'NONE', #102804, 1000.000000000000000 ) ;
#92548 = ORIENTED_EDGE ( 'NONE', *, *, #59953, .T. ) ;
#92549 = VERTEX_POINT ( 'NONE', #8941 ) ;
#92550 = DIRECTION ( 'NONE',  ( 0.000000000000000000, 0.000000000000000000, -1.000000000000000000 ) ) ;
#92551 = CARTESIAN_POINT ( 'NONE',  ( -1.250000000000001554, 12.50000000000000000, 2.165063509461097713 ) ) ;
#92552 = CARTESIAN_POINT ( 'NONE',  ( 1.899999999999951283, 2.500000000000000000, -0.3464101615137782364 ) ) ;
#92553 = EDGE_CURVE ( 'NONE', #7138, #35674, #85584, .T. ) ;
#92554 = EDGE_CURVE ( 'NONE', #48072, #27240, #119535, .T. ) ;
#92555 = FACE_BOUND ( 'NONE', #128012, .T. ) ;
#92556 = ORIENTED_EDGE ( 'NONE', *, *, #53104, .T. ) ;
#92557 = ADVANCED_FACE ( 'NONE', ( #75754 ), #35918, .T. ) ;
#92558 = EDGE_CURVE ( 'NONE', #68909, #98740, #25531, .T. ) ;
#92559 = CARTESIAN_POINT ( 'NONE',  ( -4.600000000000025402, 2.500000000000000000, 4.430127018922196847 ) ) ;
#92560 = CARTESIAN_POINT ( 'NONE',  ( -3.750000000000025757, 12.50000000000000000, 1.472243186433545459 ) ) ;
#92561 = CIRCLE ( 'NONE', #52857, 0.06509327318403745899 ) ;
#92562 = VERTEX_POINT ( 'NONE', #60019 ) ;
#92563 = DIRECTION ( 'NONE',  ( 0.000000000000000000, -0.9999939076577903929, 0.003490651415223739937 ) ) ;
#92564 = LINE ( 'NONE', #31718, #78477 ) ;
#92565 = CIRCLE ( 'NONE', #103022, 0.1000000000000000056 ) ;
#92566 = CIRCLE ( 'NONE', #90501, 0.1000000000000000472 ) ;
#92567 = AXIS2_PLACEMENT_3D ( 'NONE', #27544, #39974, #107414 ) ;
#92568 = EDGE_CURVE ( 'NONE', #69557, #38337, #38077, .T. ) ;
#92569 = LINE ( 'NONE', #44106, #36073 ) ;
#92570 = DIRECTION ( 'NONE',  ( 0.000000000000000000, -0.000000000000000000, 1.000000000000000000 ) ) ;
#92571 = CARTESIAN_POINT ( 'NONE',  ( 14.19999999999989626, 2.500000000000000000, 0.09999999999999772959 ) ) ;
#92572 = EDGE_CURVE ( 'NONE', #59496, #76961, #60653, .T. ) ;
#92573 = DIRECTION ( 'NONE',  ( -0.000000000000000000, 1.000000000000000000, -0.000000000000000000 ) ) ;
#92574 = AXIS2_PLACEMENT_3D ( 'NONE', #27348, #96737, #56805 ) ;
#92575 = PLANE ( 'NONE',  #35779 ) ;
#92576 = EDGE_CURVE ( 'NONE', #109878, #24253, #41021, .T. ) ;
#92577 = EDGE_CURVE ( 'NONE', #113875, #16833, #92346, .T. ) ;
#92578 = EDGE_LOOP ( 'NONE', ( #34001, #38925, #113662, #15151 ) ) ;
#92579 = AXIS2_PLACEMENT_3D ( 'NONE', #1148, #100005, #40455 ) ;
#92580 = ORIENTED_EDGE ( 'NONE', *, *, #58801, .T. ) ;
#92581 = ORIENTED_EDGE ( 'NONE', *, *, #46156, .T. ) ;
#92582 = ORIENTED_EDGE ( 'NONE', *, *, #42961, .F. ) ;
#92583 = CARTESIAN_POINT ( 'NONE',  ( 9.149999999999915090, 2.500000000000000000, 6.495190528383297135 ) ) ;
#92584 = CARTESIAN_POINT ( 'NONE',  ( 194.5000000000000000, 4.898587196589412829E-16, 4.000000000000000000 ) ) ;
#92585 = LINE ( 'NONE', #103037, #40457 ) ;
#92586 = ORIENTED_EDGE ( 'NONE', *, *, #56798, .T. ) ;
#92587 = FACE_BOUND ( 'NONE', #120703, .T. ) ;
#92588 = ADVANCED_FACE ( 'NONE', ( #39089 ), #111210, .T. ) ;
#92589 = CARTESIAN_POINT ( 'NONE',  ( -10.85000000000000142, 2.500000000000000000, -2.857883832488649745 ) ) ;
#92590 = DIRECTION ( 'NONE',  ( 0.000000000000000000, 0.000000000000000000, 1.000000000000000000 ) ) ;
#92591 = CARTESIAN_POINT ( 'NONE',  ( 7.099999999999928590, 2.500000000000000000, 4.230127018922196669 ) ) ;
#92592 = DIRECTION ( 'NONE',  ( -0.000000000000000000, -1.000000000000000000, -0.000000000000000000 ) ) ;
#92593 = CARTESIAN_POINT ( 'NONE',  ( -6.249999999999981348, 2.500000000000000000, 6.495190528383297135 ) ) ;
#92594 = DIRECTION ( 'NONE',  ( -4.274815082592931898E-19, -0.9999939076577903929, -0.003490651415223739937 ) ) ;
#92595 = PLANE ( 'NONE',  #116797 ) ;
#92596 = CARTESIAN_POINT ( 'NONE',  ( 13.94999999999989271, 2.500000000000000000, -1.818653347947326138 ) ) ;
#92597 = AXIS2_PLACEMENT_3D ( 'NONE', #20988, #71363, #19038 ) ;
#92598 = DIRECTION ( 'NONE',  ( 0.000000000000000000, -0.000000000000000000, 1.000000000000000000 ) ) ;
#92599 = VERTEX_POINT ( 'NONE', #120208 ) ;
#92600 = CIRCLE ( 'NONE', #115557, 0.06509327318403745899 ) ;
#92601 = VERTEX_POINT ( 'NONE', #99927 ) ;
#92602 = EDGE_LOOP ( 'NONE', ( #57043, #2640 ) ) ;
#92603 = ORIENTED_EDGE ( 'NONE', *, *, #4896, .T. ) ;
#92604 = ORIENTED_EDGE ( 'NONE', *, *, #122178, .F. ) ;
#92605 = CIRCLE ( 'NONE', #34117, 0.09999999999999982514 ) ;
#92606 = ORIENTED_EDGE ( 'NONE', *, *, #121573, .T. ) ;
#92607 = CIRCLE ( 'NONE', #27844, 0.1000000000000002554 ) ;
#92608 = FACE_OUTER_BOUND ( 'NONE', #99361, .T. ) ;
#92609 = VERTEX_POINT ( 'NONE', #50823 ) ;
#92610 = ORIENTED_EDGE ( 'NONE', *, *, #15461, .T. ) ;
#92611 = CIRCLE ( 'NONE', #4855, 0.1000000000000002554 ) ;
#92612 = CONICAL_SURFACE ( 'NONE', #17366, 0.1000000000000002554, 0.003490658503988666988 ) ;
#92613 = CARTESIAN_POINT ( 'NONE',  ( 13.39053294345136003, -2.499999999999999556, 7.037281288959354342 ) ) ;
#92614 = FACE_OUTER_BOUND ( 'NONE', #103629, .T. ) ;
#92615 = DIRECTION ( 'NONE',  ( -0.000000000000000000, 1.000000000000000000, -0.000000000000000000 ) ) ;
#92616 = CONICAL_SURFACE ( 'NONE', #109331, 0.09999999999999982514, 0.003490658503988666988 ) ;
#92617 = ORIENTED_EDGE ( 'NONE', *, *, #92224, .F. ) ;
#92618 = DIRECTION ( 'NONE',  ( 0.000000000000000000, 0.000000000000000000, 1.000000000000000000 ) ) ;
#92619 = CIRCLE ( 'NONE', #126055, 0.06509327318403745899 ) ;
#92620 = VERTEX_POINT ( 'NONE', #31195 ) ;
#92621 = EDGE_CURVE ( 'NONE', #89101, #64737, #8806, .T. ) ;
#92622 = VERTEX_POINT ( 'NONE', #89452 ) ;
#92623 = CARTESIAN_POINT ( 'NONE',  ( 129.5000000000000000, 0.6250000000000000000, 7.634788798650556707 ) ) ;
#92624 = EDGE_CURVE ( 'NONE', #20674, #99703, #81984, .T. ) ;
#92625 = CARTESIAN_POINT ( 'NONE',  ( 108.0000000000000142, 8.500000000000000000, -5.000000000000004441 ) ) ;
#92626 = ORIENTED_EDGE ( 'NONE', *, *, #124594, .T. ) ;
#92627 = ORIENTED_EDGE ( 'NONE', *, *, #86531, .F. ) ;
#92628 = CONICAL_SURFACE ( 'NONE', #107291, 0.1000000000000002554, 0.003490658503988666988 ) ;
#92629 = DIRECTION ( 'NONE',  ( 0.000000000000000000, 1.000000000000000000, 0.000000000000000000 ) ) ;
#92630 = CARTESIAN_POINT ( 'NONE',  ( 10.79999999999991012, 12.50000000000000000, 4.395220292106234439 ) ) ;
#92631 = DIRECTION ( 'NONE',  ( -0.000000000000000000, 1.000000000000000000, -0.000000000000000000 ) ) ;
#92632 = DIRECTION ( 'NONE',  ( 0.000000000000000000, 0.000000000000000000, 1.000000000000000000 ) ) ;
#92633 = LINE ( 'NONE', #366, #112970 ) ;
#92635 = ORIENTED_EDGE ( 'NONE', *, *, #112791, .T. ) ;
#92634 = CONICAL_SURFACE ( 'NONE', #46561, 0.09999999999999999167, 0.003490658503988666988 ) ;
#92636 = CARTESIAN_POINT ( 'NONE',  ( 13.54999999999989946, 12.50000000000000000, 2.576566944158910744 ) ) ;
#92637 = AXIS2_PLACEMENT_3D ( 'NONE', #122042, #61839, #20617 ) ;
#92638 = AXIS2_PLACEMENT_3D ( 'NONE', #41053, #53437, #80959 ) ;
#92639 = ORIENTED_EDGE ( 'NONE', *, *, #71291, .T. ) ;
#92640 = DIRECTION ( 'NONE',  ( -0.000000000000000000, -1.000000000000000000, -0.000000000000000000 ) ) ;
#92641 = ORIENTED_EDGE ( 'NONE', *, *, #22674, .T. ) ;
#92642 = DIRECTION ( 'NONE',  ( 0.000000000000000000, 1.000000000000000000, 0.000000000000000000 ) ) ;
#92643 = LINE ( 'NONE', #21315, #88662 ) ;
#92644 = DIRECTION ( 'NONE',  ( 0.000000000000000000, -0.9999939076577903929, 0.003490651415223739937 ) ) ;
#92646 = VECTOR ( 'NONE', #56161, 1000.000000000000000 ) ;
#92645 = LINE ( 'NONE', #4890, #2013 ) ;
#92647 = ORIENTED_EDGE ( 'NONE', *, *, #116288, .F. ) ;
#92648 = CONICAL_SURFACE ( 'NONE', #11160, 0.1000000000000002554, 0.003490658503988666988 ) ;
#92649 = VECTOR ( 'NONE', #41268, 1000.000000000000000 ) ;
#92650 = DIRECTION ( 'NONE',  ( -0.000000000000000000, 1.000000000000000000, -0.000000000000000000 ) ) ;
#92651 = AXIS2_PLACEMENT_3D ( 'NONE', #109424, #108129, #119239 ) ;
#92652 = DIRECTION ( 'NONE',  ( 0.000000000000000000, 1.000000000000000000, 0.000000000000000000 ) ) ;
#92653 = VERTEX_POINT ( 'NONE', #39737 ) ;
#92654 = EDGE_LOOP ( 'NONE', ( #21736, #14089, #15209, #15437 ) ) ;
#92655 = ORIENTED_EDGE ( 'NONE', *, *, #121688, .T. ) ;
#92656 = FACE_OUTER_BOUND ( 'NONE', #117071, .T. ) ;
#92657 = DIRECTION ( 'NONE',  ( 0.000000000000000000, 0.000000000000000000, 1.000000000000000000 ) ) ;
#92658 = CARTESIAN_POINT ( 'NONE',  ( 186.2760416670080588, 6.551208109652274736, 3.782341765625001351 ) ) ;
#92659 = CIRCLE ( 'NONE', #98608, 0.06509327318403741736 ) ;
#92660 = CARTESIAN_POINT ( 'NONE',  ( 11.44999999999990692, 2.500000000000000000, 1.718653347947321386 ) ) ;
#92661 = CARTESIAN_POINT ( 'NONE',  ( -8.350000000000013856, 2.500000000000000000, -6.395190528383296602 ) ) ;
#92662 = ADVANCED_FACE ( 'NONE', ( #111000 ), #96538, .T. ) ;
#92663 = DIRECTION ( 'NONE',  ( 0.000000000000000000, 1.000000000000000000, 0.000000000000000000 ) ) ;
#92664 = AXIS2_PLACEMENT_3D ( 'NONE', #19274, #100433, #40227 ) ;
#92665 = CIRCLE ( 'NONE', #96851, 0.06509327318403745899 ) ;
#92666 = AXIS2_PLACEMENT_3D ( 'NONE', #18222, #47708, #88915 ) ;
#92667 = CARTESIAN_POINT ( 'NONE',  ( -2.950000000000030376, 2.500000000000000000, 6.595190528383296780 ) ) ;
#92668 = CIRCLE ( 'NONE', #126005, 0.1000000000000000056 ) ;
#92669 = EDGE_CURVE ( 'NONE', #86369, #125929, #90741, .T. ) ;
#92670 = DIRECTION ( 'NONE',  ( 0.000000000000000000, -0.000000000000000000, 1.000000000000000000 ) ) ;
#92671 = VERTEX_POINT ( 'NONE', #101212 ) ;
#92672 = CARTESIAN_POINT ( 'NONE',  ( -5.800000000000018474, 12.50000000000000000, -2.276824562219559311E-15 ) ) ;
#92673 = EDGE_CURVE ( 'NONE', #80874, #13926, #11531, .T. ) ;
#92675 = ADVANCED_FACE ( 'NONE', ( #118910 ), #40139, .T. ) ;
#92674 = CYLINDRICAL_SURFACE ( 'NONE', #89323, 7.500000000000000000 ) ;
#92676 = DIRECTION ( 'NONE',  ( 0.000000000000000000, 0.000000000000000000, -1.000000000000000000 ) ) ;
#92677 = DIRECTION ( 'NONE',  ( 0.000000000000000000, 0.000000000000000000, 1.000000000000000000 ) ) ;
#92678 = EDGE_LOOP ( 'NONE', ( #119427, #120512 ) ) ;
#92679 = DIRECTION ( 'NONE',  ( 0.000000000000000000, 1.000000000000000000, 0.000000000000000000 ) ) ;
#92680 = CARTESIAN_POINT ( 'NONE',  ( 1.049999999999954525, 2.500000000000000000, -2.411473670974877859 ) ) ;
#92682 = ORIENTED_EDGE ( 'NONE', *, *, #40588, .F. ) ;
#92681 = DIRECTION ( 'NONE',  ( -0.000000000000000000, -1.000000000000000000, -0.000000000000000000 ) ) ;
#92683 = CONICAL_SURFACE ( 'NONE', #82322, 0.09999999999999982514, 0.003490658503988666988 ) ;
#92684 = AXIS2_PLACEMENT_3D ( 'NONE', #39674, #9549, #107079 ) ;
#92685 = EDGE_CURVE ( 'NONE', #26619, #8233, #50194, .T. ) ;
#92686 = EDGE_LOOP ( 'NONE', ( #122150, #56420, #62738, #38019 ) ) ;
#92687 = FACE_OUTER_BOUND ( 'NONE', #101112, .T. ) ;
#92688 = CIRCLE ( 'NONE', #109414, 0.06509327318403741736 ) ;
#92689 = AXIS2_PLACEMENT_3D ( 'NONE', #87487, #127442, #27940 ) ;
#92690 = EDGE_LOOP ( 'NONE', ( #118193, #58813 ) ) ;
#92691 = AXIS2_PLACEMENT_3D ( 'NONE', #81625, #41733, #39798 ) ;
#92692 = EDGE_LOOP ( 'NONE', ( #122269, #52231 ) ) ;
#92693 = DIRECTION ( 'NONE',  ( -0.000000000000000000, 1.000000000000000000, -0.000000000000000000 ) ) ;
#92694 = AXIS2_PLACEMENT_3D ( 'NONE', #15485, #65231, #55431 ) ;
#92695 = AXIS2_PLACEMENT_3D ( 'NONE', #84615, #63693, #15196 ) ;
#92696 = PLANE ( 'NONE',  #11234 ) ;
#92697 = CARTESIAN_POINT ( 'NONE',  ( 12.49999999999990230, 2.500000000000000000, -0.6928203230275541413 ) ) ;
#92698 = CARTESIAN_POINT ( 'NONE',  ( -9.600000000000006750, 2.500000000000000000, 0.6928203230275494784 ) ) ;
#92700 = EDGE_LOOP ( 'NONE', ( #66573, #110529, #79760, #25159 ) ) ;
#92699 = AXIS2_PLACEMENT_3D ( 'NONE', #9134, #127617, #118433 ) ;
#92701 = VECTOR ( 'NONE', #22024, 1000.000000000000000 ) ;
#92702 = AXIS2_PLACEMENT_3D ( 'NONE', #93170, #110847, #13288 ) ;
#92703 = FACE_OUTER_BOUND ( 'NONE', #83447, .T. ) ;
#92706 = VERTEX_POINT ( 'NONE', #30557 ) ;
#92705 = VECTOR ( 'NONE', #85533, 1000.000000000000000 ) ;
#92704 = DIRECTION ( 'NONE',  ( 0.000000000000000000, 1.000000000000000000, 0.000000000000000000 ) ) ;
#92707 = AXIS2_PLACEMENT_3D ( 'NONE', #103604, #15843, #36148 ) ;
#92708 = DIRECTION ( 'NONE',  ( 0.000000000000000000, 0.000000000000000000, -1.000000000000000000 ) ) ;
#92709 = CARTESIAN_POINT ( 'NONE',  ( 17.45652598566549685, -2.453228361101941424, 4.494719241542497912 ) ) ;
#92710 = CIRCLE ( 'NONE', #81942, 0.1000000000000002554 ) ;
#92711 = ORIENTED_EDGE ( 'NONE', *, *, #50638, .T. ) ;
#92712 = ADVANCED_FACE ( 'NONE', ( #29260 ), #69361, .T. ) ;
#92713 = ORIENTED_EDGE ( 'NONE', *, *, #79725, .T. ) ;
#92714 = EDGE_LOOP ( 'NONE', ( #57158, #46248 ) ) ;
#92715 = ORIENTED_EDGE ( 'NONE', *, *, #97151, .T. ) ;
#92716 = CARTESIAN_POINT ( 'NONE',  ( 12.04999999999990479, 12.50000000000000000, -6.495190528383302464 ) ) ;
#92717 = CARTESIAN_POINT ( 'NONE',  ( 15.50668943717079351, 1.500000000000191847, 6.997696160023704870 ) ) ;
#92718 = DIRECTION ( 'NONE',  ( 0.000000000000000000, -0.9999939076577903929, 0.003490651415223739937 ) ) ;
#92719 = ADVANCED_FACE ( 'NONE', ( #111678 ), #79010, .T. ) ;
#92720 = FACE_BOUND ( 'NONE', #33935, .T. ) ;
#92721 = EDGE_LOOP ( 'NONE', ( #18398, #35557, #35794, #102212 ) ) ;
#92722 = CARTESIAN_POINT ( 'NONE',  ( 184.1145833340161175, 6.668395609140177704, -3.849999999999998312 ) ) ;
#92723 = EDGE_CURVE ( 'NONE', #104908, #63527, #109055, .T. ) ;
#92724 = DIRECTION ( 'NONE',  ( 0.000000000000000000, 0.000000000000000000, -1.000000000000000000 ) ) ;
#92725 = DIRECTION ( 'NONE',  ( -0.000000000000000000, 1.000000000000000000, -0.000000000000000000 ) ) ;
#92726 = AXIS2_PLACEMENT_3D ( 'NONE', #94972, #115211, #106074 ) ;
#92727 = ADVANCED_FACE ( 'NONE', ( #9602 ), #49545, .T. ) ;
#92728 = DIRECTION ( 'NONE',  ( -0.000000000000000000, -0.000000000000000000, -1.000000000000000000 ) ) ;
#92729 = EDGE_CURVE ( 'NONE', #63286, #89688, #53403, .T. ) ;
#92730 = CARTESIAN_POINT ( 'NONE',  ( -8.150000000000012790, 2.500000000000000000, 2.611473670974873151 ) ) ;
#92731 = ADVANCED_FACE ( 'NONE', ( #23944 ), #4267, .T. ) ;
#92732 = CARTESIAN_POINT ( 'NONE',  ( 1.899999999999951283, 2.500000000000000000, 0.2464101615137736789 ) ) ;
#92733 = CIRCLE ( 'NONE', #78055, 0.09999999999999982514 ) ;
#92734 = AXIS2_PLACEMENT_3D ( 'NONE', #64870, #33510, #23673 ) ;
#92735 = VECTOR ( 'NONE', #2059, 1000.000000000000000 ) ;
#92736 = DIRECTION ( 'NONE',  ( -0.000000000000000000, -1.000000000000000000, -0.000000000000000000 ) ) ;
#92737 = ADVANCED_FACE ( 'NONE', ( #13459 ), #88212, .T. ) ;
#92738 = ORIENTED_EDGE ( 'NONE', *, *, #85283, .T. ) ;
#92739 = VERTEX_POINT ( 'NONE', #74325 ) ;
#92740 = VERTEX_POINT ( 'NONE', #84785 ) ;
#92741 = ORIENTED_EDGE ( 'NONE', *, *, #64943, .F. ) ;
#92742 = ORIENTED_EDGE ( 'NONE', *, *, #1864, .T. ) ;
#92743 = CARTESIAN_POINT ( 'NONE',  ( 6.049999999999932321, 12.50000000000000000, 1.818653347947321475 ) ) ;
#92744 = LINE ( 'NONE', #24000, #107236 ) ;
#92745 = ORIENTED_EDGE ( 'NONE', *, *, #113422, .T. ) ;
#92746 = FACE_BOUND ( 'NONE', #21470, .T. ) ;
#92747 = AXIS2_PLACEMENT_3D ( 'NONE', #18821, #49598, #118959 ) ;
#92748 = CIRCLE ( 'NONE', #50785, 0.06509327318403745899 ) ;
#92749 = EDGE_CURVE ( 'NONE', #98360, #127025, #123729, .T. ) ;
#92750 = DIRECTION ( 'NONE',  ( 0.000000000000000000, -0.000000000000000000, 1.000000000000000000 ) ) ;
#92751 = VECTOR ( 'NONE', #91634, 1000.000000000000000 ) ;
#92752 = VECTOR ( 'NONE', #26200, 1000.000000000000000 ) ;
#92753 = EDGE_LOOP ( 'NONE', ( #15444, #56401, #76565, #67248 ) ) ;
#92754 = DIRECTION ( 'NONE',  ( 0.000000000000000000, 0.000000000000000000, -1.000000000000000000 ) ) ;
#92755 = PLANE ( 'NONE',  #5159 ) ;
#92756 = CYLINDRICAL_SURFACE ( 'NONE', #68414, 0.5000000000000000000 ) ;
#92757 = CONICAL_SURFACE ( 'NONE', #46792, 0.1000000000000000472, 0.003490658503988666988 ) ;
#92758 = ORIENTED_EDGE ( 'NONE', *, *, #64843, .F. ) ;
#92759 = DIRECTION ( 'NONE',  ( -0.000000000000000000, -1.000000000000000000, -0.000000000000000000 ) ) ;
#92760 = EDGE_LOOP ( 'NONE', ( #79564, #47263 ) ) ;
#92761 = CIRCLE ( 'NONE', #36346, 0.06509327318403745899 ) ;
#92762 = AXIS2_PLACEMENT_3D ( 'NONE', #101445, #51704, #72634 ) ;
#92763 = AXIS2_PLACEMENT_3D ( 'NONE', #93423, #44313, #84230 ) ;
#92764 = EDGE_LOOP ( 'NONE', ( #95332, #56465, #117401, #45563 ) ) ;
#92765 = VERTEX_POINT ( 'NONE', #73033 ) ;
#92766 = DIRECTION ( 'NONE',  ( 0.000000000000000000, -0.000000000000000000, 1.000000000000000000 ) ) ;
#92767 = PLANE ( 'NONE',  #108261 ) ;
#92769 = VECTOR ( 'NONE', #53316, 1000.000000000000000 ) ;
#92768 = CARTESIAN_POINT ( 'NONE',  ( -12.04999999999999538, 12.50000000000000000, 2.165063509461097713 ) ) ;
#92770 = ORIENTED_EDGE ( 'NONE', *, *, #71849, .T. ) ;
#92771 = CARTESIAN_POINT ( 'NONE',  ( 6.899999999999928413, 2.500000000000000000, -3.983716857408426293 ) ) ;
#92772 = AXIS2_PLACEMENT_3D ( 'NONE', #119281, #28989, #68247 ) ;
#92773 = DIRECTION ( 'NONE',  ( 0.000000000000000000, -0.9999939076577903929, 0.003490651415223739937 ) ) ;
#92774 = DIRECTION ( 'NONE',  ( 0.000000000000000000, 0.000000000000000000, -1.000000000000000000 ) ) ;
#92775 = CARTESIAN_POINT ( 'NONE',  ( 186.1979166673494603, 6.668395609140176816, 3.850000000000000977 ) ) ;
#92776 = VERTEX_POINT ( 'NONE', #44880 ) ;
#92777 = CARTESIAN_POINT ( 'NONE',  ( 3.099999999999945466, 12.50000000000000000, 0.3464101615137735735 ) ) ;
#92778 = ORIENTED_EDGE ( 'NONE', *, *, #67229, .F. ) ;
#92779 = PLANE ( 'NONE',  #86789 ) ;
#92780 = ORIENTED_EDGE ( 'NONE', *, *, #116340, .T. ) ;
#92781 = EDGE_CURVE ( 'NONE', #57508, #93739, #12801, .T. ) ;
#92782 = ORIENTED_EDGE ( 'NONE', *, *, #64792, .F. ) ;
#92783 = CARTESIAN_POINT ( 'NONE',  ( 187.5000000000000000, -1.500000000000000000, -6.000000000000000000 ) ) ;
#92784 = CARTESIAN_POINT ( 'NONE',  ( 2.899999999999945732, 2.500000000000000000, -4.330127018922201643 ) ) ;
#92785 = VECTOR ( 'NONE', #21481, 1000.000000000000000 ) ;
#92786 = CARTESIAN_POINT ( 'NONE',  ( 8.949999999999919353, 2.500000000000000000, -6.248780366869526759 ) ) ;
#92787 = CIRCLE ( 'NONE', #32160, 0.06509327318403745899 ) ;
#92788 = CARTESIAN_POINT ( 'NONE',  ( 14.34999999999989662, 12.50000000000000000, 2.511473670974873507 ) ) ;
#92789 = DIRECTION ( 'NONE',  ( -4.274815082592931898E-19, -0.9999939076577903929, -0.003490651415223739937 ) ) ;
#92790 = ORIENTED_EDGE ( 'NONE', *, *, #77364, .T. ) ;
#92791 = EDGE_LOOP ( 'NONE', ( #19720, #30704, #18487, #111026 ) ) ;
#92792 = EDGE_CURVE ( 'NONE', #15955, #28223, #12914, .T. ) ;
#92793 = DIRECTION ( 'NONE',  ( 1.000000000000000000, 0.000000000000000000, -0.000000000000000000 ) ) ;
#92794 = AXIS2_PLACEMENT_3D ( 'NONE', #90597, #112828, #23149 ) ;
#92795 = AXIS2_PLACEMENT_3D ( 'NONE', #110366, #61278, #101200 ) ;
#92796 = CIRCLE ( 'NONE', #23836, 0.06509327318403741736 ) ;
#92797 = LINE ( 'NONE', #113057, #24347 ) ;
#92798 = AXIS2_PLACEMENT_3D ( 'NONE', #83465, #65071, #18412 ) ;
#92800 = DIRECTION ( 'NONE',  ( 0.000000000000000000, 0.000000000000000000, -1.000000000000000000 ) ) ;
#92799 = AXIS2_PLACEMENT_3D ( 'NONE', #14566, #105548, #34245 ) ;
#92801 = VERTEX_POINT ( 'NONE', #42291 ) ;
#92802 = EDGE_LOOP ( 'NONE', ( #48398, #114639 ) ) ;
#92803 = FACE_OUTER_BOUND ( 'NONE', #87366, .T. ) ;
#92804 = EDGE_LOOP ( 'NONE', ( #85361, #63958 ) ) ;
#92805 = CARTESIAN_POINT ( 'NONE',  ( 0.3999999999999563904, 2.500000000000000000, 5.022947341949748790 ) ) ;
#92806 = CARTESIAN_POINT ( 'NONE',  ( -6.450000000000016165, 2.500000000000000000, 2.511473670974873507 ) ) ;
#92807 = CIRCLE ( 'NONE', #21800, 0.1000000000000002554 ) ;
#92808 = AXIS2_PLACEMENT_3D ( 'NONE', #54459, #45306, #85209 ) ;
#92809 = AXIS2_PLACEMENT_3D ( 'NONE', #9984, #99008, #68897 ) ;
#92810 = DIRECTION ( 'NONE',  ( 0.000000000000000000, -0.9999939076577903929, 0.003490651415223739937 ) ) ;
#92811 = EDGE_LOOP ( 'NONE', ( #17236, #67457 ) ) ;
#92812 = CARTESIAN_POINT ( 'NONE',  ( -9.800000000000007816, 2.500000000000000000, -3.983716857408421852 ) ) ;
#92813 = CARTESIAN_POINT ( 'NONE',  ( -5.650000000000019895, 2.500000000000000000, 6.841600689897072485 ) ) ;
#92814 = DIRECTION ( 'NONE',  ( 0.000000000000000000, 1.000000000000000000, 0.000000000000000000 ) ) ;
#92815 = LINE ( 'NONE', #73165, #42625 ) ;
#92816 = AXIS2_PLACEMENT_3D ( 'NONE', #33425, #24877, #43889 ) ;
#92817 = CARTESIAN_POINT ( 'NONE',  ( -11.64999999999999680, 2.500000000000000000, -7.188010851410850499 ) ) ;
#92818 = VERTEX_POINT ( 'NONE', #124063 ) ;
#92819 = CARTESIAN_POINT ( 'NONE',  ( 6.649999999999928413, 12.50000000000000000, 2.922977105672686982 ) ) ;
#92820 = DIRECTION ( 'NONE',  ( 0.000000000000000000, 0.000000000000000000, 1.000000000000000000 ) ) ;
#92821 = ORIENTED_EDGE ( 'NONE', *, *, #79692, .T. ) ;
#92822 = VERTEX_POINT ( 'NONE', #103785 ) ;
#92823 = CARTESIAN_POINT ( 'NONE',  ( 184.5677083336747444, -4.367472073101514418, -7.564683531250002702 ) ) ;
#92824 = DIRECTION ( 'NONE',  ( -4.274815082592931898E-19, -0.9999939076577903929, -0.003490651415223739937 ) ) ;
#92825 = CARTESIAN_POINT ( 'NONE',  ( 13.34999999999989662, 2.500000000000000000, -2.165063509461101710 ) ) ;
#92826 = CONICAL_SURFACE ( 'NONE', #36396, 0.1000000000000002554, 0.003490658503988666988 ) ;
#92827 = CARTESIAN_POINT ( 'NONE',  ( -5.650000000000019895, 2.500000000000000000, 6.841600689897072485 ) ) ;
#92828 = DIRECTION ( 'NONE',  ( 0.000000000000000000, 1.000000000000000000, 0.000000000000000000 ) ) ;
#92829 = EDGE_CURVE ( 'NONE', #9926, #110798, #56821, .T. ) ;
#92830 = DIRECTION ( 'NONE',  ( 0.000000000000000000, 0.000000000000000000, 1.000000000000000000 ) ) ;
#92831 = DIRECTION ( 'NONE',  ( 0.000000000000000000, 0.000000000000000000, 1.000000000000000000 ) ) ;
#92832 = DIRECTION ( 'NONE',  ( 1.000000000000000000, 0.000000000000000000, 0.000000000000000000 ) ) ;
#92833 = DIRECTION ( 'NONE',  ( 0.000000000000000000, 0.000000000000000000, 1.000000000000000000 ) ) ;
#92834 = CARTESIAN_POINT ( 'NONE',  ( 12.49999999999990052, 2.500000000000000000, 0.6928203230275494784 ) ) ;
#92835 = EDGE_CURVE ( 'NONE', #15358, #56070, #124712, .T. ) ;
#92836 = EDGE_LOOP ( 'NONE', ( #88384, #35759, #23630, #62519 ) ) ;
#92837 = CIRCLE ( 'NONE', #38462, 0.06509327318403745899 ) ;
#92838 = EDGE_LOOP ( 'NONE', ( #103405, #102519, #28812, #4007 ) ) ;
#92839 = EDGE_LOOP ( 'NONE', ( #71536, #34853 ) ) ;
#92840 = EDGE_CURVE ( 'NONE', #56576, #51026, #19178, .T. ) ;
#92841 = ORIENTED_EDGE ( 'NONE', *, *, #29625, .T. ) ;
#92842 = AXIS2_PLACEMENT_3D ( 'NONE', #73713, #11580, #10908 ) ;
#92843 = ADVANCED_FACE ( 'NONE', ( #33752 ), #35062, .T. ) ;
#92844 = DIRECTION ( 'NONE',  ( 0.000000000000000000, -0.000000000000000000, 1.000000000000000000 ) ) ;
#92845 = FACE_BOUND ( 'NONE', #11683, .T. ) ;
#92846 = CIRCLE ( 'NONE', #36417, 0.09999999999999982514 ) ;
#92847 = VERTEX_POINT ( 'NONE', #32494 ) ;
#92848 = CARTESIAN_POINT ( 'NONE',  ( -5.600000000000023626, 2.500000000000000000, -4.676537180435977881 ) ) ;
#92849 = EDGE_CURVE ( 'NONE', #56575, #57519, #54663, .T. ) ;
#92850 = DIRECTION ( 'NONE',  ( 0.000000000000000000, 0.000000000000000000, 1.000000000000000000 ) ) ;
#92852 = ORIENTED_EDGE ( 'NONE', *, *, #44811, .T. ) ;
#92851 = CARTESIAN_POINT ( 'NONE',  ( 185.2500000000000000, 9.429780353434619030E-16, -7.700000000000000178 ) ) ;
#92853 = EDGE_CURVE ( 'NONE', #114323, #103313, #46371, .T. ) ;
#92854 = CARTESIAN_POINT ( 'NONE',  ( 5.849999999999933920, 12.50000000000000000, -2.792790559304616504 ) ) ;
#92855 = PLANE ( 'NONE',  #79307 ) ;
#92856 = VERTEX_POINT ( 'NONE', #114245 ) ;
#92857 = AXIS2_PLACEMENT_3D ( 'NONE', #9966, #93045, #112037 ) ;
#92858 = AXIS2_PLACEMENT_3D ( 'NONE', #42543, #121080, #71319 ) ;
#92859 = CONICAL_SURFACE ( 'NONE', #122103, 0.09999999999999982514, 0.003490658503988666988 ) ;
#92860 = ORIENTED_EDGE ( 'NONE', *, *, #97344, .T. ) ;
#92861 = ORIENTED_EDGE ( 'NONE', *, *, #105700, .T. ) ;
#92862 = VERTEX_POINT ( 'NONE', #114879 ) ;
#92863 = DIRECTION ( 'NONE',  ( -0.000000000000000000, -1.000000000000000000, -0.000000000000000000 ) ) ;
#92864 = VECTOR ( 'NONE', #106899, 1000.000000000000000 ) ;
#92865 = CARTESIAN_POINT ( 'NONE',  ( 8.299999999999922551, 2.500000000000000000, -4.430127018922202176 ) ) ;
#92866 = DIRECTION ( 'NONE',  ( 0.000000000000000000, 1.000000000000000000, 0.000000000000000000 ) ) ;
#92867 = CIRCLE ( 'NONE', #36441, 0.09999999999999999167 ) ;
#92868 = DIRECTION ( 'NONE',  ( 0.000000000000000000, 1.000000000000000000, 0.000000000000000000 ) ) ;
#92869 = VERTEX_POINT ( 'NONE', #65126 ) ;
#92870 = PLANE ( 'NONE',  #58569 ) ;
#92871 = EDGE_LOOP ( 'NONE', ( #111214, #23951, #101091, #49701 ) ) ;
#92872 = CARTESIAN_POINT ( 'NONE',  ( 108.0000000000000142, 8.500000000000000000, 0.2500000000000000000 ) ) ;
#92873 = DIRECTION ( 'NONE',  ( -0.000000000000000000, -1.000000000000000000, -0.000000000000000000 ) ) ;
#92874 = CARTESIAN_POINT ( 'NONE',  ( -9.800000000000004263, 12.50000000000000000, 3.983716857408420076 ) ) ;
#92875 = CARTESIAN_POINT ( 'NONE',  ( -2.100000000000033396, 12.50000000000000000, -0.6928203230275542523 ) ) ;
#92876 = ORIENTED_EDGE ( 'NONE', *, *, #119772, .T. ) ;
#92877 = VECTOR ( 'NONE', #69449, 1000.000000000000000 ) ;
#92878 = ORIENTED_EDGE ( 'NONE', *, *, #23124, .F. ) ;
#92879 = CONICAL_SURFACE ( 'NONE', #30191, 0.09999999999999982514, 0.003490658503988666988 ) ;
#92880 = ORIENTED_EDGE ( 'NONE', *, *, #94273, .F. ) ;
#92881 = CARTESIAN_POINT ( 'NONE',  ( -0.8500000000000386136, 2.500000000000000000, 5.802370205355744659 ) ) ;
#92883 = CONICAL_SURFACE ( 'NONE', #86593, 0.09999999999999982514, 0.003490658503988666988 ) ;
#92882 = CARTESIAN_POINT ( 'NONE',  ( -11.05000000000000071, 2.500000000000000000, 2.611473670974873151 ) ) ;
#92884 = VECTOR ( 'NONE', #62021, 1000.000000000000000 ) ;
#92885 = CARTESIAN_POINT ( 'NONE',  ( -11.24999999999996270, 2.500000000000000000, 6.495190528383297135 ) ) ;
#92886 = FACE_BOUND ( 'NONE', #26680, .T. ) ;
#92887 = DIRECTION ( 'NONE',  ( -0.000000000000000000, 1.000000000000000000, -0.000000000000000000 ) ) ;
#92888 = DIRECTION ( 'NONE',  ( 0.000000000000000000, -0.9999939076577903929, 0.003490651415223739937 ) ) ;
#92889 = EDGE_CURVE ( 'NONE', #129244, #60586, #84027, .T. ) ;
#92890 = DIRECTION ( 'NONE',  ( 0.000000000000000000, 0.000000000000000000, -1.000000000000000000 ) ) ;
#92891 = AXIS2_PLACEMENT_3D ( 'NONE', #99632, #62132, #79979 ) ;
#92892 = AXIS2_PLACEMENT_3D ( 'NONE', #46010, #124568, #115352 ) ;
#92893 = ADVANCED_FACE ( 'NONE', ( #12162 ), #42965, .T. ) ;
#92894 = EDGE_CURVE ( 'NONE', #115059, #85204, #82867, .T. ) ;
#92895 = CARTESIAN_POINT ( 'NONE',  ( 186.5052083336747444, -6.551208109652278289, 3.782341765624995134 ) ) ;
#92896 = CARTESIAN_POINT ( 'NONE',  ( 184.0000000000000000, 0.000000000000000000, 7.700000000000000178 ) ) ;
#92897 = EDGE_CURVE ( 'NONE', #71057, #102543, #5562, .T. ) ;
#92898 = CARTESIAN_POINT ( 'NONE',  ( 14.99999999999992895, 2.500000000000000000, -2.276824562219559311E-15 ) ) ;
#92899 = ORIENTED_EDGE ( 'NONE', *, *, #119486, .T. ) ;
#92900 = ADVANCED_FACE ( 'NONE', ( #17301 ), #31912, .T. ) ;
#92901 = VECTOR ( 'NONE', #127464, 1000.000000000000000 ) ;
#92902 = AXIS2_PLACEMENT_3D ( 'NONE', #37906, #19559, #59517 ) ;
#92903 = AXIS2_PLACEMENT_3D ( 'NONE', #39325, #118484, #28839 ) ;
#92904 = DIRECTION ( 'NONE',  ( 0.000000000000000000, -0.000000000000000000, 1.000000000000000000 ) ) ;
#92905 = EDGE_CURVE ( 'NONE', #123229, #126098, #29755, .T. ) ;
#92906 = ORIENTED_EDGE ( 'NONE', *, *, #101700, .F. ) ;
#92907 = VERTEX_POINT ( 'NONE', #56595 ) ;
#92908 = AXIS2_PLACEMENT_3D ( 'NONE', #70602, #81074, #20856 ) ;
#92909 = CARTESIAN_POINT ( 'NONE',  ( -3.750000000000029310, 2.500000000000000000, -7.188010851410854052 ) ) ;
#92910 = FACE_OUTER_BOUND ( 'NONE', #69823, .T. ) ;
#92911 = FACE_BOUND ( 'NONE', #10730, .T. ) ;
#92912 = CARTESIAN_POINT ( 'NONE',  ( -5.800000000000018474, 2.500000000000000000, -2.276824562219559311E-15 ) ) ;
#92913 = ADVANCED_FACE ( 'NONE', ( #57266 ), #59100, .T. ) ;
#92914 = EDGE_CURVE ( 'NONE', #79722, #65565, #77860, .T. ) ;
#92915 = VERTEX_POINT ( 'NONE', #97186 ) ;
#92916 = CARTESIAN_POINT ( 'NONE',  ( 81.97620568553573150, 3.937821662797851729, 6.124242991678374715 ) ) ;
#92917 = DIRECTION ( 'NONE',  ( 0.000000000000000000, 0.000000000000000000, 1.000000000000000000 ) ) ;
#92919 = VERTEX_POINT ( 'NONE', #67713 ) ;
#92918 = AXIS2_PLACEMENT_3D ( 'NONE', #53864, #13920, #55793 ) ;
#92920 = DIRECTION ( 'NONE',  ( 0.000000000000000000, -0.9999939076577903929, 0.003490651415223739937 ) ) ;
#92921 = CARTESIAN_POINT ( 'NONE',  ( -7.900000000000014566, 12.50000000000000000, -4.330127018922201643 ) ) ;
#92922 = ORIENTED_EDGE ( 'NONE', *, *, #42957, .T. ) ;
#92923 = CARTESIAN_POINT ( 'NONE',  ( -8.749999999999976907, 12.50000000000000000, -6.430097255199259010 ) ) ;
#92924 = DIRECTION ( 'NONE',  ( -0.000000000000000000, -1.000000000000000000, -0.000000000000000000 ) ) ;
#92925 = CIRCLE ( 'NONE', #84602, 0.06509327318403745899 ) ;
#92926 = CIRCLE ( 'NONE', #40711, 0.09999999999999982514 ) ;
#92927 = ORIENTED_EDGE ( 'NONE', *, *, #127694, .T. ) ;
#92928 = DIRECTION ( 'NONE',  ( 0.000000000000000000, 0.000000000000000000, 1.000000000000000000 ) ) ;
#92929 = CARTESIAN_POINT ( 'NONE',  ( 1.699999999999951994, 2.500000000000000000, -2.276824562219559311E-15 ) ) ;
#92930 = DIRECTION ( 'NONE',  ( 0.000000000000000000, 0.000000000000000000, 1.000000000000000000 ) ) ;
#92931 = ORIENTED_EDGE ( 'NONE', *, *, #120436, .T. ) ;
#92932 = EDGE_LOOP ( 'NONE', ( #97419, #25790 ) ) ;
#92933 = CARTESIAN_POINT ( 'NONE',  ( 9.799999999999917222, 12.50000000000000000, 0.2813168883297361700 ) ) ;
#92934 = VERTEX_POINT ( 'NONE', #16663 ) ;
#92935 = CARTESIAN_POINT ( 'NONE',  ( 4.599999999999938360, 12.50000000000000000, -0.6928203230275541413 ) ) ;
#92936 = DIRECTION ( 'NONE',  ( -0.000000000000000000, 1.000000000000000000, -0.000000000000000000 ) ) ;
#92937 = CIRCLE ( 'NONE', #69947, 0.1000000000000002554 ) ;
#92938 = ORIENTED_EDGE ( 'NONE', *, *, #85379, .T. ) ;
#92940 = DIRECTION ( 'NONE',  ( 0.000000000000000000, -0.000000000000000000, 1.000000000000000000 ) ) ;
#92939 = AXIS2_PLACEMENT_3D ( 'NONE', #55701, #54411, #85801 ) ;
#92941 = DIRECTION ( 'NONE',  ( 0.000000000000000000, -0.000000000000000000, 1.000000000000000000 ) ) ;
#92942 = DIRECTION ( 'NONE',  ( -0.000000000000000000, -1.000000000000000000, -0.000000000000000000 ) ) ;
#92943 = FACE_OUTER_BOUND ( 'NONE', #72219, .T. ) ;
#92944 = CARTESIAN_POINT ( 'NONE',  ( 6.699999999999930012, 12.50000000000000000, -4.395220292106239768 ) ) ;
#92945 = ORIENTED_EDGE ( 'NONE', *, *, #34924, .F. ) ;
#92946 = ADVANCED_FACE ( 'NONE', ( #45522 ), #88315, .T. ) ;
#92947 = ORIENTED_EDGE ( 'NONE', *, *, #862, .F. ) ;
#92948 = DIRECTION ( 'NONE',  ( -0.000000000000000000, -1.000000000000000000, -0.000000000000000000 ) ) ;
#92950 = VERTEX_POINT ( 'NONE', #87347 ) ;
#92949 = CONICAL_SURFACE ( 'NONE', #36518, 0.1000000000000000472, 0.003490658503988666988 ) ;
#92951 = AXIS2_PLACEMENT_3D ( 'NONE', #46875, #125425, #35758 ) ;
#92952 = CARTESIAN_POINT ( 'NONE',  ( -8.550000000000013145, 12.50000000000000000, 2.511473670974873507 ) ) ;
#92954 = EDGE_LOOP ( 'NONE', ( #68826, #113588 ) ) ;
#92953 = EDGE_LOOP ( 'NONE', ( #21319, #128799 ) ) ;
#92955 = VERTEX_POINT ( 'NONE', #47447 ) ;
#92956 = CIRCLE ( 'NONE', #67803, 0.06509327318403741736 ) ;
#92957 = PLANE ( 'NONE',  #114796 ) ;
#92958 = CIRCLE ( 'NONE', #65744, 0.06509327318403745899 ) ;
#92959 = FACE_OUTER_BOUND ( 'NONE', #108557, .T. ) ;
#92960 = FACE_OUTER_BOUND ( 'NONE', #76589, .T. ) ;
#92961 =( LENGTH_UNIT ( ) NAMED_UNIT ( * ) SI_UNIT ( .MILLI., .METRE. ) );
#92962 = DIRECTION ( 'NONE',  ( 0.000000000000000000, 0.000000000000000000, 1.000000000000000000 ) ) ;
#92963 = DIRECTION ( 'NONE',  ( -0.000000000000000000, 1.000000000000000000, -0.000000000000000000 ) ) ;
#92964 = CARTESIAN_POINT ( 'NONE',  ( -4.550000000000022915, 2.500000000000000000, 2.165063509461097713 ) ) ;
#92965 = CARTESIAN_POINT ( 'NONE',  ( 4.399999999999937295, 12.50000000000000000, 3.983716857408420964 ) ) ;
#92966 = DIRECTION ( 'NONE',  ( 0.000000000000000000, 0.000000000000000000, 1.000000000000000000 ) ) ;
#92967 = DIRECTION ( 'NONE',  ( 0.000000000000000000, -0.000000000000000000, 1.000000000000000000 ) ) ;
#92968 = ORIENTED_EDGE ( 'NONE', *, *, #95830, .F. ) ;
#92969 = AXIS2_PLACEMENT_3D ( 'NONE', #120196, #99272, #60641 ) ;
#92970 = DIRECTION ( 'NONE',  ( 0.000000000000000000, 1.000000000000000000, 0.000000000000000000 ) ) ;
#92971 = CIRCLE ( 'NONE', #3083, 0.06509327318403745899 ) ;
#92972 = CIRCLE ( 'NONE', #61671, 0.06509327318403745899 ) ;
#92973 = ORIENTED_EDGE ( 'NONE', *, *, #4742, .T. ) ;
#92974 = ORIENTED_EDGE ( 'NONE', *, *, #102084, .T. ) ;
#92975 = CARTESIAN_POINT ( 'NONE',  ( 5.849999999999931255, 12.50000000000000000, 2.792790559304612064 ) ) ;
#92976 = CARTESIAN_POINT ( 'NONE',  ( 0.5999999999999612310, 2.500000000000000000, -0.3464101615137760715 ) ) ;
#92977 = LINE ( 'NONE', #100832, #79988 ) ;
#92978 = AXIS2_PLACEMENT_3D ( 'NONE', #34543, #53524, #33866 ) ;
#92979 = DIRECTION ( 'NONE',  ( 0.000000000000000000, 1.000000000000000000, 0.000000000000000000 ) ) ;
#92981 = CARTESIAN_POINT ( 'NONE',  ( 5.649999999999934630, 12.50000000000000000, -2.511473670974877948 ) ) ;
#92980 = AXIS2_PLACEMENT_3D ( 'NONE', #129218, #37597, #59836 ) ;
#92982 = FACE_OUTER_BOUND ( 'NONE', #74969, .T. ) ;
#92983 = PLANE ( 'NONE',  #122053 ) ;
#92984 = EDGE_LOOP ( 'NONE', ( #65519, #75468, #85548, #97303 ) ) ;
#92986 = ORIENTED_EDGE ( 'NONE', *, *, #91656, .F. ) ;
#92985 = VECTOR ( 'NONE', #10234, 1000.000000000000000 ) ;
#92988 = EDGE_CURVE ( 'NONE', #98668, #125752, #106987, .T. ) ;
#92987 = CIRCLE ( 'NONE', #126439, 0.06509327318403745899 ) ;
#92989 = ORIENTED_EDGE ( 'NONE', *, *, #121633, .F. ) ;
#92990 = VERTEX_POINT ( 'NONE', #127302 ) ;
#92991 = VECTOR ( 'NONE', #94742, 1000.000000000000000 ) ;
#92992 = EDGE_CURVE ( 'NONE', #66128, #16718, #96516, .T. ) ;
#92993 = ORIENTED_EDGE ( 'NONE', *, *, #38153, .F. ) ;
#92994 = EDGE_CURVE ( 'NONE', #67445, #3107, #8902, .T. ) ;
#92995 = FACE_OUTER_BOUND ( 'NONE', #23126, .T. ) ;
#92996 = CARTESIAN_POINT ( 'NONE',  ( -1.700000000000034817, 2.500000000000000000, -4.330127018922201643 ) ) ;
#92997 = LINE ( 'NONE', #73333, #79903 ) ;
#92998 = PLANE ( 'NONE',  #123881 ) ;
#92999 = EDGE_CURVE ( 'NONE', #62494, #10784, #27681, .T. ) ;
#93000 = DIRECTION ( 'NONE',  ( 0.000000000000000000, 0.000000000000000000, 1.000000000000000000 ) ) ;
#93002 = VERTEX_POINT ( 'NONE', #57919 ) ;
#93001 = ADVANCED_FACE ( 'NONE', ( #35696 ), #21434, .T. ) ;
#93003 = CARTESIAN_POINT ( 'NONE',  ( 65.39894239681107990, -3.129862336044758386, 5.811320851586441627 ) ) ;
#93004 = EDGE_CURVE ( 'NONE', #23771, #17021, #19364, .T. ) ;
#93005 = CARTESIAN_POINT ( 'NONE',  ( 11.64999999999990443, 12.50000000000000000, -7.188010851410854052 ) ) ;
#93006 = EDGE_CURVE ( 'NONE', #844, #101014, #61152, .T. ) ;
#93007 = CARTESIAN_POINT ( 'NONE',  ( 7.949999999999922018, 12.50000000000000000, -2.165063509461101710 ) ) ;
#93008 = AXIS2_PLACEMENT_3D ( 'NONE', #97091, #105630, #56513 ) ;
#93009 = DIRECTION ( 'NONE',  ( 0.000000000000000000, 0.000000000000000000, 1.000000000000000000 ) ) ;
#93010 = ORIENTED_EDGE ( 'NONE', *, *, #65966, .F. ) ;
#93011 = ORIENTED_EDGE ( 'NONE', *, *, #52512, .F. ) ;
#93012 = VERTEX_POINT ( 'NONE', #105053 ) ;
#93013 = CARTESIAN_POINT ( 'NONE',  ( 5.399999999999933742, 12.50000000000000000, -0.06509327318403980434 ) ) ;
#93014 = EDGE_CURVE ( 'NONE', #110490, #129134, #125354, .T. ) ;
#93015 = AXIS2_PLACEMENT_3D ( 'NONE', #3567, #81491, #83432 ) ;
#93016 = DIRECTION ( 'NONE',  ( 0.000000000000000000, 0.000000000000000000, -1.000000000000000000 ) ) ;
#93017 = DIRECTION ( 'NONE',  ( 0.000000000000000000, -0.9999939076577903929, 0.003490651415223739937 ) ) ;
#93018 = VERTEX_POINT ( 'NONE', #55960 ) ;
#93019 = CARTESIAN_POINT ( 'NONE',  ( -7.700000000000010836, 2.500000000000000000, 3.983716857408420964 ) ) ;
#93020 = DIRECTION ( 'NONE',  ( -0.000000000000000000, 1.000000000000000000, -0.000000000000000000 ) ) ;
#93021 = DIRECTION ( 'NONE',  ( 0.000000000000000000, 1.000000000000000000, 0.000000000000000000 ) ) ;
#93022 = LINE ( 'NONE', #60969, #70616 ) ;
#93023 = AXIS2_PLACEMENT_3D ( 'NONE', #55830, #17831, #78047 ) ;
#93024 = CARTESIAN_POINT ( 'NONE',  ( 4.149999999999941735, 2.500000000000000000, -7.288010851410854585 ) ) ;
#93025 = VERTEX_POINT ( 'NONE', #95898 ) ;
#93026 = ORIENTED_EDGE ( 'NONE', *, *, #10659, .T. ) ;
#93027 = ADVANCED_FACE ( 'NONE', ( #6204 ), #36356, .T. ) ;
#93028 = CARTESIAN_POINT ( 'NONE',  ( 165.4999999999999716, 0.000000000000000000, -2.000000000000000000 ) ) ;
#93029 = CARTESIAN_POINT ( 'NONE',  ( -9.150000000000005684, 12.50000000000000000, 5.867463478539781896 ) ) ;
#93030 = DIRECTION ( 'NONE',  ( -0.000000000000000000, 1.000000000000000000, -0.000000000000000000 ) ) ;
#93031 = DIRECTION ( 'NONE',  ( 0.000000000000000000, 0.000000000000000000, -1.000000000000000000 ) ) ;
#93032 = DIRECTION ( 'NONE',  ( -0.000000000000000000, 1.000000000000000000, -0.000000000000000000 ) ) ;
#93033 = ORIENTED_EDGE ( 'NONE', *, *, #30997, .T. ) ;
#93034 = VECTOR ( 'NONE', #986, 1000.000000000000000 ) ;
#93035 = EDGE_CURVE ( 'NONE', #49015, #70759, #102910, .T. ) ;
#93036 = ORIENTED_EDGE ( 'NONE', *, *, #124805, .F. ) ;
#93037 = EDGE_CURVE ( 'NONE', #120364, #18875, #92535, .T. ) ;
#93038 = LINE ( 'NONE', #64847, #83620 ) ;
#93039 = DIRECTION ( 'NONE',  ( 0.000000000000000000, 1.000000000000000000, 0.000000000000000000 ) ) ;
#93040 = CARTESIAN_POINT ( 'NONE',  ( -1.450000000000035483, 12.50000000000000000, 6.148780366869520897 ) ) ;
#93041 = DIRECTION ( 'NONE',  ( 0.000000000000000000, 0.000000000000000000, 1.000000000000000000 ) ) ;
#93042 = ADVANCED_FACE ( 'NONE', ( #81425 ), #111298, .T. ) ;
#93043 = CARTESIAN_POINT ( 'NONE',  ( -6.450000000000019718, 2.500000000000000000, -6.148780366869526226 ) ) ;
#93044 = ORIENTED_EDGE ( 'NONE', *, *, #95095, .F. ) ;
#93045 = DIRECTION ( 'NONE',  ( -0.000000000000000000, 1.000000000000000000, -0.000000000000000000 ) ) ;
#93046 = EDGE_CURVE ( 'NONE', #16038, #102251, #40208, .T. ) ;
#93047 = DIRECTION ( 'NONE',  ( 0.000000000000000000, 0.000000000000000000, -1.000000000000000000 ) ) ;
#93048 = ORIENTED_EDGE ( 'NONE', *, *, #115979, .F. ) ;
#93049 = DIRECTION ( 'NONE',  ( -4.274815082592931898E-19, -0.9999939076577903929, -0.003490651415223739937 ) ) ;
#93050 = EDGE_CURVE ( 'NONE', #17558, #95927, #60505, .T. ) ;
#93051 = AXIS2_PLACEMENT_3D ( 'NONE', #35968, #24218, #105352 ) ;
#93052 = EDGE_LOOP ( 'NONE', ( #68478, #114986, #129269, #81704 ) ) ;
#93053 = CARTESIAN_POINT ( 'NONE',  ( -3.469446951953614189E-14, 2.500000000000000000, -0.5928203230275518321 ) ) ;
#93054 = ADVANCED_FACE ( 'NONE', ( #59871 ), #38165, .T. ) ;
#93055 = EDGE_CURVE ( 'NONE', #117313, #46303, #52736, .T. ) ;
#93056 = ADVANCED_FACE ( 'NONE', ( #50664 ), #88654, .T. ) ;
#93057 = AXIS2_PLACEMENT_3D ( 'NONE', #31115, #61856, #52034 ) ;
#93058 = EDGE_LOOP ( 'NONE', ( #82853, #15741, #47337, #9287 ) ) ;
#93059 = DIRECTION ( 'NONE',  ( 0.000000000000000000, 1.000000000000000000, 0.000000000000000000 ) ) ;
#93060 = DIRECTION ( 'NONE',  ( -0.000000000000000000, -1.000000000000000000, -0.000000000000000000 ) ) ;
#93061 = AXIS2_PLACEMENT_3D ( 'NONE', #8766, #20550, #244 ) ;
#93062 = CONICAL_SURFACE ( 'NONE', #61770, 0.09999999999999982514, 0.003490658503988666988 ) ;
#93063 = EDGE_LOOP ( 'NONE', ( #36689, #98498, #126950, #7092 ) ) ;
#93064 = ORIENTED_EDGE ( 'NONE', *, *, #95361, .F. ) ;
#93065 = CARTESIAN_POINT ( 'NONE',  ( 185.1302083336747160, -4.367472073101514418, -7.564683531250002702 ) ) ;
#93066 = DIRECTION ( 'NONE',  ( 0.000000000000000000, 1.000000000000000000, 0.000000000000000000 ) ) ;
#93067 = EDGE_CURVE ( 'NONE', #34614, #59330, #10943, .T. ) ;
#93068 = CARTESIAN_POINT ( 'NONE',  ( 186.5052083336747444, -6.551208109652278289, 3.782341765624995134 ) ) ;
#93069 = CARTESIAN_POINT ( 'NONE',  ( 185.5260416670080588, -6.551208109652273848, -3.782341765625003571 ) ) ;
#93070 = AXIS2_PLACEMENT_3D ( 'NONE', #32306, #51925, #11344 ) ;
#93071 = VECTOR ( 'NONE', #80385, 1000.000000000000000 ) ;
#93072 = AXIS2_PLACEMENT_3D ( 'NONE', #57728, #87161, #128415 ) ;
#93073 = DIRECTION ( 'NONE',  ( -0.000000000000000000, 1.000000000000000000, -0.000000000000000000 ) ) ;
#93074 = FACE_OUTER_BOUND ( 'NONE', #127313, .T. ) ;
#93075 = PLANE ( 'NONE',  #122528 ) ;
#93076 = DIRECTION ( 'NONE',  ( 0.000000000000000000, -0.9999939076577903929, 0.003490651415223739937 ) ) ;
#93077 = AXIS2_PLACEMENT_3D ( 'NONE', #64479, #93306, #35048 ) ;
#93078 = AXIS2_PLACEMENT_3D ( 'NONE', #96748, #61198, #126880 ) ;
#93079 = VERTEX_POINT ( 'NONE', #11377 ) ;
#93080 = VERTEX_POINT ( 'NONE', #128613 ) ;
#93081 = DIRECTION ( 'NONE',  ( 0.000000000000000000, -0.000000000000000000, 1.000000000000000000 ) ) ;
#93082 = ORIENTED_EDGE ( 'NONE', *, *, #122758, .F. ) ;
#93083 = DIRECTION ( 'NONE',  ( 0.000000000000000000, 0.000000000000000000, 1.000000000000000000 ) ) ;
#93084 = DIRECTION ( 'NONE',  ( 0.000000000000000000, 1.000000000000000000, 0.000000000000000000 ) ) ;
#93085 = CIRCLE ( 'NONE', #118104, 0.1000000000000002554 ) ;
#93086 = CARTESIAN_POINT ( 'NONE',  ( -1.450000000000035039, 12.50000000000000000, -6.906693963081115051 ) ) ;
#93088 = VERTEX_POINT ( 'NONE', #70310 ) ;
#93087 = EDGE_LOOP ( 'NONE', ( #294, #119735 ) ) ;
#93089 = FACE_BOUND ( 'NONE', #112690, .T. ) ;
#93090 = EDGE_LOOP ( 'NONE', ( #75125, #71530, #104844, #123515 ) ) ;
#93091 = CARTESIAN_POINT ( 'NONE',  ( -14.39999999999998614, 2.500000000000000000, -0.3464101615137760715 ) ) ;
#93092 = FACE_OUTER_BOUND ( 'NONE', #53831, .T. ) ;
#93093 = CARTESIAN_POINT ( 'NONE',  ( 3.549999999999943867, 2.500000000000000000, -6.148780366869526226 ) ) ;
#93094 = CARTESIAN_POINT ( 'NONE',  ( 4.149999999999938183, 2.500000000000000000, 5.802370205355744659 ) ) ;
#93095 = CARTESIAN_POINT ( 'NONE',  ( -2.900000000000029665, 2.500000000000000000, 3.637306695894644726 ) ) ;
#93096 = CARTESIAN_POINT ( 'NONE',  ( 2.049999999999948308, 2.500000000000000000, 6.495190528383297135 ) ) ;
#93097 = LINE ( 'NONE', #52505, #118775 ) ;
#93098 = LINE ( 'NONE', #5336, #9807 ) ;
#93099 = CARTESIAN_POINT ( 'NONE',  ( 129.5000000000000000, 1.500000000000000000, -6.000000000000000000 ) ) ;
#93100 = DIRECTION ( 'NONE',  ( -0.000000000000000000, 1.000000000000000000, -0.000000000000000000 ) ) ;
#93101 = CIRCLE ( 'NONE', #105711, 0.06509327318403745899 ) ;
#93102 = DIRECTION ( 'NONE',  ( 0.000000000000000000, 0.000000000000000000, -1.000000000000000000 ) ) ;
#93103 = VERTEX_POINT ( 'NONE', #31051 ) ;
#93104 = EDGE_LOOP ( 'NONE', ( #9928, #72291 ) ) ;
#93105 = ADVANCED_FACE ( 'NONE', ( #119389 ), #128053, .T. ) ;
#93106 = VERTEX_POINT ( 'NONE', #10095 ) ;
#93107 = CARTESIAN_POINT ( 'NONE',  ( -7.700000000000016165, 2.500000000000000000, 0.3464101615137735735 ) ) ;
#93108 = ORIENTED_EDGE ( 'NONE', *, *, #121071, .T. ) ;
#93109 = DIRECTION ( 'NONE',  ( -0.000000000000000000, -1.000000000000000000, -0.000000000000000000 ) ) ;
#93111 = ORIENTED_EDGE ( 'NONE', *, *, #96213, .T. ) ;
#93110 = VERTEX_POINT ( 'NONE', #38945 ) ;
#93112 = CONICAL_SURFACE ( 'NONE', #101512, 0.1000000000000000056, 0.003490658503988666988 ) ;
#93113 = ORIENTED_EDGE ( 'NONE', *, *, #15863, .T. ) ;
#93114 = CARTESIAN_POINT ( 'NONE',  ( 7.899999999999921307, 2.500000000000000000, -2.385244779468109755E-15 ) ) ;
#93115 = AXIS2_PLACEMENT_3D ( 'NONE', #17220, #128531, #69570 ) ;
#93116 = DIRECTION ( 'NONE',  ( -0.000000000000000000, 1.000000000000000000, -0.000000000000000000 ) ) ;
#93117 = CARTESIAN_POINT ( 'NONE',  ( -0.8500000000000390576, 2.500000000000000000, -2.265063509461101798 ) ) ;
#93118 = CARTESIAN_POINT ( 'NONE',  ( 26.76176526821260282, -1.073658814954678631, -4.445806700280396484 ) ) ;
#93119 = LINE ( 'NONE', #101646, #93643 ) ;
#93120 = CARTESIAN_POINT ( 'NONE',  ( 4.349999999999940137, 12.50000000000000000, -2.446380397790840266 ) ) ;
#93121 = ADVANCED_FACE ( 'NONE', ( #110856 ), #50049, .T. ) ;
#93122 = ORIENTED_EDGE ( 'NONE', *, *, #129499, .T. ) ;
#93123 = DIRECTION ( 'NONE',  ( -0.000000000000000000, 1.000000000000000000, -0.000000000000000000 ) ) ;
#93124 = ORIENTED_EDGE ( 'NONE', *, *, #36321, .T. ) ;
#93125 = AXIS2_PLACEMENT_3D ( 'NONE', #23002, #93030, #74029 ) ;
#93126 = ORIENTED_EDGE ( 'NONE', *, *, #29329, .F. ) ;
#93127 = ORIENTED_EDGE ( 'NONE', *, *, #85616, .F. ) ;
#93128 = VECTOR ( 'NONE', #126881, 1000.000000000000000 ) ;
#93129 = DIRECTION ( 'NONE',  ( 0.000000000000000000, -0.000000000000000000, 1.000000000000000000 ) ) ;
#93130 = ORIENTED_EDGE ( 'NONE', *, *, #80871, .F. ) ;
#93131 = ORIENTED_EDGE ( 'NONE', *, *, #120396, .T. ) ;
#93132 = EDGE_LOOP ( 'NONE', ( #93991, #34712, #39591, #38063 ) ) ;
#93133 = FACE_OUTER_BOUND ( 'NONE', #63920, .T. ) ;
#93135 = AXIS2_PLACEMENT_3D ( 'NONE', #76153, #116706, #54555 ) ;
#93134 = DIRECTION ( 'NONE',  ( 0.000000000000000000, 1.000000000000000000, 0.000000000000000000 ) ) ;
#93136 = CARTESIAN_POINT ( 'NONE',  ( 10.84999999999991260, 12.50000000000000000, -1.472243186433550122 ) ) ;
#93137 = DIRECTION ( 'NONE',  ( 0.000000000000000000, -0.9999939076577903929, 0.003490651415223739937 ) ) ;
#93138 = DIRECTION ( 'NONE',  ( -0.000000000000000000, -1.000000000000000000, -0.000000000000000000 ) ) ;
#93139 = DIRECTION ( 'NONE',  ( 0.000000000000000000, 0.000000000000000000, -1.000000000000000000 ) ) ;
#93140 = FACE_OUTER_BOUND ( 'NONE', #41418, .T. ) ;
#93141 = VERTEX_POINT ( 'NONE', #69005 ) ;
#93142 = DIRECTION ( 'NONE',  ( -0.000000000000000000, -1.000000000000000000, -0.000000000000000000 ) ) ;
#93143 = EDGE_CURVE ( 'NONE', #33550, #38354, #100843, .T. ) ;
#93144 = ORIENTED_EDGE ( 'NONE', *, *, #115878, .F. ) ;
#93145 = DIRECTION ( 'NONE',  ( 0.000000000000000000, 1.000000000000000000, 0.000000000000000000 ) ) ;
#93146 = AXIS2_PLACEMENT_3D ( 'NONE', #81024, #20167, #49647 ) ;
#93147 = ORIENTED_EDGE ( 'NONE', *, *, #83808, .F. ) ;
#93148 = CIRCLE ( 'NONE', #13700, 0.09999999999999982514 ) ;
#93149 = EDGE_LOOP ( 'NONE', ( #7062, #65351 ) ) ;
#93150 = EDGE_CURVE ( 'NONE', #121438, #77033, #40224, .T. ) ;
#93151 = DIRECTION ( 'NONE',  ( 0.000000000000000000, -0.000000000000000000, 1.000000000000000000 ) ) ;
#93152 = FACE_OUTER_BOUND ( 'NONE', #82799, .T. ) ;
#93153 = CIRCLE ( 'NONE', #82695, 0.06509327318403745899 ) ;
#93155 = DIRECTION ( 'NONE',  ( -4.274815082592931898E-19, -0.9999939076577903929, -0.003490651415223739937 ) ) ;
#93154 = VECTOR ( 'NONE', #110844, 1000.000000000000000 ) ;
#93156 = ORIENTED_EDGE ( 'NONE', *, *, #45590, .F. ) ;
#93157 = ADVANCED_FACE ( 'NONE', ( #30407 ), #80785, .T. ) ;
#93159 = ORIENTED_EDGE ( 'NONE', *, *, #92729, .F. ) ;
#93158 = EDGE_CURVE ( 'NONE', #92121, #40225, #46468, .T. ) ;
#93160 = DIRECTION ( 'NONE',  ( -0.000000000000000000, 1.000000000000000000, -0.000000000000000000 ) ) ;
#93161 = DIRECTION ( 'NONE',  ( 0.000000000000000000, 0.000000000000000000, 1.000000000000000000 ) ) ;
#93162 = EDGE_CURVE ( 'NONE', #82670, #107304, #19251, .T. ) ;
#93163 = CARTESIAN_POINT ( 'NONE',  ( 2.099999999999950351, 12.50000000000000000, -4.395220292106239768 ) ) ;
#93164 = EDGE_CURVE ( 'NONE', #63587, #120581, #6732, .T. ) ;
#93165 = EDGE_CURVE ( 'NONE', #120897, #27524, #4761, .T. ) ;
#93166 = DIRECTION ( 'NONE',  ( 0.000000000000000000, -0.000000000000000000, 1.000000000000000000 ) ) ;
#93167 = CIRCLE ( 'NONE', #9530, 0.1000000000000002554 ) ;
#93168 = LINE ( 'NONE', #101689, #112758 ) ;
#93169 = ORIENTED_EDGE ( 'NONE', *, *, #104227, .F. ) ;
#93170 = CARTESIAN_POINT ( 'NONE',  ( -13.29999999999998828, 2.500000000000000000, 4.330127018922196314 ) ) ;
#93171 = EDGE_CURVE ( 'NONE', #114482, #85021, #44422, .T. ) ;
#93172 = ORIENTED_EDGE ( 'NONE', *, *, #95198, .F. ) ;
#93173 = EDGE_CURVE ( 'NONE', #1061, #37867, #61791, .T. ) ;
#93174 = CIRCLE ( 'NONE', #114089, 0.06509327318403745899 ) ;
#93175 = PLANE ( 'NONE',  #8916 ) ;
#93177 = AXIS2_PLACEMENT_3D ( 'NONE', #828, #28369, #118663 ) ;
#93176 = CARTESIAN_POINT ( 'NONE',  ( 10.19999999999991047, 12.50000000000000000, -3.918623584224389056 ) ) ;
#93178 = EDGE_CURVE ( 'NONE', #93002, #83416, #109357, .T. ) ;
#93179 = AXIS2_PLACEMENT_3D ( 'NONE', #42081, #40145, #40809 ) ;
#93180 = VECTOR ( 'NONE', #87174, 1000.000000000000000 ) ;
#93181 = CARTESIAN_POINT ( 'NONE',  ( 187.0416666666666288, -4.445597072760122614, 7.699999999999998401 ) ) ;
#93182 = FACE_OUTER_BOUND ( 'NONE', #123353, .T. ) ;
#93183 = DIRECTION ( 'NONE',  ( 0.000000000000000000, -0.000000000000000000, 1.000000000000000000 ) ) ;
#93184 = CARTESIAN_POINT ( 'NONE',  ( -3.950000000000025491, 2.500000000000000000, 6.148780366869520897 ) ) ;
#93185 = CARTESIAN_POINT ( 'NONE',  ( -6.450000000000014388, 2.500000000000000000, 6.148780366869520897 ) ) ;
#93186 = EDGE_LOOP ( 'NONE', ( #48273, #70895, #10957, #10478 ) ) ;
#93187 = DIRECTION ( 'NONE',  ( 0.000000000000000000, 0.000000000000000000, 1.000000000000000000 ) ) ;
#93188 = DIRECTION ( 'NONE',  ( -0.000000000000000000, -1.000000000000000000, -0.000000000000000000 ) ) ;
#93189 = DIRECTION ( 'NONE',  ( 0.000000000000000000, 0.000000000000000000, -1.000000000000000000 ) ) ;
#93190 = VERTEX_POINT ( 'NONE', #111510 ) ;
#93191 = CIRCLE ( 'NONE', #80667, 0.1000000000000002554 ) ;
#93192 = DIRECTION ( 'NONE',  ( -0.000000000000000000, 1.000000000000000000, -0.000000000000000000 ) ) ;
#93193 = EDGE_LOOP ( 'NONE', ( #106308, #30428, #28553, #84502 ) ) ;
#93194 = DIRECTION ( 'NONE',  ( 0.000000000000000000, 1.000000000000000000, 0.000000000000000000 ) ) ;
#93195 = AXIS2_PLACEMENT_3D ( 'NONE', #66815, #6585, #106746 ) ;
#93196 = ORIENTED_EDGE ( 'NONE', *, *, #119233, .F. ) ;
#93197 = CARTESIAN_POINT ( 'NONE',  ( 19.08853762628606532, -0.5565172523996277931, -4.470057054644892780 ) ) ;
#93198 = DIRECTION ( 'NONE',  ( -4.274815082592931898E-19, -0.9999939076577903929, -0.003490651415223739937 ) ) ;
#93199 = CARTESIAN_POINT ( 'NONE',  ( -14.39999999999998614, 2.500000000000000000, 0.2464101615137758439 ) ) ;
#93200 = CIRCLE ( 'NONE', #9572, 0.06509327318403745899 ) ;
#93201 = ORIENTED_EDGE ( 'NONE', *, *, #23119, .T. ) ;
#93202 = DIRECTION ( 'NONE',  ( 0.000000000000000000, 1.000000000000000000, 0.000000000000000000 ) ) ;
#93203 = CIRCLE ( 'NONE', #43139, 0.06509327318403745899 ) ;
#93204 = CARTESIAN_POINT ( 'NONE',  ( -11.64999999999999680, 2.500000000000000000, 2.757883832488649656 ) ) ;
#93205 = ADVANCED_FACE ( 'NONE', ( #33608 ), #36214, .T. ) ;
#93206 = EDGE_LOOP ( 'NONE', ( #41694, #87784 ) ) ;
#93207 = ADVANCED_FACE ( 'NONE', ( #112813 ), #29853, .T. ) ;
#93208 = ORIENTED_EDGE ( 'NONE', *, *, #12618, .T. ) ;
#93211 = EDGE_CURVE ( 'NONE', #109920, #5141, #54514, .T. ) ;
#93210 = CIRCLE ( 'NONE', #89099, 0.06509327318403745899 ) ;
#93209 = AXIS2_PLACEMENT_3D ( 'NONE', #45138, #77166, #35320 ) ;
#93212 = VERTEX_POINT ( 'NONE', #44722 ) ;
#93213 = DIRECTION ( 'NONE',  ( -0.000000000000000000, -1.000000000000000000, -0.000000000000000000 ) ) ;
#93214 = DIRECTION ( 'NONE',  ( 0.000000000000000000, 0.000000000000000000, 1.000000000000000000 ) ) ;
#93215 = CARTESIAN_POINT ( 'NONE',  ( 11.64999999999990266, 2.500000000000000000, 2.165063509461097713 ) ) ;
#93216 = ORIENTED_EDGE ( 'NONE', *, *, #106313, .F. ) ;
#93217 = DIRECTION ( 'NONE',  ( 0.000000000000000000, 0.000000000000000000, 1.000000000000000000 ) ) ;
#93218 = DIRECTION ( 'NONE',  ( 0.000000000000000000, -0.000000000000000000, 1.000000000000000000 ) ) ;
#93219 = ORIENTED_EDGE ( 'NONE', *, *, #24547, .F. ) ;
#93220 = ADVANCED_FACE ( 'NONE', ( #13949 ), #92634, .T. ) ;
#93221 = FACE_OUTER_BOUND ( 'NONE', #110034, .T. ) ;
#93223 = FACE_OUTER_BOUND ( 'NONE', #60522, .T. ) ;
#93222 = VECTOR ( 'NONE', #50539, 1000.000000000000000 ) ;
#93224 = DIRECTION ( 'NONE',  ( 0.000000000000000000, 1.000000000000000000, 0.000000000000000000 ) ) ;
#93225 = PLANE ( 'NONE',  #111981 ) ;
#93226 = DIRECTION ( 'NONE',  ( 0.000000000000000000, -0.9999939076577903929, 0.003490651415223739937 ) ) ;
#93227 = FACE_OUTER_BOUND ( 'NONE', #100116, .T. ) ;
#93228 = CARTESIAN_POINT ( 'NONE',  ( -5.850000000000021849, 12.50000000000000000, -7.253104124594891289 ) ) ;
#93229 = ORIENTED_EDGE ( 'NONE', *, *, #3193, .T. ) ;
#93230 = VERTEX_POINT ( 'NONE', #123906 ) ;
#93231 = ORIENTED_EDGE ( 'NONE', *, *, #62156, .F. ) ;
#93232 = EDGE_LOOP ( 'NONE', ( #59606, #53568, #81620, #50969 ) ) ;
#93233 = CARTESIAN_POINT ( 'NONE',  ( 48.81612456492386087, 3.619496399135581743, 4.312668942933988170 ) ) ;
#93234 = DIRECTION ( 'NONE',  ( -0.000000000000000000, 1.000000000000000000, -0.000000000000000000 ) ) ;
#93235 = DIRECTION ( 'NONE',  ( 0.000000000000000000, 0.000000000000000000, -1.000000000000000000 ) ) ;
#93236 = ORIENTED_EDGE ( 'NONE', *, *, #17664, .F. ) ;
#93237 = FACE_BOUND ( 'NONE', #98708, .T. ) ;
#93238 = ADVANCED_FACE ( 'NONE', ( #103639 ), #71592, .T. ) ;
#93239 = DIRECTION ( 'NONE',  ( 0.000000000000000000, 1.000000000000000000, 0.000000000000000000 ) ) ;
#93240 = DIRECTION ( 'NONE',  ( -0.000000000000000000, -1.000000000000000000, -0.000000000000000000 ) ) ;
#93241 = DIRECTION ( 'NONE',  ( -0.000000000000000000, 1.000000000000000000, -0.000000000000000000 ) ) ;
#93242 = CONICAL_SURFACE ( 'NONE', #89119, 0.1000000000000002554, 0.003490658503988666988 ) ;
#93243 = FACE_OUTER_BOUND ( 'NONE', #99418, .T. ) ;
#93244 = AXIS2_PLACEMENT_3D ( 'NONE', #12493, #91708, #52419 ) ;
#93245 = DIRECTION ( 'NONE',  ( 0.000000000000000000, 1.000000000000000000, 0.000000000000000000 ) ) ;
#93246 = CARTESIAN_POINT ( 'NONE',  ( -6.850000000000017408, 12.50000000000000000, -1.818653347947325916 ) ) ;
#93247 = DIRECTION ( 'NONE',  ( 0.000000000000000000, -0.9999939076577903929, 0.003490651415223739937 ) ) ;
#93248 = CARTESIAN_POINT ( 'NONE',  ( 3.949999999999941558, 2.500000000000000000, -6.148780366869526226 ) ) ;
#93249 = DIRECTION ( 'NONE',  ( 0.000000000000000000, 0.000000000000000000, 1.000000000000000000 ) ) ;
#93251 = ORIENTED_EDGE ( 'NONE', *, *, #12258, .F. ) ;
#93250 = CONICAL_SURFACE ( 'NONE', #7547, 0.09999999999999999167, 0.003490658503988666988 ) ;
#93252 = ORIENTED_EDGE ( 'NONE', *, *, #26216, .F. ) ;
#93253 = ORIENTED_EDGE ( 'NONE', *, *, #89737, .F. ) ;
#93254 = EDGE_CURVE ( 'NONE', #96534, #61265, #82173, .T. ) ;
#93255 = ORIENTED_EDGE ( 'NONE', *, *, #99926, .F. ) ;
#93256 = ORIENTED_EDGE ( 'NONE', *, *, #116510, .T. ) ;
#93257 = ORIENTED_EDGE ( 'NONE', *, *, #31938, .T. ) ;
#93258 = CARTESIAN_POINT ( 'NONE',  ( -1.050000000000038236, 2.500000000000000000, -1.818653347947326138 ) ) ;
#93259 = VERTEX_POINT ( 'NONE', #43443 ) ;
#93260 = EDGE_LOOP ( 'NONE', ( #70485, #119790, #103822, #77754 ) ) ;
#93261 = AXIS2_PLACEMENT_3D ( 'NONE', #58396, #116645, #16499 ) ;
#93262 = AXIS2_PLACEMENT_3D ( 'NONE', #67479, #117885, #26946 ) ;
#93263 = CARTESIAN_POINT ( 'NONE',  ( 0.1999999999999571565, 2.500000000000000000, 3.983716857408420076 ) ) ;
#93264 = CARTESIAN_POINT ( 'NONE',  ( 7.699999999999923794, 12.50000000000000000, 4.676537180435972552 ) ) ;
#93265 = DIRECTION ( 'NONE',  ( -4.274815082592931898E-19, -0.9999939076577903929, -0.003490651415223739937 ) ) ;
#93266 = EDGE_CURVE ( 'NONE', #56139, #116013, #128146, .T. ) ;
#93267 = ORIENTED_EDGE ( 'NONE', *, *, #80197, .F. ) ;
#93268 = CARTESIAN_POINT ( 'NONE',  ( 6.649999999999931077, 12.50000000000000000, -6.495190528383302464 ) ) ;
#93269 = ORIENTED_EDGE ( 'NONE', *, *, #77237, .F. ) ;
#93270 = ORIENTED_EDGE ( 'NONE', *, *, #86803, .T. ) ;
#93271 = FACE_OUTER_BOUND ( 'NONE', #81671, .T. ) ;
#93272 = FACE_OUTER_BOUND ( 'NONE', #91854, .T. ) ;
#93273 = AXIS2_PLACEMENT_3D ( 'NONE', #15624, #125581, #56827 ) ;
#93274 = ORIENTED_EDGE ( 'NONE', *, *, #93006, .F. ) ;
#93275 = VERTEX_POINT ( 'NONE', #114096 ) ;
#93276 = CARTESIAN_POINT ( 'NONE',  ( -6.850000000000017408, 2.500000000000000000, -6.841600689897077814 ) ) ;
#93277 = LINE ( 'NONE', #73619, #106002 ) ;
#93278 = DIRECTION ( 'NONE',  ( 0.000000000000000000, 0.000000000000000000, -1.000000000000000000 ) ) ;
#93279 = DIRECTION ( 'NONE',  ( 0.000000000000000000, -0.9999939076577903929, 0.003490651415223739937 ) ) ;
#93280 = DIRECTION ( 'NONE',  ( 0.000000000000000000, 0.000000000000000000, 1.000000000000000000 ) ) ;
#93281 = CONICAL_SURFACE ( 'NONE', #24320, 0.1000000000000002554, 0.003490658503988666988 ) ;
#93282 = CIRCLE ( 'NONE', #84955, 0.06509327318403741736 ) ;
#93283 = ORIENTED_EDGE ( 'NONE', *, *, #119233, .T. ) ;
#93284 = DIRECTION ( 'NONE',  ( 0.000000000000000000, 0.000000000000000000, 1.000000000000000000 ) ) ;
#93285 = VERTEX_POINT ( 'NONE', #42137 ) ;
#93286 = CARTESIAN_POINT ( 'NONE',  ( 87.50000000000002842, 7.500000000000000888, 0.6928095518838445210 ) ) ;
#93287 = ADVANCED_FACE ( 'NONE', ( #121987 ), #102352, .T. ) ;
#93288 = ORIENTED_EDGE ( 'NONE', *, *, #52052, .T. ) ;
#93289 = DIRECTION ( 'NONE',  ( 0.000000000000000000, 1.000000000000000000, 0.000000000000000000 ) ) ;
#93290 = CARTESIAN_POINT ( 'NONE',  ( 11.89999999999990443, 2.500000000000000000, 0.2464101615137736789 ) ) ;
#93291 = LINE ( 'NONE', #49683, #115528 ) ;
#93292 = DIRECTION ( 'NONE',  ( -4.274815082592931898E-19, -0.9999939076577903929, -0.003490651415223739937 ) ) ;
#93293 = ORIENTED_EDGE ( 'NONE', *, *, #95342, .T. ) ;
#93294 = AXIS2_PLACEMENT_3D ( 'NONE', #69861, #50231, #8987 ) ;
#93295 = EDGE_CURVE ( 'NONE', #93509, #80466, #52834, .T. ) ;
#93296 = CARTESIAN_POINT ( 'NONE',  ( -1.650000000000034328, 2.500000000000000000, -2.857883832488653741 ) ) ;
#93298 = AXIS2_PLACEMENT_3D ( 'NONE', #72006, #91631, #33379 ) ;
#93297 = CIRCLE ( 'NONE', #99573, 0.09999999999999982514 ) ;
#93299 = DIRECTION ( 'NONE',  ( -0.000000000000000000, -1.000000000000000000, -0.000000000000000000 ) ) ;
#93300 = ORIENTED_EDGE ( 'NONE', *, *, #1652, .F. ) ;
#93301 = ORIENTED_EDGE ( 'NONE', *, *, #46638, .F. ) ;
#93302 = ADVANCED_FACE ( 'NONE', ( #63062 ), #25726, .T. ) ;
#93304 = ORIENTED_EDGE ( 'NONE', *, *, #53036, .T. ) ;
#93303 = EDGE_CURVE ( 'NONE', #3765, #43648, #117645, .T. ) ;
#93305 = FACE_OUTER_BOUND ( 'NONE', #61747, .T. ) ;
#93306 = DIRECTION ( 'NONE',  ( 0.000000000000000000, 1.000000000000000000, 0.000000000000000000 ) ) ;
#93307 = EDGE_CURVE ( 'NONE', #31124, #120269, #122631, .T. ) ;
#93308 = CARTESIAN_POINT ( 'NONE',  ( 185.4843750003414300, -8.734944146203032389, -1.604583208406768146E-15 ) ) ;
#93309 = ADVANCED_FACE ( 'NONE', ( #56451 ), #46011, .T. ) ;
#93310 = DIRECTION ( 'NONE',  ( 0.000000000000000000, 0.000000000000000000, -1.000000000000000000 ) ) ;
#93311 = DIRECTION ( 'NONE',  ( 0.000000000000000000, 0.000000000000000000, 1.000000000000000000 ) ) ;
#93312 = FACE_OUTER_BOUND ( 'NONE', #38913, .T. ) ;
#93313 = DIRECTION ( 'NONE',  ( 0.000000000000000000, -0.9999939076577903929, 0.003490651415223739937 ) ) ;
#93314 = EDGE_CURVE ( 'NONE', #43343, #109816, #95747, .T. ) ;
#93315 = EDGE_CURVE ( 'NONE', #15536, #105793, #57023, .T. ) ;
#93316 = ADVANCED_FACE ( 'NONE', ( #79182 ), #25068, .T. ) ;
#93317 = ORIENTED_EDGE ( 'NONE', *, *, #17151, .T. ) ;
#93318 = EDGE_CURVE ( 'NONE', #21011, #54541, #65436, .T. ) ;
#93319 = DIRECTION ( 'NONE',  ( 0.000000000000000000, 1.000000000000000000, 0.000000000000000000 ) ) ;
#93320 = EDGE_CURVE ( 'NONE', #68464, #16720, #102997, .T. ) ;
#93321 = VERTEX_POINT ( 'NONE', #125834 ) ;
#93322 = LINE ( 'NONE', #125822, #94512 ) ;
#93323 = DIRECTION ( 'NONE',  ( 0.000000000000000000, 1.000000000000000000, 0.000000000000000000 ) ) ;
#93324 = DIRECTION ( 'NONE',  ( 0.000000000000000000, 0.000000000000000000, 1.000000000000000000 ) ) ;
#93325 = DIRECTION ( 'NONE',  ( 0.000000000000000000, 0.000000000000000000, 1.000000000000000000 ) ) ;
#93326 = EDGE_CURVE ( 'NONE', #102605, #88147, #119722, .T. ) ;
#93327 = EDGE_LOOP ( 'NONE', ( #35097, #127653, #127423, #50148 ) ) ;
#93328 = CIRCLE ( 'NONE', #11834, 0.06509327318403745899 ) ;
#93329 = AXIS2_PLACEMENT_3D ( 'NONE', #65453, #43271, #114553 ) ;
#93330 = PLANE ( 'NONE',  #15775 ) ;
#93332 = VERTEX_POINT ( 'NONE', #114732 ) ;
#93331 = CARTESIAN_POINT ( 'NONE',  ( 4.549999999999935874, 2.500000000000000000, 6.495190528383297135 ) ) ;
#93333 = EDGE_LOOP ( 'NONE', ( #65403, #84586 ) ) ;
#93335 = AXIS2_PLACEMENT_3D ( 'NONE', #82275, #23993, #22717 ) ;
#93334 = CIRCLE ( 'NONE', #36911, 0.06509327318403743123 ) ;
#93336 = CARTESIAN_POINT ( 'NONE',  ( -11.89999999999999503, 2.500000000000000000, 3.983716857408420076 ) ) ;
#93337 = EDGE_LOOP ( 'NONE', ( #111460, #51447, #47617, #53186 ) ) ;
#93338 = VERTEX_POINT ( 'NONE', #29429 ) ;
#93339 = CARTESIAN_POINT ( 'NONE',  ( -7.100000000000018296, 12.50000000000000000, 0.06509327318403504425 ) ) ;
#93340 = VERTEX_POINT ( 'NONE', #6682 ) ;
#93341 = CARTESIAN_POINT ( 'NONE',  ( 16.86689433361523172, 2.548103353433960994, -5.776876940644999792 ) ) ;
#93342 = DIRECTION ( 'NONE',  ( -4.274815082592931898E-19, -0.9999939076577903929, -0.003490651415223739937 ) ) ;
#93344 = CIRCLE ( 'NONE', #124656, 0.06509327318403745899 ) ;
#93343 = VECTOR ( 'NONE', #89126, 1000.000000000000000 ) ;
#93345 = CARTESIAN_POINT ( 'NONE',  ( -2.500000000000030642, 12.50000000000000000, -5.022947341949754119 ) ) ;
#93346 = ORIENTED_EDGE ( 'NONE', *, *, #93721, .F. ) ;
#93347 = CONICAL_SURFACE ( 'NONE', #57855, 0.09999999999999982514, 0.003490658503988666988 ) ;
#93348 = FACE_OUTER_BOUND ( 'NONE', #39612, .T. ) ;
#93350 = EDGE_LOOP ( 'NONE', ( #141, #99744 ) ) ;
#93349 = CARTESIAN_POINT ( 'NONE',  ( -6.700000000000016165, 12.50000000000000000, 4.330127018922196314 ) ) ;
#93351 = CARTESIAN_POINT ( 'NONE',  ( 17.50011901588676722, 2.224285231026832843, 4.071013062215452116 ) ) ;
#93352 = LINE ( 'NONE', #22048, #38372 ) ;
#93353 = ORIENTED_EDGE ( 'NONE', *, *, #21344, .F. ) ;
#93354 = ADVANCED_FACE ( 'NONE', ( #9776 ), #63295, .T. ) ;
#93355 = EDGE_LOOP ( 'NONE', ( #44075, #118929, #44361, #119843 ) ) ;
#93357 = ORIENTED_EDGE ( 'NONE', *, *, #102720, .T. ) ;
#93356 = EDGE_CURVE ( 'NONE', #99398, #54553, #125206, .T. ) ;
#93358 = EDGE_LOOP ( 'NONE', ( #8379, #8907 ) ) ;
#93359 = DIRECTION ( 'NONE',  ( 0.000000000000000000, -0.9999939076577903929, 0.003490651415223739937 ) ) ;
#93360 = CARTESIAN_POINT ( 'NONE',  ( -2.100000000000033396, 2.500000000000000000, 0.6928203230275494784 ) ) ;
#93361 = DIRECTION ( 'NONE',  ( -0.000000000000000000, 1.000000000000000000, -0.000000000000000000 ) ) ;
#93362 = FACE_BOUND ( 'NONE', #22133, .T. ) ;
#93363 = VERTEX_POINT ( 'NONE', #57103 ) ;
#93364 = AXIS2_PLACEMENT_3D ( 'NONE', #113698, #63299, #51563 ) ;
#93365 = CARTESIAN_POINT ( 'NONE',  ( 184.6562500006828031, 8.891194145520236347, 5.444286225454521982E-16 ) ) ;
#93366 = DIRECTION ( 'NONE',  ( 0.000000000000000000, -0.9999939076577903929, 0.003490651415223739937 ) ) ;
#93367 = DIRECTION ( 'NONE',  ( -0.000000000000000000, 1.000000000000000000, -0.000000000000000000 ) ) ;
#93368 = CIRCLE ( 'NONE', #104115, 0.06509327318403745899 ) ;
#93369 = EDGE_CURVE ( 'NONE', #94125, #52738, #6830, .T. ) ;
#93370 = AXIS2_PLACEMENT_3D ( 'NONE', #77558, #17996, #78232 ) ;
#93371 = LINE ( 'NONE', #13502, #63166 ) ;
#93372 = CARTESIAN_POINT ( 'NONE',  ( -8.350000000000013856, 2.500000000000000000, -7.188010851410848723 ) ) ;
#93373 = CARTESIAN_POINT ( 'NONE',  ( -5.400000000000020783, 2.500000000000000000, 4.922947341949748257 ) ) ;
#93374 = AXIS2_PLACEMENT_3D ( 'NONE', #73732, #113678, #74392 ) ;
#93375 = CONICAL_SURFACE ( 'NONE', #35003, 0.1000000000000002554, 0.003490658503988666988 ) ;
#93376 = LINE ( 'NONE', #122834, #80824 ) ;
#93377 = AXIS2_PLACEMENT_3D ( 'NONE', #47030, #45096, #84994 ) ;
#93378 = ORIENTED_EDGE ( 'NONE', *, *, #111801, .T. ) ;
#93379 = EDGE_LOOP ( 'NONE', ( #106596, #65658 ) ) ;
#93380 = EDGE_LOOP ( 'NONE', ( #88714, #40448 ) ) ;
#93381 = EDGE_LOOP ( 'NONE', ( #1743, #102524 ) ) ;
#93382 = ORIENTED_EDGE ( 'NONE', *, *, #60426, .T. ) ;
#93383 = DIRECTION ( 'NONE',  ( -0.000000000000000000, 1.000000000000000000, -0.000000000000000000 ) ) ;
#93384 = DIRECTION ( 'NONE',  ( 0.000000000000000000, 1.000000000000000000, 0.000000000000000000 ) ) ;
#93385 = CONICAL_SURFACE ( 'NONE', #39126, 0.09999999999999982514, 0.003490658503988666988 ) ;
#93386 = EDGE_LOOP ( 'NONE', ( #48571, #129467 ) ) ;
#93387 = FACE_BOUND ( 'NONE', #29272, .T. ) ;
#93389 = CARTESIAN_POINT ( 'NONE',  ( -10.85000000000000142, 12.50000000000000000, 6.495190528383297135 ) ) ;
#93388 = AXIS2_PLACEMENT_3D ( 'NONE', #14611, #25096, #61331 ) ;
#93391 = CIRCLE ( 'NONE', #36963, 0.06509327318403745899 ) ;
#93390 = CONICAL_SURFACE ( 'NONE', #105910, 0.09999999999999999167, 0.003490658503988666988 ) ;
#93392 = VERTEX_POINT ( 'NONE', #76105 ) ;
#93393 = CARTESIAN_POINT ( 'NONE',  ( 10.84999999999990905, 12.50000000000000000, -7.188010851410854052 ) ) ;
#93394 = DIRECTION ( 'NONE',  ( 0.000000000000000000, 0.000000000000000000, -1.000000000000000000 ) ) ;
#93395 = CARTESIAN_POINT ( 'NONE',  ( 7.899999999999924860, 12.50000000000000000, 5.088040615133786027 ) ) ;
#93396 = VERTEX_POINT ( 'NONE', #65631 ) ;
#93397 = DIRECTION ( 'NONE',  ( 0.000000000000000000, 0.000000000000000000, 1.000000000000000000 ) ) ;
#93398 = ADVANCED_FACE ( 'NONE', ( #34913 ), #128938, .T. ) ;
#93399 = ORIENTED_EDGE ( 'NONE', *, *, #81181, .T. ) ;
#93400 = ORIENTED_EDGE ( 'NONE', *, *, #108092, .T. ) ;
#93401 = EDGE_LOOP ( 'NONE', ( #128181, #63812 ) ) ;
#93402 = FACE_OUTER_BOUND ( 'NONE', #44763, .T. ) ;
#93403 = CARTESIAN_POINT ( 'NONE',  ( 11.69999999999990514, 2.500000000000000000, -2.276824562219559311E-15 ) ) ;
#93404 = PLANE ( 'NONE',  #38392 ) ;
#93405 = ORIENTED_EDGE ( 'NONE', *, *, #2053, .T. ) ;
#93406 = AXIS2_PLACEMENT_3D ( 'NONE', #33224, #14819, #43054 ) ;
#93407 = DIRECTION ( 'NONE',  ( 0.000000000000000000, 0.000000000000000000, 1.000000000000000000 ) ) ;
#93408 = CARTESIAN_POINT ( 'NONE',  ( -14.14999999999998614, 12.50000000000000000, -2.857883832488651521 ) ) ;
#93409 = FACE_OUTER_BOUND ( 'NONE', #41839, .T. ) ;
#93410 = CARTESIAN_POINT ( 'NONE',  ( 186.6979166673494603, 6.668395609140176816, 3.850000000000000977 ) ) ;
#93411 = ORIENTED_EDGE ( 'NONE', *, *, #88908, .T. ) ;
#93412 = ADVANCED_FACE ( 'NONE', ( #96367 ), #42478, .T. ) ;
#93413 = DIRECTION ( 'NONE',  ( 0.000000000000000000, 1.000000000000000000, 0.000000000000000000 ) ) ;
#93414 = EDGE_CURVE ( 'NONE', #97521, #2455, #54974, .T. ) ;
#93415 = ORIENTED_EDGE ( 'NONE', *, *, #97695, .T. ) ;
#93416 = DIRECTION ( 'NONE',  ( 0.000000000000000000, -0.000000000000000000, 1.000000000000000000 ) ) ;
#93417 = CIRCLE ( 'NONE', #13974, 0.06509327318403745899 ) ;
#93418 = ORIENTED_EDGE ( 'NONE', *, *, #70009, .F. ) ;
#93419 = AXIS2_PLACEMENT_3D ( 'NONE', #40544, #80458, #90907 ) ;
#93420 = ORIENTED_EDGE ( 'NONE', *, *, #114450, .T. ) ;
#93421 = DIRECTION ( 'NONE',  ( -4.274815082592931898E-19, -0.9999939076577903929, -0.003490651415223739937 ) ) ;
#93422 = PLANE ( 'NONE',  #25697 ) ;
#93423 = CARTESIAN_POINT ( 'NONE',  ( -5.600000000000020073, 2.500000000000000000, -0.3464101615137782364 ) ) ;
#93425 = ADVANCED_FACE ( 'NONE', ( #66280 ), #588, .T. ) ;
#93424 = PLANE ( 'NONE',  #69626 ) ;
#93426 = DIRECTION ( 'NONE',  ( -4.274815082592931898E-19, -0.9999939076577903929, -0.003490651415223739937 ) ) ;
#93427 = ORIENTED_EDGE ( 'NONE', *, *, #128621, .F. ) ;
#93430 = EDGE_LOOP ( 'NONE', ( #62819, #57588 ) ) ;
#93429 = AXIS2_PLACEMENT_3D ( 'NONE', #94647, #3068, #84834 ) ;
#93428 = AXIS2_PLACEMENT_3D ( 'NONE', #1256, #18941, #11714 ) ;
#93431 = DIRECTION ( 'NONE',  ( 0.000000000000000000, 1.000000000000000000, 0.000000000000000000 ) ) ;
#93432 = CARTESIAN_POINT ( 'NONE',  ( -0.4000000000000392131, 2.500000000000000000, -4.330127018922201643 ) ) ;
#93433 = DIRECTION ( 'NONE',  ( -0.000000000000000000, 1.000000000000000000, -0.000000000000000000 ) ) ;
#93434 = ORIENTED_EDGE ( 'NONE', *, *, #96693, .F. ) ;
#93435 = VERTEX_POINT ( 'NONE', #7346 ) ;
#93436 = FACE_OUTER_BOUND ( 'NONE', #91305, .T. ) ;
#93437 = CONICAL_SURFACE ( 'NONE', #120628, 0.1000000000000000472, 0.003490658503988666988 ) ;
#93438 = ORIENTED_EDGE ( 'NONE', *, *, #115019, .F. ) ;
#93439 = DIRECTION ( 'NONE',  ( 0.000000000000000000, 1.000000000000000000, 0.000000000000000000 ) ) ;
#93440 = DIRECTION ( 'NONE',  ( 0.000000000000000000, 0.000000000000000000, 1.000000000000000000 ) ) ;
#93441 = VERTEX_POINT ( 'NONE', #88986 ) ;
#93442 = CARTESIAN_POINT ( 'NONE',  ( 9.599999999999917932, 2.500000000000000000, -2.276824562219559311E-15 ) ) ;
#93443 = CARTESIAN_POINT ( 'NONE',  ( -0.6000000000000388356, 2.500000000000000000, 3.883716857408421319 ) ) ;
#93444 = DIRECTION ( 'NONE',  ( -4.274815082592931898E-19, -0.9999939076577903929, -0.003490651415223739937 ) ) ;
#93445 = DIRECTION ( 'NONE',  ( -4.274815082592931898E-19, -0.9999939076577903929, -0.003490651415223739937 ) ) ;
#93446 = VERTEX_POINT ( 'NONE', #39274 ) ;
#93447 = EDGE_CURVE ( 'NONE', #10025, #121831, #69325, .T. ) ;
#93448 = DIRECTION ( 'NONE',  ( -0.000000000000000000, -1.000000000000000000, -0.000000000000000000 ) ) ;
#93449 = CARTESIAN_POINT ( 'NONE',  ( 81.97673105525203141, -3.779183761609747005, 6.223416311177524918 ) ) ;
#93450 = EDGE_LOOP ( 'NONE', ( #102738, #107970, #101327, #106691 ) ) ;
#93451 = ORIENTED_EDGE ( 'NONE', *, *, #5394, .T. ) ;
#93452 = ADVANCED_FACE ( 'NONE', ( #30086 ), #90466, .T. ) ;
#93453 = CARTESIAN_POINT ( 'NONE',  ( 186.0468750003414300, -8.734944146203032389, -1.604583208406768146E-15 ) ) ;
#93454 = FACE_OUTER_BOUND ( 'NONE', #44587, .T. ) ;
#93455 = CONICAL_SURFACE ( 'NONE', #110187, 0.09999999999999982514, 0.003490658503988666988 ) ;
#93456 = CARTESIAN_POINT ( 'NONE',  ( -2.050000000000032685, 12.50000000000000000, -6.430097255199264339 ) ) ;
#93457 = AXIS2_PLACEMENT_3D ( 'NONE', #40634, #68769, #39970 ) ;
#93458 = EDGE_CURVE ( 'NONE', #17249, #75945, #121874, .T. ) ;
#93460 = CIRCLE ( 'NONE', #28716, 0.06509327318403745899 ) ;
#93459 = CARTESIAN_POINT ( 'NONE',  ( 11.64999999999990621, 2.500000000000000000, -2.165063509461101710 ) ) ;
#93461 = DIRECTION ( 'NONE',  ( 0.000000000000000000, 0.000000000000000000, -1.000000000000000000 ) ) ;
#93462 = DIRECTION ( 'NONE',  ( -0.000000000000000000, -1.000000000000000000, -0.000000000000000000 ) ) ;
#93463 = VECTOR ( 'NONE', #31073, 1000.000000000000000 ) ;
#93464 = CARTESIAN_POINT ( 'NONE',  ( -8.749999999999971578, 2.500000000000000000, 6.395190528383296602 ) ) ;
#93465 = CARTESIAN_POINT ( 'NONE',  ( -5.850000000000018296, 2.500000000000000000, 5.802370205355744659 ) ) ;
#93466 = CARTESIAN_POINT ( 'NONE',  ( 3.549999999999942979, 2.500000000000000000, 1.918653347947321564 ) ) ;
#93467 = DIRECTION ( 'NONE',  ( 0.000000000000000000, 0.000000000000000000, 1.000000000000000000 ) ) ;
#93468 = EDGE_CURVE ( 'NONE', #115231, #122569, #4784, .T. ) ;
#93469 = EDGE_CURVE ( 'NONE', #20166, #39360, #98890, .T. ) ;
#93470 = EDGE_CURVE ( 'NONE', #57519, #16723, #40555, .T. ) ;
#93471 = AXIS2_PLACEMENT_3D ( 'NONE', #80205, #21265, #31746 ) ;
#93472 = AXIS2_PLACEMENT_3D ( 'NONE', #56663, #106429, #54737 ) ;
#93473 = CARTESIAN_POINT ( 'NONE',  ( -11.44999999999999751, 12.50000000000000000, 1.818653347947321475 ) ) ;
#93474 = ORIENTED_EDGE ( 'NONE', *, *, #21663, .F. ) ;
#93475 = ORIENTED_EDGE ( 'NONE', *, *, #86906, .F. ) ;
#93476 = AXIS2_PLACEMENT_3D ( 'NONE', #76749, #37485, #48584 ) ;
#93477 = EDGE_CURVE ( 'NONE', #119959, #63523, #32017, .T. ) ;
#93478 = EDGE_LOOP ( 'NONE', ( #64120, #120602, #2591, #26119 ) ) ;
#93479 = ORIENTED_EDGE ( 'NONE', *, *, #62068, .T. ) ;
#93480 = AXIS2_PLACEMENT_3D ( 'NONE', #90181, #120315, #41128 ) ;
#93481 = FACE_OUTER_BOUND ( 'NONE', #109353, .T. ) ;
#93482 = CARTESIAN_POINT ( 'NONE',  ( -13.74999999999998934, 2.500000000000000000, 2.857883832488652853 ) ) ;
#93483 = EDGE_CURVE ( 'NONE', #39312, #13198, #38370, .T. ) ;
#93484 = CONICAL_SURFACE ( 'NONE', #3393, 0.09999999999999982514, 0.003490658503988666988 ) ;
#93485 = ORIENTED_EDGE ( 'NONE', *, *, #53901, .F. ) ;
#93486 = CYLINDRICAL_SURFACE ( 'NONE', #61123, 1.000000000000000888 ) ;
#93487 = CIRCLE ( 'NONE', #68429, 0.09999999999999982514 ) ;
#93488 = DIRECTION ( 'NONE',  ( -0.000000000000000000, -1.000000000000000000, -0.000000000000000000 ) ) ;
#93490 = ORIENTED_EDGE ( 'NONE', *, *, #126407, .T. ) ;
#93489 = DIRECTION ( 'NONE',  ( 0.000000000000000000, 0.000000000000000000, -1.000000000000000000 ) ) ;
#93491 = DIRECTION ( 'NONE',  ( 0.000000000000000000, 0.000000000000000000, -1.000000000000000000 ) ) ;
#93492 = DIRECTION ( 'NONE',  ( -0.000000000000000000, -1.000000000000000000, -0.000000000000000000 ) ) ;
#93493 = EDGE_LOOP ( 'NONE', ( #50936, #36850, #65574, #111795 ) ) ;
#93494 = VERTEX_POINT ( 'NONE', #129582 ) ;
#93495 = ORIENTED_EDGE ( 'NONE', *, *, #89334, .T. ) ;
#93496 = EDGE_LOOP ( 'NONE', ( #104172, #59046, #62437, #126124 ) ) ;
#93497 = CARTESIAN_POINT ( 'NONE',  ( -6.850000000000017408, 12.50000000000000000, -6.841600689897077814 ) ) ;
#93498 = AXIS2_PLACEMENT_3D ( 'NONE', #94196, #7084, #85661 ) ;
#93499 = DIRECTION ( 'NONE',  ( -0.000000000000000000, 1.000000000000000000, -0.000000000000000000 ) ) ;
#93500 = DIRECTION ( 'NONE',  ( -0.000000000000000000, 1.000000000000000000, -0.000000000000000000 ) ) ;
#93501 = CARTESIAN_POINT ( 'NONE',  ( 11.24999999999990585, 2.500000000000000000, 2.957883832488649389 ) ) ;
#93502 = VERTEX_POINT ( 'NONE', #21533 ) ;
#93503 = DIRECTION ( 'NONE',  ( 0.000000000000000000, -0.000000000000000000, 1.000000000000000000 ) ) ;
#93504 = ORIENTED_EDGE ( 'NONE', *, *, #33389, .T. ) ;
#93505 = DIRECTION ( 'NONE',  ( -4.274815082592931898E-19, -0.9999939076577903929, -0.003490651415223739937 ) ) ;
#93506 = DIRECTION ( 'NONE',  ( 0.000000000000000000, 1.000000000000000000, 0.000000000000000000 ) ) ;
#93507 = DIRECTION ( 'NONE',  ( 0.000000000000000000, -0.9999939076577903929, 0.003490651415223739937 ) ) ;
#93508 = DIRECTION ( 'NONE',  ( -0.000000000000000000, 1.000000000000000000, -0.000000000000000000 ) ) ;
#93509 = VERTEX_POINT ( 'NONE', #32672 ) ;
#93510 = AXIS2_PLACEMENT_3D ( 'NONE', #54148, #63966, #113053 ) ;
#93511 = EDGE_CURVE ( 'NONE', #38170, #29262, #100722, .T. ) ;
#93512 = CIRCLE ( 'NONE', #89400, 0.06509327318403745899 ) ;
#93513 = ORIENTED_EDGE ( 'NONE', *, *, #19383, .T. ) ;
#93514 = EDGE_LOOP ( 'NONE', ( #98074, #84888, #96288, #54445 ) ) ;
#93515 = FACE_OUTER_BOUND ( 'NONE', #57725, .T. ) ;
#93516 = DIRECTION ( 'NONE',  ( 0.000000000000000000, 0.000000000000000000, 1.000000000000000000 ) ) ;
#93517 = CARTESIAN_POINT ( 'NONE',  ( -10.00000000000000355, 2.500000000000000000, 3.637306695894644726 ) ) ;
#93518 = FACE_BOUND ( 'NONE', #7765, .T. ) ;
#93519 = CARTESIAN_POINT ( 'NONE',  ( 5.399999999999931966, 2.500000000000000000, 4.330127018922196314 ) ) ;
#93520 = DIRECTION ( 'NONE',  ( -4.274815082592931898E-19, -0.9999939076577903929, -0.003490651415223739937 ) ) ;
#93521 = AXIS2_PLACEMENT_3D ( 'NONE', #29416, #10406, #120373 ) ;
#93522 = FACE_OUTER_BOUND ( 'NONE', #13418, .T. ) ;
#93523 = EDGE_CURVE ( 'NONE', #36055, #45761, #10419, .T. ) ;
#93524 = CARTESIAN_POINT ( 'NONE',  ( 12.09999999999990550, 2.500000000000000000, -5.022947341949754119 ) ) ;
#93525 = DIRECTION ( 'NONE',  ( 0.000000000000000000, 0.000000000000000000, 1.000000000000000000 ) ) ;
#93526 = FACE_OUTER_BOUND ( 'NONE', #125729, .T. ) ;
#93527 = ORIENTED_EDGE ( 'NONE', *, *, #103340, .T. ) ;
#93529 = CIRCLE ( 'NONE', #32918, 0.06509327318403745899 ) ;
#93528 = CONICAL_SURFACE ( 'NONE', #68477, 0.1000000000000000472, 0.003490658503988666988 ) ;
#93530 = CONICAL_SURFACE ( 'NONE', #51770, 0.1000000000000002554, 0.003490658503988666988 ) ;
#93531 = DIRECTION ( 'NONE',  ( -0.000000000000000000, -1.000000000000000000, -0.000000000000000000 ) ) ;
#93532 = EDGE_LOOP ( 'NONE', ( #7711, #74492 ) ) ;
#93533 = VERTEX_POINT ( 'NONE', #11048 ) ;
#93534 = ORIENTED_EDGE ( 'NONE', *, *, #113353, .F. ) ;
#93535 = ORIENTED_EDGE ( 'NONE', *, *, #68146, .T. ) ;
#93536 = DIRECTION ( 'NONE',  ( 0.000000000000000000, 1.000000000000000000, 0.000000000000000000 ) ) ;
#93537 = FACE_BOUND ( 'NONE', #123300, .T. ) ;
#93538 = DIRECTION ( 'NONE',  ( 0.000000000000000000, 0.000000000000000000, 1.000000000000000000 ) ) ;
#93539 = CONICAL_SURFACE ( 'NONE', #30863, 0.1000000000000002554, 0.003490658503988666988 ) ;
#93540 = CIRCLE ( 'NONE', #104008, 0.09999999999999999167 ) ;
#93541 = VERTEX_POINT ( 'NONE', #90250 ) ;
#93542 = CARTESIAN_POINT ( 'NONE',  ( 59.88499455100932067, 2.860410828906190250, 5.641292085229139275 ) ) ;
#93543 = DIRECTION ( 'NONE',  ( 0.000000000000000000, -0.9999939076577903929, 0.003490651415223739937 ) ) ;
#93544 = AXIS2_PLACEMENT_3D ( 'NONE', #90836, #24522, #84073 ) ;
#93545 = EDGE_LOOP ( 'NONE', ( #102657, #81981, #105171, #129351 ) ) ;
#93546 = DIRECTION ( 'NONE',  ( 1.000000000000000000, 0.000000000000000000, 0.000000000000000000 ) ) ;
#93547 = VECTOR ( 'NONE', #38471, 1000.000000000000000 ) ;
#93548 = CARTESIAN_POINT ( 'NONE',  ( 1.649999999999951505, 2.500000000000000000, 1.472243186433545459 ) ) ;
#93549 = ADVANCED_FACE ( 'NONE', ( #51013 ), #15339, .T. ) ;
#93550 = CIRCLE ( 'NONE', #74778, 0.09999999999999982514 ) ;
#93551 = ORIENTED_EDGE ( 'NONE', *, *, #35989, .T. ) ;
#93552 = CARTESIAN_POINT ( 'NONE',  ( -0.4500000000000397571, 12.50000000000000000, -6.430097255199264339 ) ) ;
#93553 = CARTESIAN_POINT ( 'NONE',  ( -13.09999999999999076, 12.50000000000000000, 3.983716857408420964 ) ) ;
#93554 = AXIS2_PLACEMENT_3D ( 'NONE', #72323, #84048, #104346 ) ;
#93555 = CIRCLE ( 'NONE', #95715, 0.06509327318403745899 ) ;
#93556 = ADVANCED_FACE ( 'NONE', ( #11706 ), #84313, .T. ) ;
#93557 = ORIENTED_EDGE ( 'NONE', *, *, #23697, .T. ) ;
#93558 = CONICAL_SURFACE ( 'NONE', #72638, 0.1000000000000000472, 0.003490658503988666988 ) ;
#93559 = AXIS2_PLACEMENT_3D ( 'NONE', #64187, #43926, #34754 ) ;
#93560 = LINE ( 'NONE', #46374, #55127 ) ;
#93561 = B_SPLINE_CURVE_WITH_KNOTS ( 'NONE', 3,
 ( #96719, #7043, #58749, #47001, #128135, #117634, #67912, #86905 ),
 .UNSPECIFIED., .F., .F.,
 ( 4, 2, 2, 4 ),
 ( -0.0001155885020466859676, 0.03307027595371006545, 0.04966320818158844602, 0.06625614040946682659 ),
 .UNSPECIFIED. ) ;
#93562 = CARTESIAN_POINT ( 'NONE',  ( 4.599999999999937472, 2.500000000000000000, 0.5928203230275495006 ) ) ;
#93563 = CARTESIAN_POINT ( 'NONE',  ( -8.750000000000007105, 2.500000000000000000, 7.188010851410848723 ) ) ;
#93564 = EDGE_LOOP ( 'NONE', ( #67646, #44165 ) ) ;
#93565 = ADVANCED_FACE ( 'NONE', ( #20890 ), #103096, .T. ) ;
#93566 = ORIENTED_EDGE ( 'NONE', *, *, #49763, .T. ) ;
#93567 = EDGE_CURVE ( 'NONE', #12736, #118052, #72577, .T. ) ;
#93568 = CARTESIAN_POINT ( 'NONE',  ( -6.050000000000018474, 2.500000000000000000, 6.941600689897073018 ) ) ;
#93569 = EDGE_LOOP ( 'NONE', ( #55930, #111397, #12174, #432 ) ) ;
#93570 = CARTESIAN_POINT ( 'NONE',  ( 2.299999999999948752, 2.500000000000000000, 0.2464101615137735679 ) ) ;
#93571 = DIRECTION ( 'NONE',  ( -4.274815082592931898E-19, -0.9999939076577903929, -0.003490651415223739937 ) ) ;
#93573 = AXIS2_PLACEMENT_3D ( 'NONE', #16526, #76116, #77405 ) ;
#93572 = AXIS2_PLACEMENT_3D ( 'NONE', #40825, #81388, #82676 ) ;
#93574 = VERTEX_POINT ( 'NONE', #71938 ) ;
#93575 = EDGE_CURVE ( 'NONE', #96273, #1760, #55071, .T. ) ;
#93576 = DIRECTION ( 'NONE',  ( -0.000000000000000000, -1.000000000000000000, -0.000000000000000000 ) ) ;
#93577 = DIRECTION ( 'NONE',  ( 0.000000000000000000, 0.000000000000000000, -1.000000000000000000 ) ) ;
#93578 = DIRECTION ( 'NONE',  ( 0.000000000000000000, 0.000000000000000000, -1.000000000000000000 ) ) ;
#93579 = DIRECTION ( 'NONE',  ( 0.000000000000000000, 1.000000000000000000, 0.000000000000000000 ) ) ;
#93580 = EDGE_CURVE ( 'NONE', #27907, #9598, #112498, .T. ) ;
#93581 = LINE ( 'NONE', #112583, #26519 ) ;
#93582 = VERTEX_POINT ( 'NONE', #22199 ) ;
#93583 = ORIENTED_EDGE ( 'NONE', *, *, #44168, .F. ) ;
#93584 = CARTESIAN_POINT ( 'NONE',  ( -3.550000000000028688, 2.500000000000000000, 6.941600689897073018 ) ) ;
#93585 = CARTESIAN_POINT ( 'NONE',  ( -14.34999999999998543, 12.50000000000000000, 1.883746621131362931 ) ) ;
#93587 = ORIENTED_EDGE ( 'NONE', *, *, #63597, .F. ) ;
#93586 = ORIENTED_EDGE ( 'NONE', *, *, #84555, .T. ) ;
#93588 = EDGE_LOOP ( 'NONE', ( #94659, #68114, #124790, #97468 ) ) ;
#93589 = AXIS2_PLACEMENT_3D ( 'NONE', #90152, #88889, #488 ) ;
#93590 = DIRECTION ( 'NONE',  ( 0.000000000000000000, -0.9999939076577903929, 0.003490651415223739937 ) ) ;
#93591 = DIRECTION ( 'NONE',  ( 0.000000000000000000, 1.000000000000000000, 0.000000000000000000 ) ) ;
#93592 = DIRECTION ( 'NONE',  ( -0.000000000000000000, -1.000000000000000000, -0.000000000000000000 ) ) ;
#93593 = DIRECTION ( 'NONE',  ( 0.000000000000000000, 1.000000000000000000, 0.000000000000000000 ) ) ;
#93594 = FACE_OUTER_BOUND ( 'NONE', #30795, .T. ) ;
#93595 = FACE_OUTER_BOUND ( 'NONE', #119052, .T. ) ;
#93596 = DIRECTION ( 'NONE',  ( -0.000000000000000000, 1.000000000000000000, -0.000000000000000000 ) ) ;
#93597 = CARTESIAN_POINT ( 'NONE',  ( 2.099999999999950351, 12.50000000000000000, -2.276824562219559311E-15 ) ) ;
#93598 = CARTESIAN_POINT ( 'NONE',  ( -2.950000000000029932, 2.500000000000000000, -2.265063509461101798 ) ) ;
#93600 = ORIENTED_EDGE ( 'NONE', *, *, #9797, .F. ) ;
#93599 = AXIS2_PLACEMENT_3D ( 'NONE', #8096, #7446, #87931 ) ;
#93601 = EDGE_CURVE ( 'NONE', #11848, #128991, #121979, .T. ) ;
#93602 = CIRCLE ( 'NONE', #26704, 0.06509327318403745899 ) ;
#93603 = CARTESIAN_POINT ( 'NONE',  ( -4.600000000000025402, 12.50000000000000000, 4.330127018922196314 ) ) ;
#93604 = EDGE_LOOP ( 'NONE', ( #28066, #33688, #57192, #83673 ) ) ;
#93605 = EDGE_LOOP ( 'NONE', ( #95796, #76058 ) ) ;
#93606 = CARTESIAN_POINT ( 'NONE',  ( 8.149999999999923972, 2.500000000000000000, -6.741600689897077281 ) ) ;
#93607 = DIRECTION ( 'NONE',  ( 0.000000000000000000, 0.000000000000000000, 1.000000000000000000 ) ) ;
#93608 = FACE_OUTER_BOUND ( 'NONE', #27873, .T. ) ;
#93610 = EDGE_CURVE ( 'NONE', #29262, #50768, #126174, .T. ) ;
#93609 = CONICAL_SURFACE ( 'NONE', #32987, 0.1000000000000002554, 0.003490658503988666988 ) ;
#93611 = DIRECTION ( 'NONE',  ( 0.000000000000000000, 1.000000000000000000, 0.000000000000000000 ) ) ;
#93612 = AXIS2_PLACEMENT_3D ( 'NONE', #1983, #41933, #100821 ) ;
#93613 = AXIS2_PLACEMENT_3D ( 'NONE', #86645, #109515, #68936 ) ;
#93614 = CARTESIAN_POINT ( 'NONE',  ( 8.749999999999918288, 12.50000000000000000, -1.472243186433550122 ) ) ;
#93615 = CARTESIAN_POINT ( 'NONE',  ( 185.7812500006828031, 0.000000000000000000, 7.700000000000000178 ) ) ;
#93616 = DIRECTION ( 'NONE',  ( 0.000000000000000000, 0.000000000000000000, 1.000000000000000000 ) ) ;
#93617 = VERTEX_POINT ( 'NONE', #121021 ) ;
#93618 = CARTESIAN_POINT ( 'NONE',  ( -2.100000000000034728, 12.50000000000000000, 4.265033745738159077 ) ) ;
#93619 = EDGE_CURVE ( 'NONE', #27240, #48072, #19569, .T. ) ;
#93620 = EDGE_CURVE ( 'NONE', #54758, #51555, #128251, .T. ) ;
#93621 = ADVANCED_FACE ( 'NONE', ( #43770 ), #34149, .T. ) ;
#93622 = CARTESIAN_POINT ( 'NONE',  ( -7.900000000000014566, 12.50000000000000000, -5.022947341949754119 ) ) ;
#93623 = ORIENTED_EDGE ( 'NONE', *, *, #88840, .T. ) ;
#93624 = CIRCLE ( 'NONE', #49727, 0.1000000000000000472 ) ;
#93625 = VERTEX_POINT ( 'NONE', #94133 ) ;
#93626 = ADVANCED_FACE ( 'NONE', ( #65960 ), #44389, .T. ) ;
#93627 = ORIENTED_EDGE ( 'NONE', *, *, #28334, .F. ) ;
#93628 = CIRCLE ( 'NONE', #110348, 0.09999999999999982514 ) ;
#93629 = VERTEX_POINT ( 'NONE', #14274 ) ;
#93630 = CARTESIAN_POINT ( 'NONE',  ( 4.599999999999940137, 2.500000000000000000, -4.430127018922202176 ) ) ;
#93631 = DIRECTION ( 'NONE',  ( 0.000000000000000000, 1.000000000000000000, 0.000000000000000000 ) ) ;
#93632 = ADVANCED_FACE ( 'NONE', ( #83046 ), #9098, .T. ) ;
#93633 = AXIS2_PLACEMENT_3D ( 'NONE', #112680, #46340, #126200 ) ;
#93634 = EDGE_CURVE ( 'NONE', #109159, #31303, #54220, .T. ) ;
#93635 = DIRECTION ( 'NONE',  ( 0.000000000000000000, 1.000000000000000000, 0.000000000000000000 ) ) ;
#93636 = CARTESIAN_POINT ( 'NONE',  ( -4.400000000000025224, 2.500000000000000000, 0.2464101615137735679 ) ) ;
#93637 = CIRCLE ( 'NONE', #95777, 0.06509327318403745899 ) ;
#93638 = DIRECTION ( 'NONE',  ( -0.000000000000000000, -1.000000000000000000, -0.000000000000000000 ) ) ;
#93639 = EDGE_LOOP ( 'NONE', ( #112673, #77641 ) ) ;
#93640 = CARTESIAN_POINT ( 'NONE',  ( 2.099999999999950351, 12.50000000000000000, -0.6928203230275541413 ) ) ;
#93641 = DIRECTION ( 'NONE',  ( -0.000000000000000000, 1.000000000000000000, -0.000000000000000000 ) ) ;
#93642 = CARTESIAN_POINT ( 'NONE',  ( -9.350000000000006750, 12.50000000000000000, 2.446380397790835826 ) ) ;
#93643 = VECTOR ( 'NONE', #73453, 1000.000000000000000 ) ;
#93644 = CONICAL_SURFACE ( 'NONE', #70653, 0.09999999999999982514, 0.003490658503988666988 ) ;
#93645 = FACE_OUTER_BOUND ( 'NONE', #111324, .T. ) ;
#93646 = VERTEX_POINT ( 'NONE', #115045 ) ;
#93647 = VECTOR ( 'NONE', #46018, 1000.000000000000000 ) ;
#93648 = EDGE_LOOP ( 'NONE', ( #100280, #112698, #108576, #70385 ) ) ;
#93649 = ORIENTED_EDGE ( 'NONE', *, *, #68329, .F. ) ;
#93650 = DIRECTION ( 'NONE',  ( 0.000000000000000000, 1.000000000000000000, 0.000000000000000000 ) ) ;
#93651 = AXIS2_PLACEMENT_3D ( 'NONE', #55880, #37551, #56523 ) ;
#93652 = VECTOR ( 'NONE', #39506, 1000.000000000000000 ) ;
#93653 = CARTESIAN_POINT ( 'NONE',  ( 2.099999999999950351, 12.50000000000000000, -0.6277270498435166823 ) ) ;
#93654 = DIRECTION ( 'NONE',  ( 0.000000000000000000, 1.000000000000000000, 0.000000000000000000 ) ) ;
#93655 = AXIS2_PLACEMENT_3D ( 'NONE', #6373, #86896, #125532 ) ;
#93656 = VERTEX_POINT ( 'NONE', #55507 ) ;
#93657 = DIRECTION ( 'NONE',  ( -0.000000000000000000, 1.000000000000000000, -0.000000000000000000 ) ) ;
#93659 = AXIS2_PLACEMENT_3D ( 'NONE', #117018, #98045, #96110 ) ;
#93658 = DIRECTION ( 'NONE',  ( -0.000000000000000000, 1.000000000000000000, -0.000000000000000000 ) ) ;
#93660 = PLANE ( 'NONE',  #10642 ) ;
#93661 = DIRECTION ( 'NONE',  ( 0.000000000000000000, -0.9999939076577903929, 0.003490651415223739937 ) ) ;
#93662 = CONICAL_SURFACE ( 'NONE', #104128, 0.1000000000000002554, 0.003490658503988666988 ) ;
#93663 = CYLINDRICAL_SURFACE ( 'NONE', #3935, 2.000000000000000000 ) ;
#93664 = EDGE_CURVE ( 'NONE', #76363, #115754, #43134, .T. ) ;
#93665 = VERTEX_POINT ( 'NONE', #124250 ) ;
#93666 = ORIENTED_EDGE ( 'NONE', *, *, #21332, .F. ) ;
#93667 = CARTESIAN_POINT ( 'NONE',  ( 129.5000000000000000, 1.375000000000002442, -6.000000000000000888 ) ) ;
#93668 = DIRECTION ( 'NONE',  ( -0.000000000000000000, -1.000000000000000000, -0.000000000000000000 ) ) ;
#93669 = DIRECTION ( 'NONE',  ( 0.000000000000000000, 0.000000000000000000, -1.000000000000000000 ) ) ;
#93670 = CARTESIAN_POINT ( 'NONE',  ( 9.349999999999919709, 2.500000000000000000, 1.718653347947321386 ) ) ;
#93671 = DIRECTION ( 'NONE',  ( 0.000000000000000000, 0.000000000000000000, 1.000000000000000000 ) ) ;
#93672 = EDGE_CURVE ( 'NONE', #98954, #56105, #63393, .T. ) ;
#93673 = ORIENTED_EDGE ( 'NONE', *, *, #79401, .F. ) ;
#93674 = ORIENTED_EDGE ( 'NONE', *, *, #32846, .T. ) ;
#93675 = DIRECTION ( 'NONE',  ( 0.000000000000000000, 0.000000000000000000, 1.000000000000000000 ) ) ;
#93676 = DIRECTION ( 'NONE',  ( 0.000000000000000000, -0.9999939076577903929, 0.003490651415223739937 ) ) ;
#93677 = CARTESIAN_POINT ( 'NONE',  ( 17.46224641144930345, -2.500000000000000000, -5.244174873161000505 ) ) ;
#93678 = FACE_OUTER_BOUND ( 'NONE', #93694, .T. ) ;
#93679 = EDGE_LOOP ( 'NONE', ( #10678, #115103 ) ) ;
#93680 = CARTESIAN_POINT ( 'NONE',  ( 8.149999999999920419, 2.500000000000000000, 6.741600689897071952 ) ) ;
#93681 = CARTESIAN_POINT ( 'NONE',  ( -6.850000000000017408, 2.500000000000000000, -1.818653347947325916 ) ) ;
#93682 = AXIS2_PLACEMENT_3D ( 'NONE', #673, #111928, #40636 ) ;
#93683 = CIRCLE ( 'NONE', #18465, 0.1000000000000000472 ) ;
#93684 = EDGE_LOOP ( 'NONE', ( #31261, #100551 ) ) ;
#93685 = AXIS2_PLACEMENT_3D ( 'NONE', #93403, #80373, #21431 ) ;
#93686 = CARTESIAN_POINT ( 'NONE',  ( -5.450000000000023270, 2.500000000000000000, -6.495190528383302464 ) ) ;
#93687 = VERTEX_POINT ( 'NONE', #84312 ) ;
#93688 = CARTESIAN_POINT ( 'NONE',  ( 8.099999999999923261, 12.50000000000000000, 4.676537180435972552 ) ) ;
#93689 = AXIS2_PLACEMENT_3D ( 'NONE', #30999, #72831, #83304 ) ;
#93690 = CONICAL_SURFACE ( 'NONE', #10166, 0.09999999999999999167, 0.003490658503988666988 ) ;
#93691 = ORIENTED_EDGE ( 'NONE', *, *, #24708, .F. ) ;
#93692 = FACE_OUTER_BOUND ( 'NONE', #34820, .T. ) ;
#93693 = PLANE ( 'NONE',  #92014 ) ;
#93694 = EDGE_LOOP ( 'NONE', ( #11539, #115976, #120469, #1811 ) ) ;
#93695 = ORIENTED_EDGE ( 'NONE', *, *, #103081, .F. ) ;
#93696 = CARTESIAN_POINT ( 'NONE',  ( 184.7552083336747444, 6.551208109652275624, -3.782341765624998686 ) ) ;
#93697 = CARTESIAN_POINT ( 'NONE',  ( -10.65000000000000391, 12.50000000000000000, -6.213873640053560798 ) ) ;
#93698 = CONICAL_SURFACE ( 'NONE', #53997, 0.1000000000000002554, 0.003490658503988666988 ) ;
#93699 = DIRECTION ( 'NONE',  ( -0.000000000000000000, 1.000000000000000000, -0.000000000000000000 ) ) ;
#93700 = CARTESIAN_POINT ( 'NONE',  ( 184.3177083336747160, 4.367472073101515306, 7.564683531250000925 ) ) ;
#93701 = CONICAL_SURFACE ( 'NONE', #16314, 0.09999999999999982514, 0.003490658503988666988 ) ;
#93702 = DIRECTION ( 'NONE',  ( 0.000000000000000000, 1.000000000000000000, 0.000000000000000000 ) ) ;
#93703 = DIRECTION ( 'NONE',  ( 0.000000000000000000, 0.000000000000000000, 1.000000000000000000 ) ) ;
#93704 = DIRECTION ( 'NONE',  ( 0.000000000000000000, 1.000000000000000000, 0.000000000000000000 ) ) ;
#93705 = FACE_OUTER_BOUND ( 'NONE', #44957, .T. ) ;
#93707 = EDGE_CURVE ( 'NONE', #97182, #98382, #114413, .T. ) ;
#93706 = AXIS2_PLACEMENT_3D ( 'NONE', #117037, #37230, #8385 ) ;
#93708 = EDGE_LOOP ( 'NONE', ( #95371, #65754, #95138, #34160 ) ) ;
#93709 = EDGE_LOOP ( 'NONE', ( #73171, #14362 ) ) ;
#93710 = DIRECTION ( 'NONE',  ( 0.000000000000000000, 0.000000000000000000, 1.000000000000000000 ) ) ;
#93711 = ORIENTED_EDGE ( 'NONE', *, *, #109698, .F. ) ;
#93712 = FACE_OUTER_BOUND ( 'NONE', #3873, .T. ) ;
#93713 = DIRECTION ( 'NONE',  ( -0.000000000000000000, -1.000000000000000000, -0.000000000000000000 ) ) ;
#93714 = CIRCLE ( 'NONE', #95770, 0.1000000000000002554 ) ;
#93715 = CARTESIAN_POINT ( 'NONE',  ( 7.499999999999925393, 2.500000000000000000, -0.6928203230275541413 ) ) ;
#93717 = ORIENTED_EDGE ( 'NONE', *, *, #17806, .T. ) ;
#93716 = EDGE_LOOP ( 'NONE', ( #46999, #112789, #123768, #25315 ) ) ;
#93718 = ADVANCED_FACE ( 'NONE', ( #54840 ), #35866, .T. ) ;
#93719 = FACE_BOUND ( 'NONE', #23391, .T. ) ;
#93720 = VERTEX_POINT ( 'NONE', #24761 ) ;
#93721 = EDGE_CURVE ( 'NONE', #89399, #110447, #92733, .T. ) ;
#93722 = DIRECTION ( 'NONE',  ( 0.000000000000000000, -0.000000000000000000, 1.000000000000000000 ) ) ;
#93723 = CARTESIAN_POINT ( 'NONE',  ( 4.549999999999939426, 12.50000000000000000, -6.495190528383302464 ) ) ;
#93724 = ORIENTED_EDGE ( 'NONE', *, *, #53680, .F. ) ;
#93725 = CARTESIAN_POINT ( 'NONE',  ( 1.249999999999950262, 2.500000000000000000, 7.088010851410848190 ) ) ;
#93726 = CIRCLE ( 'NONE', #95775, 0.09999999999999982514 ) ;
#93727 = DIRECTION ( 'NONE',  ( 0.000000000000000000, 0.000000000000000000, -1.000000000000000000 ) ) ;
#93728 = CARTESIAN_POINT ( 'NONE',  ( -2.100000000000034284, 12.50000000000000000, 0.06509327318403504425 ) ) ;
#93729 = CARTESIAN_POINT ( 'NONE',  ( -4.150000000000027889, 2.500000000000000000, -7.188010851410854052 ) ) ;
#93730 = EDGE_CURVE ( 'NONE', #112512, #120557, #107298, .T. ) ;
#93731 = DIRECTION ( 'NONE',  ( -4.274815082592931898E-19, -0.9999939076577903929, -0.003490651415223739937 ) ) ;
#93732 = ADVANCED_FACE ( 'NONE', ( #53580 ), #98986, .T. ) ;
#93733 = CARTESIAN_POINT ( 'NONE',  ( -9.150000000000005684, 12.50000000000000000, 6.495190528383297135 ) ) ;
#93734 = CARTESIAN_POINT ( 'NONE',  ( 186.0260416670080588, -6.551208109652273848, -3.782341765625003571 ) ) ;
#93735 = CARTESIAN_POINT ( 'NONE',  ( 11.24999999999991118, 2.500000000000000000, 5.902370205355745192 ) ) ;
#93736 = ADVANCED_FACE ( 'NONE', ( #5099 ), #36313, .T. ) ;
#93737 = CIRCLE ( 'NONE', #37312, 0.1000000000000000056 ) ;
#93738 = DIRECTION ( 'NONE',  ( 0.000000000000000000, 0.000000000000000000, 1.000000000000000000 ) ) ;
#93739 = VERTEX_POINT ( 'NONE', #24113 ) ;
#93741 = ORIENTED_EDGE ( 'NONE', *, *, #97547, .F. ) ;
#93740 = CIRCLE ( 'NONE', #118771, 0.06509327318403745899 ) ;
#93742 = ORIENTED_EDGE ( 'NONE', *, *, #35976, .T. ) ;
#93743 = DIRECTION ( 'NONE',  ( 0.000000000000000000, 0.000000000000000000, -1.000000000000000000 ) ) ;
#93744 = EDGE_LOOP ( 'NONE', ( #5900, #22215 ) ) ;
#93746 = ORIENTED_EDGE ( 'NONE', *, *, #68774, .T. ) ;
#93745 = ORIENTED_EDGE ( 'NONE', *, *, #124203, .T. ) ;
#93747 = ORIENTED_EDGE ( 'NONE', *, *, #88459, .F. ) ;
#93748 = AXIS2_PLACEMENT_3D ( 'NONE', #112726, #23051, #14493 ) ;
#93749 = DIRECTION ( 'NONE',  ( 0.000000000000000000, -0.000000000000000000, 1.000000000000000000 ) ) ;
#93750 = FACE_OUTER_BOUND ( 'NONE', #5730, .T. ) ;
#93751 = FILL_AREA_STYLE ('',( #25638 ) ) ;
#93752 = CARTESIAN_POINT ( 'NONE',  ( 5.399999999999932854, 2.500000000000000000, 3.637306695894644726 ) ) ;
#93753 = DIRECTION ( 'NONE',  ( 0.000000000000000000, -0.9999939076577903929, 0.003490651415223739937 ) ) ;
#93754 = LINE ( 'NONE', #83918, #60089 ) ;
#93755 = CIRCLE ( 'NONE', #58167, 0.1000000000000000472 ) ;
#93756 = EDGE_LOOP ( 'NONE', ( #93587, #56381, #113587, #52752 ) ) ;
#93757 = DIRECTION ( 'NONE',  ( 0.000000000000000000, 0.000000000000000000, 1.000000000000000000 ) ) ;
#93758 = VERTEX_POINT ( 'NONE', #64035 ) ;
#93760 = CIRCLE ( 'NONE', #47789, 0.06509327318403745899 ) ;
#93759 = AXIS2_PLACEMENT_3D ( 'NONE', #84916, #94729, #65259 ) ;
#93761 = ORIENTED_EDGE ( 'NONE', *, *, #80209, .T. ) ;
#93762 = ORIENTED_EDGE ( 'NONE', *, *, #13503, .T. ) ;
#93763 = CARTESIAN_POINT ( 'NONE',  ( -14.99999999999998224, 2.500000000000000000, -0.6928203230275519209 ) ) ;
#93764 =( BOUNDED_SURFACE ( )  B_SPLINE_SURFACE ( 3, 2, ( 
 ( #32681, #62123, #45066 ),
 ( #84965, #124897, #22207 ),
 ( #112508, #12985, #74508 ),
 ( #72585, #52938, #43143 ),
 ( #83053, #33315, #73224 ),
 ( #43780, #24123, #73859 ),
 ( #33943, #113138, #113795 ),
 ( #64044, #103974, #4442 ),
 ( #94144, #17500, #97366 ),
 ( #26056, #116986, #106536 ),
 ( #37803, #37175, #35875 ),
 ( #55519, #86239, #85609 ),
 ( #77710, #8332, #48266 ),
 ( #88162, #95441, #127478 ),
 ( #98003, #115707, #46992 ),
 ( #67222, #46328, #16205 ) ),
 .UNSPECIFIED., .F., .F., .F. ) 
 B_SPLINE_SURFACE_WITH_KNOTS ( ( 4, 2, 2, 2, 2, 2, 2, 4 ),
 ( 3, 3 ),
 ( 0.000000000000000000, 0.003502803217043997872, 0.007005606434087995743, 0.008757008042609995546, 0.01050840965113199361, 0.01225981125965399168, 0.01313551206391499158, 0.01401121286817599149 ),
 ( 0.000000000000000000, 1.000000000000000000 ),
 .UNSPECIFIED. ) 
 GEOMETRIC_REPRESENTATION_ITEM ( )  RATIONAL_B_SPLINE_SURFACE ( (
 ( 1.000000000000000000, 0.7071067811865476838, 1.000000000000000000),
 ( 1.000000000000000000, 0.7071067811865476838, 1.000000000000000000),
 ( 1.000000000000000000, 0.7071067811865474617, 1.000000000000000000),
 ( 1.000000000000000000, 0.7071067811865474617, 1.000000000000000000),
 ( 1.000000000000000000, 0.7071067811865477948, 1.000000000000000000),
 ( 1.000000000000000000, 0.7071067811865477948, 1.000000000000000000),
 ( 1.000000000000000000, 0.7071067811865473507, 1.000000000000000000),
 ( 1.000000000000000000, 0.7071067811865473507, 1.000000000000000000),
 ( 1.000000000000000000, 0.7071067811865472397, 1.000000000000000000),
 ( 1.000000000000000000, 0.7071067811865472397, 1.000000000000000000),
 ( 1.000000000000000000, 0.7071067811865473507, 1.000000000000000000),
 ( 1.000000000000000000, 0.7071067811865473507, 1.000000000000000000),
 ( 1.000000000000000000, 0.7071067811865472397, 1.000000000000000000),
 ( 1.000000000000000000, 0.7071067811865472397, 1.000000000000000000),
 ( 1.000000000000000000, 0.7071067811865479058, 1.000000000000000000),
 ( 1.000000000000000000, 0.7071067811865479058, 1.000000000000000000) ) ) 
 REPRESENTATION_ITEM ( '' )  SURFACE ( )  );
#93765 = ORIENTED_EDGE ( 'NONE', *, *, #75285, .T. ) ;
#93766 = ORIENTED_EDGE ( 'NONE', *, *, #51786, .T. ) ;
#93767 = EDGE_LOOP ( 'NONE', ( #41173, #120231, #126673, #8803 ) ) ;
#93768 = PLANE ( 'NONE',  #88430 ) ;
#93769 = CARTESIAN_POINT ( 'NONE',  ( -6.450000000000014388, 2.500000000000000000, 1.818653347947321475 ) ) ;
#93770 = DIRECTION ( 'NONE',  ( -4.274815082592931898E-19, -0.9999939076577903929, -0.003490651415223739937 ) ) ;
#93771 = DIRECTION ( 'NONE',  ( 0.000000000000000000, 1.000000000000000000, 0.000000000000000000 ) ) ;
#93772 = FACE_OUTER_BOUND ( 'NONE', #65880, .T. ) ;
#93773 = EDGE_CURVE ( 'NONE', #4955, #103364, #29949, .T. ) ;
#93775 = VECTOR ( 'NONE', #11098, 1000.000000000000000 ) ;
#93774 = DIRECTION ( 'NONE',  ( 0.000000000000000000, -0.9999939076577903929, 0.003490651415223739937 ) ) ;
#93776 = EDGE_CURVE ( 'NONE', #127507, #116228, #45691, .T. ) ;
#93777 = EDGE_CURVE ( 'NONE', #55129, #89331, #101043, .T. ) ;
#93778 = DIRECTION ( 'NONE',  ( 0.000000000000000000, -0.9999939076577903929, 0.003490651415223739937 ) ) ;
#93779 = ORIENTED_EDGE ( 'NONE', *, *, #91944, .F. ) ;
#93781 = CARTESIAN_POINT ( 'NONE',  ( -12.89999999999999325, 12.50000000000000000, -3.637306695894647390 ) ) ;
#93780 = CONICAL_SURFACE ( 'NONE', #5916, 0.09999999999999982514, 0.003490658503988666988 ) ;
#93783 = EDGE_LOOP ( 'NONE', ( #38339, #38895, #94462, #202 ) ) ;
#93782 = CIRCLE ( 'NONE', #62489, 0.09999999999999999167 ) ;
#93784 = DIRECTION ( 'NONE',  ( 0.000000000000000000, 0.000000000000000000, 1.000000000000000000 ) ) ;
#93785 = VECTOR ( 'NONE', #81048, 1000.000000000000000 ) ;
#93786 = ADVANCED_FACE ( 'NONE', ( #6364 ), #40426, .T. ) ;
#93788 = ORIENTED_EDGE ( 'NONE', *, *, #39800, .T. ) ;
#93787 = EDGE_CURVE ( 'NONE', #34238, #8778, #18786, .T. ) ;
#93789 = ORIENTED_EDGE ( 'NONE', *, *, #53088, .T. ) ;
#93791 = CARTESIAN_POINT ( 'NONE',  ( -1.700000000000034817, 2.500000000000000000, -4.330127018922201643 ) ) ;
#93790 = AXIS2_PLACEMENT_3D ( 'NONE', #72345, #110317, #82151 ) ;
#93792 = DIRECTION ( 'NONE',  ( -4.274815082592931898E-19, -0.9999939076577903929, -0.003490651415223739937 ) ) ;
#93794 = ADVANCED_FACE ( 'NONE', ( #7671 ), #21630, .T. ) ;
#93793 = AXIS2_PLACEMENT_3D ( 'NONE', #83150, #123065, #104690 ) ;
#93795 = AXIS2_PLACEMENT_3D ( 'NONE', #106476, #56077, #14842 ) ;
#93796 = ADVANCED_FACE ( 'NONE', ( #17490 ), #124022, .T. ) ;
#93797 = PLANE ( 'NONE',  #92495 ) ;
#93798 = ORIENTED_EDGE ( 'NONE', *, *, #100673, .F. ) ;
#93799 = ORIENTED_EDGE ( 'NONE', *, *, #127724, .T. ) ;
#93800 = DIRECTION ( 'NONE',  ( -0.000000000000000000, 1.000000000000000000, -0.000000000000000000 ) ) ;
#93801 = DIRECTION ( 'NONE',  ( 0.000000000000000000, -0.9999939076577903929, 0.003490651415223739937 ) ) ;
#93802 = DIRECTION ( 'NONE',  ( 0.000000000000000000, 1.000000000000000000, 0.000000000000000000 ) ) ;
#93803 = DIRECTION ( 'NONE',  ( 0.000000000000000000, -0.000000000000000000, 1.000000000000000000 ) ) ;
#93804 = EDGE_CURVE ( 'NONE', #99888, #43212, #57122, .T. ) ;
#93805 = AXIS2_PLACEMENT_3D ( 'NONE', #99165, #67760, #107692 ) ;
#93806 = DIRECTION ( 'NONE',  ( 0.000000000000000000, -0.000000000000000000, 1.000000000000000000 ) ) ;
#93807 = VECTOR ( 'NONE', #115840, 1000.000000000000000 ) ;
#93808 = ORIENTED_EDGE ( 'NONE', *, *, #31272, .T. ) ;
#93809 = ORIENTED_EDGE ( 'NONE', *, *, #46021, .T. ) ;
#93810 = DIRECTION ( 'NONE',  ( 0.000000000000000000, 0.000000000000000000, -1.000000000000000000 ) ) ;
#93812 = CONICAL_SURFACE ( 'NONE', #31134, 0.1000000000000002554, 0.003490658503988666988 ) ;
#93811 = DIRECTION ( 'NONE',  ( 0.000000000000000000, 0.000000000000000000, 1.000000000000000000 ) ) ;
#93813 = AXIS2_PLACEMENT_3D ( 'NONE', #72079, #110060, #11840 ) ;
#93814 = CARTESIAN_POINT ( 'NONE',  ( 185.6302083336747444, -4.367472073101514418, -7.564683531250002702 ) ) ;
#93815 = FACE_OUTER_BOUND ( 'NONE', #11831, .T. ) ;
#93816 = DIRECTION ( 'NONE',  ( 0.000000000000000000, -0.000000000000000000, 1.000000000000000000 ) ) ;
#93817 = DIRECTION ( 'NONE',  ( 0.000000000000000000, -0.000000000000000000, 1.000000000000000000 ) ) ;
#93818 = DIRECTION ( 'NONE',  ( 0.000000000000000000, 1.000000000000000000, 0.000000000000000000 ) ) ;
#93819 = ORIENTED_EDGE ( 'NONE', *, *, #67748, .F. ) ;
#93820 = DIRECTION ( 'NONE',  ( 0.000000000000000000, -0.000000000000000000, 1.000000000000000000 ) ) ;
#93821 = DIRECTION ( 'NONE',  ( 0.000000000000000000, 0.000000000000000000, 1.000000000000000000 ) ) ;
#93822 = DIRECTION ( 'NONE',  ( 0.000000000000000000, 0.000000000000000000, -1.000000000000000000 ) ) ;
#93823 = CIRCLE ( 'NONE', #118943, 0.1000000000000002554 ) ;
#93824 = ORIENTED_EDGE ( 'NONE', *, *, #109997, .T. ) ;
#93825 = CIRCLE ( 'NONE', #16432, 0.06509327318403745899 ) ;
#93826 = CARTESIAN_POINT ( 'NONE',  ( 11.89999999999990798, 12.50000000000000000, 4.741630453620009789 ) ) ;
#93827 = AXIS2_PLACEMENT_3D ( 'NONE', #102817, #13142, #53096 ) ;
#93828 = EDGE_CURVE ( 'NONE', #22216, #78336, #21720, .T. ) ;
#93829 = ORIENTED_EDGE ( 'NONE', *, *, #1749, .F. ) ;
#93830 = DIRECTION ( 'NONE',  ( 0.000000000000000000, 0.000000000000000000, -1.000000000000000000 ) ) ;
#93831 = ORIENTED_EDGE ( 'NONE', *, *, #63280, .T. ) ;
#93833 = VECTOR ( 'NONE', #15965, 1000.000000000000000 ) ;
#93832 = CARTESIAN_POINT ( 'NONE',  ( 5.399999999999935518, 2.500000000000000000, -4.430127018922202176 ) ) ;
#93834 = DIRECTION ( 'NONE',  ( -0.000000000000000000, -1.000000000000000000, -0.000000000000000000 ) ) ;
#93835 = CARTESIAN_POINT ( 'NONE',  ( 13.14999999999990088, 2.500000000000000000, 2.511473670974873507 ) ) ;
#93836 = VERTEX_POINT ( 'NONE', #47620 ) ;
#93837 = CARTESIAN_POINT ( 'NONE',  ( -10.85000000000000142, 2.500000000000000000, -1.572243186433546214 ) ) ;
#93839 = AXIS2_PLACEMENT_3D ( 'NONE', #129604, #120410, #71287 ) ;
#93838 = AXIS2_PLACEMENT_3D ( 'NONE', #90395, #70143, #736 ) ;
#93840 = DIRECTION ( 'NONE',  ( 0.000000000000000000, 1.000000000000000000, 0.000000000000000000 ) ) ;
#93841 = CONICAL_SURFACE ( 'NONE', #125148, 0.1000000000000002554, 0.003490658503988666988 ) ;
#93842 = VERTEX_POINT ( 'NONE', #108458 ) ;
#93843 = DIRECTION ( 'NONE',  ( 0.000000000000000000, 0.000000000000000000, -1.000000000000000000 ) ) ;
#93845 = CIRCLE ( 'NONE', #114761, 0.06509327318403745899 ) ;
#93844 = CONICAL_SURFACE ( 'NONE', #100205, 0.1000000000000000472, 0.003490658503988666988 ) ;
#93846 = ORIENTED_EDGE ( 'NONE', *, *, #48638, .T. ) ;
#93847 = VERTEX_POINT ( 'NONE', #98626 ) ;
#93848 = FACE_OUTER_BOUND ( 'NONE', #63214, .T. ) ;
#93849 = CARTESIAN_POINT ( 'NONE',  ( -13.74999999999998934, 2.500000000000000000, 2.857883832488652853 ) ) ;
#93850 = CARTESIAN_POINT ( 'NONE',  ( -3.550000000000027800, 2.500000000000000000, 6.148780366869520009 ) ) ;
#93851 = VERTEX_POINT ( 'NONE', #28629 ) ;
#93852 = CARTESIAN_POINT ( 'NONE',  ( 13.34999999999989662, 2.500000000000000000, -2.265063509461101798 ) ) ;
#93853 = CARTESIAN_POINT ( 'NONE',  ( -0.8500000000000386136, 12.50000000000000000, 7.188010851410848723 ) ) ;
#93854 = ORIENTED_EDGE ( 'NONE', *, *, #57893, .F. ) ;
#93855 = DIRECTION ( 'NONE',  ( 0.000000000000000000, 0.000000000000000000, -1.000000000000000000 ) ) ;
#93856 = DIRECTION ( 'NONE',  ( 0.000000000000000000, 0.000000000000000000, 1.000000000000000000 ) ) ;
#93857 = DIRECTION ( 'NONE',  ( 0.000000000000000000, -0.9999939076577903929, 0.003490651415223739937 ) ) ;
#93858 = DIRECTION ( 'NONE',  ( -0.000000000000000000, -1.000000000000000000, -0.000000000000000000 ) ) ;
#93859 = VECTOR ( 'NONE', #114465, 1000.000000000000000 ) ;
#93860 = FACE_OUTER_BOUND ( 'NONE', #931, .T. ) ;
#93861 = DIRECTION ( 'NONE',  ( 0.000000000000000000, 0.000000000000000000, 1.000000000000000000 ) ) ;
#93862 = DIRECTION ( 'NONE',  ( 0.000000000000000000, 0.000000000000000000, 1.000000000000000000 ) ) ;
#93863 = AXIS2_PLACEMENT_3D ( 'NONE', #36014, #56913, #4577 ) ;
#93864 = ADVANCED_FACE ( 'NONE', ( #87525 ), #116977, .T. ) ;
#93865 = AXIS2_PLACEMENT_3D ( 'NONE', #87017, #37290, #17625 ) ;
#93866 = ORIENTED_EDGE ( 'NONE', *, *, #84737, .F. ) ;
#93867 = ORIENTED_EDGE ( 'NONE', *, *, #16112, .T. ) ;
#93868 = ORIENTED_EDGE ( 'NONE', *, *, #127978, .T. ) ;
#93869 = VERTEX_POINT ( 'NONE', #38457 ) ;
#93870 = DIRECTION ( 'NONE',  ( 0.000000000000000000, -0.9999939076577903929, 0.003490651415223739937 ) ) ;
#93871 = PLANE ( 'NONE',  #74971 ) ;
#93872 = LINE ( 'NONE', #23854, #23808 ) ;
#93873 = VERTEX_POINT ( 'NONE', #126822 ) ;
#93874 = EDGE_CURVE ( 'NONE', #2220, #61588, #55171, .T. ) ;
#93875 = FACE_BOUND ( 'NONE', #21346, .T. ) ;
#93876 = ADVANCED_FACE ( 'NONE', ( #77702 ), #44417, .T. ) ;
#93877 = CARTESIAN_POINT ( 'NONE',  ( -3.150000000000030109, 12.50000000000000000, -2.446380397790840266 ) ) ;
#93878 = LINE ( 'NONE', #14647, #104400 ) ;
#93879 = CONICAL_SURFACE ( 'NONE', #95926, 0.1000000000000002554, 0.003490658503988666988 ) ;
#93880 = AXIS2_PLACEMENT_3D ( 'NONE', #96809, #37896, #36633 ) ;
#93881 = DIRECTION ( 'NONE',  ( 0.000000000000000000, 1.000000000000000000, 0.000000000000000000 ) ) ;
#93882 = VECTOR ( 'NONE', #18402, 1000.000000000000000 ) ;
#93883 = DIRECTION ( 'NONE',  ( -0.000000000000000000, 1.000000000000000000, -0.000000000000000000 ) ) ;
#93884 = DIRECTION ( 'NONE',  ( 0.000000000000000000, -0.000000000000000000, 1.000000000000000000 ) ) ;
#93885 = EDGE_CURVE ( 'NONE', #124646, #32011, #118282, .T. ) ;
#93886 = DIRECTION ( 'NONE',  ( 0.000000000000000000, 0.000000000000000000, -1.000000000000000000 ) ) ;
#93887 = EDGE_CURVE ( 'NONE', #47249, #948, #128345, .T. ) ;
#93888 = FACE_OUTER_BOUND ( 'NONE', #80218, .T. ) ;
#93889 = CARTESIAN_POINT ( 'NONE',  ( -6.900000000000019007, 12.50000000000000000, -3.983716857408426293 ) ) ;
#93890 = EDGE_CURVE ( 'NONE', #38209, #96649, #46318, .T. ) ;
#93891 = CARTESIAN_POINT ( 'NONE',  ( 2.949999999999946887, 2.500000000000000000, -6.395190528383301931 ) ) ;
#93892 = ADVANCED_FACE ( 'NONE', ( #79025 ), #26687, .T. ) ;
#93893 = EDGE_CURVE ( 'NONE', #87565, #77368, #13289, .T. ) ;
#93894 = CIRCLE ( 'NONE', #52126, 0.06509327318403745899 ) ;
#93895 = CARTESIAN_POINT ( 'NONE',  ( 9.399999999999918643, 2.500000000000000000, 0.4464101615137736623 ) ) ;
#93896 = VERTEX_POINT ( 'NONE', #58090 ) ;
#93897 = CIRCLE ( 'NONE', #37471, 0.1000000000000002554 ) ;
#93898 = ORIENTED_EDGE ( 'NONE', *, *, #116504, .T. ) ;
#93899 = VERTEX_POINT ( 'NONE', #46984 ) ;
#93900 = ORIENTED_EDGE ( 'NONE', *, *, #13126, .F. ) ;
#93901 = EDGE_LOOP ( 'NONE', ( #863, #123052 ) ) ;
#93902 = EDGE_LOOP ( 'NONE', ( #40267, #121862, #98357, #37046 ) ) ;
#93903 = PLANE ( 'NONE',  #94566 ) ;
#93904 = EDGE_LOOP ( 'NONE', ( #58095, #8116 ) ) ;
#93905 = ADVANCED_FACE ( 'NONE', ( #106527 ), #44712, .T. ) ;
#93906 = EDGE_LOOP ( 'NONE', ( #122018, #98208 ) ) ;
#93907 = EDGE_CURVE ( 'NONE', #30951, #72795, #117834, .T. ) ;
#93908 = CARTESIAN_POINT ( 'NONE',  ( 12.07106445339097256, -1.499999999999809264, 8.629160868130600903 ) ) ;
#93909 = DIRECTION ( 'NONE',  ( -0.000000000000000000, -1.000000000000000000, -0.000000000000000000 ) ) ;
#93910 = DIRECTION ( 'NONE',  ( 0.000000000000000000, 1.000000000000000000, 0.000000000000000000 ) ) ;
#93911 = AXIS2_PLACEMENT_3D ( 'NONE', #75528, #45459, #125295 ) ;
#93912 = ORIENTED_EDGE ( 'NONE', *, *, #113067, .F. ) ;
#93913 = LINE ( 'NONE', #97608, #82042 ) ;
#93914 = ORIENTED_EDGE ( 'NONE', *, *, #67389, .T. ) ;
#93915 = ORIENTED_EDGE ( 'NONE', *, *, #104377, .F. ) ;
#93917 = ORIENTED_EDGE ( 'NONE', *, *, #39793, .T. ) ;
#93916 = CARTESIAN_POINT ( 'NONE',  ( -5.450000000000019718, 2.500000000000000000, 2.265063509461097357 ) ) ;
#93918 = DIRECTION ( 'NONE',  ( 0.000000000000000000, -0.000000000000000000, 1.000000000000000000 ) ) ;
#93919 = VERTEX_POINT ( 'NONE', #80950 ) ;
#93920 = AXIS2_PLACEMENT_3D ( 'NONE', #93136, #42767, #82678 ) ;
#93921 = CARTESIAN_POINT ( 'NONE',  ( -6.250000000000015987, 2.500000000000000000, 5.702370205355745014 ) ) ;
#93922 = CARTESIAN_POINT ( 'NONE',  ( -12.89999999999999147, 2.500000000000000000, -4.330127018922198978 ) ) ;
#93923 = DIRECTION ( 'NONE',  ( 0.000000000000000000, 0.000000000000000000, -1.000000000000000000 ) ) ;
#93924 = LINE ( 'NONE', #44171, #102686 ) ;
#93925 = CARTESIAN_POINT ( 'NONE',  ( -13.34999999999999076, 12.50000000000000000, -2.922977105672689202 ) ) ;
#93926 = ADVANCED_FACE ( 'NONE', ( #111694 ), #119916, .T. ) ;
#93927 = VERTEX_POINT ( 'NONE', #31850 ) ;
#93928 = EDGE_CURVE ( 'NONE', #122474, #89282, #71771, .T. ) ;
#93929 = CARTESIAN_POINT ( 'NONE',  ( -7.950000000000012612, 2.500000000000000000, -2.065063509461102065 ) ) ;
#93930 = ORIENTED_EDGE ( 'NONE', *, *, #68631, .T. ) ;
#93932 = EDGE_CURVE ( 'NONE', #65807, #119406, #15144, .T. ) ;
#93931 = CARTESIAN_POINT ( 'NONE',  ( -3.350000000000032507, 2.500000000000000000, -6.395190528383301931 ) ) ;
#93934 = AXIS2_PLACEMENT_3D ( 'NONE', #14143, #82266, #94637 ) ;
#93933 = AXIS2_PLACEMENT_3D ( 'NONE', #77058, #8301, #88806 ) ;
#93935 = EDGE_LOOP ( 'NONE', ( #5393, #73846, #67400, #12304 ) ) ;
#93936 = DIRECTION ( 'NONE',  ( 0.000000000000000000, 0.000000000000000000, -1.000000000000000000 ) ) ;
#93937 = CARTESIAN_POINT ( 'NONE',  ( 8.749999999999953815, 2.500000000000000000, -2.265063509461101798 ) ) ;
#93938 = CIRCLE ( 'NONE', #31168, 0.06509327318403745899 ) ;
#93939 = DIRECTION ( 'NONE',  ( 0.000000000000000000, 0.000000000000000000, 1.000000000000000000 ) ) ;
#93940 = EDGE_CURVE ( 'NONE', #121539, #41830, #20093, .T. ) ;
#93941 = FACE_OUTER_BOUND ( 'NONE', #113574, .T. ) ;
#93942 = ORIENTED_EDGE ( 'NONE', *, *, #69098, .F. ) ;
#93943 = EDGE_CURVE ( 'NONE', #13400, #125465, #71908, .T. ) ;
#93945 = CONICAL_SURFACE ( 'NONE', #18719, 0.09999999999999982514, 0.003490658503988666988 ) ;
#93944 = CONICAL_SURFACE ( 'NONE', #87662, 0.09999999999999999167, 0.003490658503988666988 ) ;
#93946 = EDGE_CURVE ( 'NONE', #50900, #103695, #123820, .T. ) ;
#93947 = DIRECTION ( 'NONE',  ( -0.000000000000000000, 1.000000000000000000, -0.000000000000000000 ) ) ;
#93948 = ORIENTED_EDGE ( 'NONE', *, *, #113877, .T. ) ;
#93949 = ORIENTED_EDGE ( 'NONE', *, *, #127487, .F. ) ;
#93950 = ORIENTED_EDGE ( 'NONE', *, *, #17941, .F. ) ;
#93951 = DIRECTION ( 'NONE',  ( 0.000000000000000000, 0.000000000000000000, 1.000000000000000000 ) ) ;
#93952 = CARTESIAN_POINT ( 'NONE',  ( 195.5000000000000000, 0.000000000000000000, 0.000000000000000000 ) ) ;
#93953 = CARTESIAN_POINT ( 'NONE',  ( 186.5677083336747160, -4.367472073101514418, -7.564683531250002702 ) ) ;
#93954 = DIRECTION ( 'NONE',  ( -4.274815082592931898E-19, -0.9999939076577903929, -0.003490651415223739937 ) ) ;
#93955 = EDGE_CURVE ( 'NONE', #87480, #6221, #96917, .T. ) ;
#93956 = FACE_OUTER_BOUND ( 'NONE', #546, .T. ) ;
#93957 = CARTESIAN_POINT ( 'NONE',  ( 12.04999999999990479, 2.500000000000000000, -6.495190528383302464 ) ) ;
#93958 = ORIENTED_EDGE ( 'NONE', *, *, #107516, .F. ) ;
#93959 = PLANE ( 'NONE',  #119548 ) ;
#93960 = AXIS2_PLACEMENT_3D ( 'NONE', #21527, #102023, #12965 ) ;
#93961 = AXIS2_PLACEMENT_3D ( 'NONE', #33904, #124864, #73820 ) ;
#93962 = ORIENTED_EDGE ( 'NONE', *, *, #87929, .F. ) ;
#93963 = CARTESIAN_POINT ( 'NONE',  ( 6.899999999999928413, 12.50000000000000000, -3.983716857408426293 ) ) ;
#93964 = DIRECTION ( 'NONE',  ( 0.000000000000000000, 0.000000000000000000, -1.000000000000000000 ) ) ;
#93965 = EDGE_CURVE ( 'NONE', #7088, #9874, #4677, .T. ) ;
#93966 = DIRECTION ( 'NONE',  ( 0.000000000000000000, 1.000000000000000000, 0.000000000000000000 ) ) ;
#93967 = DIRECTION ( 'NONE',  ( -4.274815082592931898E-19, -0.9999939076577903929, -0.003490651415223739937 ) ) ;
#93968 = CONICAL_SURFACE ( 'NONE', #125356, 0.09999999999999982514, 0.003490658503988666988 ) ;
#93969 = ORIENTED_EDGE ( 'NONE', *, *, #85583, .F. ) ;
#93970 = VECTOR ( 'NONE', #110349, 1000.000000000000000 ) ;
#93971 = AXIS2_PLACEMENT_3D ( 'NONE', #95526, #56229, #25475 ) ;
#93972 = CARTESIAN_POINT ( 'NONE',  ( 12.04999999999990834, 12.50000000000000000, -2.230156782645139391 ) ) ;
#93974 = ORIENTED_EDGE ( 'NONE', *, *, #86570, .T. ) ;
#93973 = FACE_OUTER_BOUND ( 'NONE', #84796, .T. ) ;
#93975 = AXIS2_PLACEMENT_3D ( 'NONE', #16551, #56482, #6719 ) ;
#93976 = VERTEX_POINT ( 'NONE', #119562 ) ;
#93977 = CYLINDRICAL_SURFACE ( 'NONE', #17509, 8.699999999999999289 ) ;
#93978 = VECTOR ( 'NONE', #111505, 1000.000000000000000 ) ;
#93979 = CIRCLE ( 'NONE', #87706, 2.250000000000001776 ) ;
#93980 = EDGE_CURVE ( 'NONE', #102949, #35583, #111602, .T. ) ;
#93981 = ORIENTED_EDGE ( 'NONE', *, *, #87266, .T. ) ;
#93982 = ORIENTED_EDGE ( 'NONE', *, *, #98280, .F. ) ;
#93983 = DIRECTION ( 'NONE',  ( -0.000000000000000000, 1.000000000000000000, -0.000000000000000000 ) ) ;
#93984 = ORIENTED_EDGE ( 'NONE', *, *, #90635, .T. ) ;
#93985 = DIRECTION ( 'NONE',  ( 0.000000000000000000, 1.000000000000000000, 0.000000000000000000 ) ) ;
#93986 = FACE_OUTER_BOUND ( 'NONE', #6114, .T. ) ;
#93987 = DIRECTION ( 'NONE',  ( 0.000000000000000000, 1.000000000000000000, 0.000000000000000000 ) ) ;
#93988 = VERTEX_POINT ( 'NONE', #19428 ) ;
#93989 = CARTESIAN_POINT ( 'NONE',  ( 9.799999999999915445, 2.500000000000000000, -4.776537180435977525 ) ) ;
#93991 = ORIENTED_EDGE ( 'NONE', *, *, #39993, .F. ) ;
#93990 = CARTESIAN_POINT ( 'NONE',  ( -3.300000000000027800, 12.50000000000000000, -4.330127018922201643 ) ) ;
#93992 = CIRCLE ( 'NONE', #110703, 0.06509327318403745899 ) ;
#93993 = DIRECTION ( 'NONE',  ( -4.274815082592931898E-19, -0.9999939076577903929, -0.003490651415223739937 ) ) ;
#93994 = ADVANCED_FACE ( 'NONE', ( #101227 ), #15433, .T. ) ;
#93995 = CARTESIAN_POINT ( 'NONE',  ( -9.150000000000011013, 12.50000000000000000, -5.737276932171707422 ) ) ;
#93996 = EDGE_LOOP ( 'NONE', ( #116008, #50035 ) ) ;
#93997 = VERTEX_POINT ( 'NONE', #12179 ) ;
#93998 = VERTEX_POINT ( 'NONE', #109763 ) ;
#93999 = DIRECTION ( 'NONE',  ( 0.000000000000000000, -0.9999939076577903929, 0.003490651415223739937 ) ) ;
#94000 = CARTESIAN_POINT ( 'NONE',  ( 3.749999999999940492, 2.500000000000000000, 2.757883832488649656 ) ) ;
#94001 = CARTESIAN_POINT ( 'NONE',  ( 4.349999999999940137, 2.500000000000000000, -6.741600689897078169 ) ) ;
#94002 = FACE_BOUND ( 'NONE', #95632, .T. ) ;
#94003 = ORIENTED_EDGE ( 'NONE', *, *, #66722, .T. ) ;
#94004 = CARTESIAN_POINT ( 'NONE',  ( 186.4010416670080588, -4.367472073101519747, 7.564683531249999149 ) ) ;
#94005 = CARTESIAN_POINT ( 'NONE',  ( 6.249999999999930722, 2.500000000000000000, 1.372243186433545370 ) ) ;
#94006 = DIRECTION ( 'NONE',  ( -0.000000000000000000, 1.000000000000000000, -0.000000000000000000 ) ) ;
#94007 = LINE ( 'NONE', #42340, #54742 ) ;
#94008 = CARTESIAN_POINT ( 'NONE',  ( -1.650000000000034328, 2.500000000000000000, -2.957883832488653830 ) ) ;
#94009 = CIRCLE ( 'NONE', #85691, 0.06509327318403745899 ) ;
#94010 = FACE_OUTER_BOUND ( 'NONE', #127409, .T. ) ;
#94011 = CARTESIAN_POINT ( 'NONE',  ( 0.5999999999999621192, 2.500000000000000000, 0.3464101615137758494 ) ) ;
#94012 = ADVANCED_FACE ( 'NONE', ( #59396 ), #66975, .T. ) ;
#94014 = CIRCLE ( 'NONE', #54313, 0.06509327318403745899 ) ;
#94013 = CIRCLE ( 'NONE', #68976, 0.09999999999999982514 ) ;
#94015 = VERTEX_POINT ( 'NONE', #112975 ) ;
#94016 = ORIENTED_EDGE ( 'NONE', *, *, #129252, .F. ) ;
#94017 = EDGE_LOOP ( 'NONE', ( #110477, #57015, #106234, #8227 ) ) ;
#94018 = VERTEX_POINT ( 'NONE', #102512 ) ;
#94019 = ORIENTED_EDGE ( 'NONE', *, *, #101498, .T. ) ;
#94020 = LINE ( 'NONE', #44268, #61035 ) ;
#94021 = CIRCLE ( 'NONE', #108598, 0.06509327318403741736 ) ;
#94022 = FACE_OUTER_BOUND ( 'NONE', #29532, .T. ) ;
#94023 = ORIENTED_EDGE ( 'NONE', *, *, #46585, .F. ) ;
#94024 = FACE_BOUND ( 'NONE', #107945, .T. ) ;
#94025 = FACE_OUTER_BOUND ( 'NONE', #53465, .T. ) ;
#94026 = EDGE_CURVE ( 'NONE', #13985, #106765, #112338, .T. ) ;
#94028 = CIRCLE ( 'NONE', #56366, 0.1000000000000002554 ) ;
#94027 = AXIS2_PLACEMENT_3D ( 'NONE', #53237, #33597, #43431 ) ;
#94029 = VERTEX_POINT ( 'NONE', #104444 ) ;
#94030 = EDGE_CURVE ( 'NONE', #117860, #90471, #54059, .T. ) ;
#94031 = LINE ( 'NONE', #104491, #83018 ) ;
#94032 = ADVANCED_FACE ( 'NONE', ( #63880 ), #84149, .T. ) ;
#94033 = DIRECTION ( 'NONE',  ( 0.000000000000000000, 1.000000000000000000, 0.000000000000000000 ) ) ;
#94034 = EDGE_CURVE ( 'NONE', #84904, #91963, #52763, .T. ) ;
#94035 = CARTESIAN_POINT ( 'NONE',  ( 4.549999999999939426, 2.500000000000000000, -2.065063509461102065 ) ) ;
#94036 = ADVANCED_FACE ( 'NONE', ( #23294 ), #103189, .T. ) ;
#94037 = ORIENTED_EDGE ( 'NONE', *, *, #22672, .F. ) ;
#94038 = DIRECTION ( 'NONE',  ( -0.000000000000000000, 1.000000000000000000, -0.000000000000000000 ) ) ;
#94039 = ORIENTED_EDGE ( 'NONE', *, *, #70579, .T. ) ;
#94040 = EDGE_CURVE ( 'NONE', #2601, #92856, #4936, .T. ) ;
#94041 = ORIENTED_EDGE ( 'NONE', *, *, #77810, .T. ) ;
#94042 = VERTEX_POINT ( 'NONE', #35081 ) ;
#94043 = CARTESIAN_POINT ( 'NONE',  ( 10.39999999999991154, 12.50000000000000000, 4.957854068765711553 ) ) ;
#94044 = LINE ( 'NONE', #4342, #98572 ) ;
#94045 = DIRECTION ( 'NONE',  ( 0.000000000000000000, 1.000000000000000000, 0.000000000000000000 ) ) ;
#94046 = EDGE_LOOP ( 'NONE', ( #7295, #2284 ) ) ;
#94047 = ADVANCED_FACE ( 'NONE', ( #74988 ), #114897, .T. ) ;
#94048 = CARTESIAN_POINT ( 'NONE',  ( -9.150000000000009237, 2.500000000000000000, 2.757883832488649656 ) ) ;
#94049 = EDGE_CURVE ( 'NONE', #109495, #92601, #80220, .T. ) ;
#94050 = AXIS2_PLACEMENT_3D ( 'NONE', #32982, #102983, #63717 ) ;
#94051 = DIRECTION ( 'NONE',  ( 0.000000000000000000, 0.000000000000000000, 1.000000000000000000 ) ) ;
#94052 = EDGE_CURVE ( 'NONE', #122843, #19850, #33962, .T. ) ;
#94053 = AXIS2_PLACEMENT_3D ( 'NONE', #15300, #106283, #4193 ) ;
#94054 = CARTESIAN_POINT ( 'NONE',  ( 187.0000000000000000, 0.000000000000000000, 7.700000000000000178 ) ) ;
#94055 = CARTESIAN_POINT ( 'NONE',  ( 185.6979166673494603, 6.668395609140176816, 3.850000000000000977 ) ) ;
#94056 = EDGE_LOOP ( 'NONE', ( #121170, #2978 ) ) ;
#94057 = DIRECTION ( 'NONE',  ( 0.000000000000000000, -0.000000000000000000, 1.000000000000000000 ) ) ;
#94058 = ADVANCED_FACE ( 'NONE', ( #3033 ), #92696, .T. ) ;
#94059 = ORIENTED_EDGE ( 'NONE', *, *, #60104, .T. ) ;
#94060 = DIRECTION ( 'NONE',  ( 0.000000000000000000, 0.000000000000000000, -1.000000000000000000 ) ) ;
#94061 = CIRCLE ( 'NONE', #62681, 0.1000000000000002554 ) ;
#94062 = ORIENTED_EDGE ( 'NONE', *, *, #105328, .T. ) ;
#94063 = ORIENTED_EDGE ( 'NONE', *, *, #116502, .F. ) ;
#94064 = DIRECTION ( 'NONE',  ( 0.000000000000000000, 1.000000000000000000, 0.000000000000000000 ) ) ;
#94065 = DIRECTION ( 'NONE',  ( 1.000000000000000000, -0.000000000000000000, -0.000000000000000000 ) ) ;
#94066 = DIRECTION ( 'NONE',  ( -0.000000000000000000, 1.000000000000000000, -0.000000000000000000 ) ) ;
#94067 = CARTESIAN_POINT ( 'NONE',  ( -11.64999999999999680, 2.500000000000000000, -2.165063509461097713 ) ) ;
#94068 = CARTESIAN_POINT ( 'NONE',  ( -9.150000000000009237, 2.500000000000000000, -7.288010851410849256 ) ) ;
#94069 = CONICAL_SURFACE ( 'NONE', #108729, 0.09999999999999982514, 0.003490658503988666988 ) ;
#94070 = EDGE_LOOP ( 'NONE', ( #26397, #21378 ) ) ;
#94071 = VERTEX_POINT ( 'NONE', #13473 ) ;
#94072 = CIRCLE ( 'NONE', #39727, 0.09999999999999982514 ) ;
#94073 = DIRECTION ( 'NONE',  ( 0.000000000000000000, -0.000000000000000000, 1.000000000000000000 ) ) ;
#94074 = AXIS2_PLACEMENT_3D ( 'NONE', #75314, #43941, #84503 ) ;
#94075 = DIRECTION ( 'NONE',  ( -0.000000000000000000, 1.000000000000000000, -0.000000000000000000 ) ) ;
#94076 = CARTESIAN_POINT ( 'NONE',  ( -7.300000000000014921, 2.500000000000000000, 4.576537180435972019 ) ) ;
#94077 = ORIENTED_EDGE ( 'NONE', *, *, #55319, .T. ) ;
#94078 = ORIENTED_EDGE ( 'NONE', *, *, #45290, .F. ) ;
#94079 = AXIS2_PLACEMENT_3D ( 'NONE', #87758, #6594, #18381 ) ;
#94080 = CARTESIAN_POINT ( 'NONE',  ( 7.499999999999923617, 2.500000000000000000, 0.5928203230275495006 ) ) ;
#94081 = CIRCLE ( 'NONE', #102402, 0.06509327318403745899 ) ;
#94082 = ORIENTED_EDGE ( 'NONE', *, *, #36838, .T. ) ;
#94083 = CARTESIAN_POINT ( 'NONE',  ( -1.650000000000035660, 2.500000000000000000, 7.188010851410848723 ) ) ;
#94084 = FACE_OUTER_BOUND ( 'NONE', #17073, .T. ) ;
#94085 = VERTEX_POINT ( 'NONE', #107002 ) ;
#94086 = LINE ( 'NONE', #23397, #98331 ) ;
#94087 = DIRECTION ( 'NONE',  ( 0.000000000000000000, 0.000000000000000000, -1.000000000000000000 ) ) ;
#94088 = AXIS2_PLACEMENT_3D ( 'NONE', #123769, #123150, #33495 ) ;
#94089 = DIRECTION ( 'NONE',  ( 0.000000000000000000, 0.000000000000000000, 1.000000000000000000 ) ) ;
#94090 = DIRECTION ( 'NONE',  ( 0.000000000000000000, -0.000000000000000000, 1.000000000000000000 ) ) ;
#94091 = ORIENTED_EDGE ( 'NONE', *, *, #116484, .T. ) ;
#94092 = EDGE_CURVE ( 'NONE', #122396, #51312, #47463, .T. ) ;
#94093 = FACE_OUTER_BOUND ( 'NONE', #17131, .T. ) ;
#94095 = EDGE_CURVE ( 'NONE', #12403, #1184, #90668, .T. ) ;
#94094 = LINE ( 'NONE', #83640, #81151 ) ;
#94096 = ORIENTED_EDGE ( 'NONE', *, *, #32349, .F. ) ;
#94097 = VERTEX_POINT ( 'NONE', #115534 ) ;
#94098 = CARTESIAN_POINT ( 'NONE',  ( 184.2968750003414300, 8.734944146203032389, 5.348610694689227483E-16 ) ) ;
#94099 = DIRECTION ( 'NONE',  ( -0.000000000000000000, 1.000000000000000000, -0.000000000000000000 ) ) ;
#94100 = DIRECTION ( 'NONE',  ( 0.000000000000000000, 0.000000000000000000, 1.000000000000000000 ) ) ;
#94101 = CARTESIAN_POINT ( 'NONE',  ( 6.699999999999928235, 2.500000000000000000, -0.1000000000000022815 ) ) ;
#94102 = EDGE_CURVE ( 'NONE', #70406, #25375, #84407, .T. ) ;
#94103 = FACE_OUTER_BOUND ( 'NONE', #126968, .T. ) ;
#94104 = DIRECTION ( 'NONE',  ( -0.000000000000000000, -1.000000000000000000, -0.000000000000000000 ) ) ;
#94105 = CARTESIAN_POINT ( 'NONE',  ( -10.20000000000000284, 12.50000000000000000, 3.918623584224383727 ) ) ;
#94106 = LINE ( 'NONE', #33278, #92991 ) ;
#94107 = CARTESIAN_POINT ( 'NONE',  ( -6.900000000000015454, 12.50000000000000000, 4.676537180435972552 ) ) ;
#94108 = CARTESIAN_POINT ( 'NONE',  ( -4.350000000000023626, 12.50000000000000000, 6.148780366869520897 ) ) ;
#94109 = AXIS2_PLACEMENT_3D ( 'NONE', #31789, #101171, #30518 ) ;
#94110 = CARTESIAN_POINT ( 'NONE',  ( 2.899999999999946620, 2.500000000000000000, -0.6928203230275542523 ) ) ;
#94111 = ORIENTED_EDGE ( 'NONE', *, *, #87154, .F. ) ;
#94112 = ORIENTED_EDGE ( 'NONE', *, *, #62731, .T. ) ;
#94114 = AXIS2_PLACEMENT_3D ( 'NONE', #83401, #84018, #61833 ) ;
#94113 = CIRCLE ( 'NONE', #37684, 0.1000000000000002554 ) ;
#94115 = EDGE_LOOP ( 'NONE', ( #18505, #59244 ) ) ;
#94116 = EDGE_LOOP ( 'NONE', ( #108869, #63991 ) ) ;
#94117 = PLANE ( 'NONE',  #12326 ) ;
#94118 = DIRECTION ( 'NONE',  ( 0.000000000000000000, 1.000000000000000000, 0.000000000000000000 ) ) ;
#94119 = DIRECTION ( 'NONE',  ( -4.274815082592931898E-19, -0.9999939076577903929, -0.003490651415223739937 ) ) ;
#94121 = ORIENTED_EDGE ( 'NONE', *, *, #5673, .T. ) ;
#94120 = CIRCLE ( 'NONE', #110740, 0.06509327318403745899 ) ;
#94122 = FACE_OUTER_BOUND ( 'NONE', #55719, .T. ) ;
#94123 = CARTESIAN_POINT ( 'NONE',  ( -4.400000000000028777, 12.50000000000000000, -3.983716857408426293 ) ) ;
#94125 = VERTEX_POINT ( 'NONE', #117448 ) ;
#94124 = CARTESIAN_POINT ( 'NONE',  ( -1.900000000000035438, 12.50000000000000000, 3.918623584224382839 ) ) ;
#94126 = DIRECTION ( 'NONE',  ( 0.000000000000000000, 1.000000000000000000, 0.000000000000000000 ) ) ;
#94127 = DIRECTION ( 'NONE',  ( -1.000000000000000000, -0.000000000000000000, -0.000000000000000000 ) ) ;
#94128 = ORIENTED_EDGE ( 'NONE', *, *, #45454, .T. ) ;
#94129 = VERTEX_POINT ( 'NONE', #75610 ) ;
#94130 = EDGE_LOOP ( 'NONE', ( #41407, #19606, #101723, #17767 ) ) ;
#94131 = ORIENTED_EDGE ( 'NONE', *, *, #64227, .T. ) ;
#94132 = LINE ( 'NONE', #55504, #51043 ) ;
#94133 = CARTESIAN_POINT ( 'NONE',  ( 7.299999999999926104, 2.500000000000000000, 4.776537180435972196 ) ) ;
#94134 = CARTESIAN_POINT ( 'NONE',  ( 6.249999999999967137, 12.50000000000000000, 6.495190528383297135 ) ) ;
#94135 = DIRECTION ( 'NONE',  ( 0.000000000000000000, -0.9999939076577903929, 0.003490651415223739937 ) ) ;
#94136 = AXIS2_PLACEMENT_3D ( 'NONE', #18889, #17597, #127567 ) ;
#94137 = ADVANCED_FACE ( 'NONE', ( #127951 ), #88001, .T. ) ;
#94138 = ORIENTED_EDGE ( 'NONE', *, *, #115148, .F. ) ;
#94139 = CIRCLE ( 'NONE', #20981, 0.06509327318403741736 ) ;
#94140 = PLANE ( 'NONE',  #125449 ) ;
#94142 = VERTEX_POINT ( 'NONE', #46828 ) ;
#94141 = EDGE_CURVE ( 'NONE', #79210, #113203, #67738, .T. ) ;
#94143 = DIRECTION ( 'NONE',  ( 0.000000000000000000, 1.000000000000000000, 0.000000000000000000 ) ) ;
#94144 = CARTESIAN_POINT ( 'NONE',  ( 12.64862127202683872, -1.499999999999935607, -8.430718248283369576 ) ) ;
#94145 = CARTESIAN_POINT ( 'NONE',  ( 11.24999999999990585, 2.500000000000000000, -5.902370205355750521 ) ) ;
#94146 = CARTESIAN_POINT ( 'NONE',  ( 20.37025966759669515, -0.6621301594403563584, 4.188616773932332116 ) ) ;
#94147 = EDGE_CURVE ( 'NONE', #66442, #60131, #77853, .T. ) ;
#94148 = AXIS2_PLACEMENT_3D ( 'NONE', #60823, #50352, #90254 ) ;
#94149 = ORIENTED_EDGE ( 'NONE', *, *, #10657, .F. ) ;
#94150 = ORIENTED_EDGE ( 'NONE', *, *, #97865, .F. ) ;
#94151 = ORIENTED_EDGE ( 'NONE', *, *, #418, .F. ) ;
#94152 = DIRECTION ( 'NONE',  ( 0.000000000000000000, 0.000000000000000000, -1.000000000000000000 ) ) ;
#94153 = CARTESIAN_POINT ( 'NONE',  ( -6.650000000000018119, 2.500000000000000000, -7.188010851410854052 ) ) ;
#94154 = EDGE_CURVE ( 'NONE', #89533, #35730, #37003, .T. ) ;
#94155 = LINE ( 'NONE', #86907, #25200 ) ;
#94156 = FACE_BOUND ( 'NONE', #100777, .T. ) ;
#94157 = DIRECTION ( 'NONE',  ( 0.000000000000000000, 0.000000000000000000, 1.000000000000000000 ) ) ;
#94158 = CARTESIAN_POINT ( 'NONE',  ( -13.34999999999999076, 2.500000000000000000, 2.857883832488652853 ) ) ;
#94159 = DIRECTION ( 'NONE',  ( -0.000000000000000000, 1.000000000000000000, -0.000000000000000000 ) ) ;
#94160 = AXIS2_PLACEMENT_3D ( 'NONE', #54365, #2671, #101541 ) ;
#94161 = CIRCLE ( 'NONE', #92095, 0.06509327318403745899 ) ;
#94162 = B_SPLINE_CURVE_WITH_KNOTS ( 'NONE', 3,
 ( #68253, #60401, #8670, #50542, #49937, #119288, #59096, #80672, #20459, #68900, #108175, #79383, #100309, #120586, #9989, #90462, #108815, #99015, #18515, #89830, #119946, #19135, #48628, #9343, #805, #88539, #28996, #38837, #49290, #89192, #30296, #40764, #30935, #57806, #97718, #53773 ),
 .UNSPECIFIED., .F., .F.,
 ( 4, 2, 2, 2, 2, 2, 2, 2, 2, 2, 2, 2, 2, 2, 2, 2, 2, 4 ),
 ( 0.01599712308563960503, 0.01699497736294824229, 0.01799283164025687956, 0.01899068591756551683, 0.01998854019487415062, 0.02098639447218278789, 0.02198424874949142516, 0.02298210302680006242, 0.02397995730410869969, 0.02447888444276301659, 0.02497781158141733349, 0.02597566585872598116, 0.02697352013603462537, 0.02797137441334326957, 0.02896922869065191725, 0.02996708296796055798, 0.03096493724526920219, 0.03196279152257784639 ),
 .UNSPECIFIED. ) ;
#94163 = CARTESIAN_POINT ( 'NONE',  ( 11.04999999999991012, 2.500000000000000000, -1.918653347947326004 ) ) ;
#94164 = PLANE ( 'NONE',  #121989 ) ;
#94165 = DIRECTION ( 'NONE',  ( -0.000000000000000000, 1.000000000000000000, -0.000000000000000000 ) ) ;
#94166 = VERTEX_POINT ( 'NONE', #6222 ) ;
#94167 = CIRCLE ( 'NONE', #46060, 0.06509327318403745899 ) ;
#94168 = CARTESIAN_POINT ( 'NONE',  ( 6.049999999999935874, 2.500000000000000000, -6.841600689897077814 ) ) ;
#94169 = EDGE_CURVE ( 'NONE', #89954, #19824, #37654, .T. ) ;
#94170 = ORIENTED_EDGE ( 'NONE', *, *, #50888, .T. ) ;
#94171 = AXIS2_PLACEMENT_3D ( 'NONE', #70667, #60232, #121694 ) ;
#94172 = ORIENTED_EDGE ( 'NONE', *, *, #20782, .F. ) ;
#94173 = ORIENTED_EDGE ( 'NONE', *, *, #117200, .F. ) ;
#94174 = ORIENTED_EDGE ( 'NONE', *, *, #98910, .F. ) ;
#94175 = DIRECTION ( 'NONE',  ( 0.000000000000000000, -0.000000000000000000, 1.000000000000000000 ) ) ;
#94176 = FACE_BOUND ( 'NONE', #61022, .T. ) ;
#94177 = DIRECTION ( 'NONE',  ( 0.000000000000000000, 0.000000000000000000, 1.000000000000000000 ) ) ;
#94178 = ADVANCED_FACE ( 'NONE', ( #76921 ), #28474, .T. ) ;
#94179 = ORIENTED_EDGE ( 'NONE', *, *, #20201, .T. ) ;
#94180 = EDGE_CURVE ( 'NONE', #101722, #87021, #27774, .T. ) ;
#94181 = DIRECTION ( 'NONE',  ( 0.000000000000000000, 0.000000000000000000, 1.000000000000000000 ) ) ;
#94182 = ADVANCED_FACE ( 'NONE', ( #107673 ), #17991, .T. ) ;
#94183 = LINE ( 'NONE', #4485, #123017 ) ;
#94184 = ADVANCED_FACE ( 'NONE', ( #57935 ), #46167, .F. ) ;
#94185 = ADVANCED_FACE ( 'NONE', ( #118127 ), #108307, .T. ) ;
#94186 = ORIENTED_EDGE ( 'NONE', *, *, #95685, .T. ) ;
#94187 = CARTESIAN_POINT ( 'NONE',  ( -8.550000000000013145, 2.500000000000000000, -1.818653347947326138 ) ) ;
#94188 = DIRECTION ( 'NONE',  ( 0.000000000000000000, -0.9999939076577903929, 0.003490651415223739937 ) ) ;
#94189 = EDGE_CURVE ( 'NONE', #50586, #35208, #57012, .T. ) ;
#94190 = VECTOR ( 'NONE', #44172, 1000.000000000000000 ) ;
#94191 = ORIENTED_EDGE ( 'NONE', *, *, #38635, .T. ) ;
#94192 = AXIS2_PLACEMENT_3D ( 'NONE', #90551, #70283, #61099 ) ;
#94193 = CARTESIAN_POINT ( 'NONE',  ( 6.449999999999930012, 2.500000000000000000, -1.818653347947326138 ) ) ;
#94194 = AXIS2_PLACEMENT_3D ( 'NONE', #8258, #78321, #39053 ) ;
#94195 = EDGE_CURVE ( 'NONE', #117091, #54998, #34051, .T. ) ;
#94196 = CARTESIAN_POINT ( 'NONE',  ( -3.750000000000031086, 2.500000000000000000, -5.802370205355749988 ) ) ;
#94197 = ADVANCED_FACE ( 'NONE', ( #56612 ), #21526, .T. ) ;
#94198 = EDGE_LOOP ( 'NONE', ( #2917, #1175, #45574, #112492 ) ) ;
#94199 = DIRECTION ( 'NONE',  ( 0.000000000000000000, 0.000000000000000000, -1.000000000000000000 ) ) ;
#94201 = ADVANCED_FACE ( 'NONE', ( #89955 ), #118777, .T. ) ;
#94200 = AXIS2_PLACEMENT_3D ( 'NONE', #40715, #80628, #100263 ) ;
#94202 = CARTESIAN_POINT ( 'NONE',  ( -1.050000000000037792, 12.50000000000000000, 1.818653347947321475 ) ) ;
#94203 = FACE_OUTER_BOUND ( 'NONE', #21985, .T. ) ;
#94204 = ORIENTED_EDGE ( 'NONE', *, *, #82123, .T. ) ;
#94205 = ORIENTED_EDGE ( 'NONE', *, *, #101456, .F. ) ;
#94206 = EDGE_CURVE ( 'NONE', #48754, #67150, #13095, .T. ) ;
#94207 = DIRECTION ( 'NONE',  ( 0.000000000000000000, -0.9999939076577903929, 0.003490651415223739937 ) ) ;
#94208 = ADVANCED_FACE ( 'NONE', ( #29753 ), #119714, .T. ) ;
#94209 = ORIENTED_EDGE ( 'NONE', *, *, #52198, .T. ) ;
#94210 = CARTESIAN_POINT ( 'NONE',  ( -14.34999999999998543, 2.500000000000000000, -1.918653347947323784 ) ) ;
#94211 = CARTESIAN_POINT ( 'NONE',  ( 8.099999999999923261, 2.500000000000000000, -3.983716857408426293 ) ) ;
#94212 = ORIENTED_EDGE ( 'NONE', *, *, #50563, .T. ) ;
#94213 = DIRECTION ( 'NONE',  ( 0.000000000000000000, 0.000000000000000000, 1.000000000000000000 ) ) ;
#94214 = CARTESIAN_POINT ( 'NONE',  ( -6.250000000000017764, 12.50000000000000000, 2.857883832488649301 ) ) ;
#94215 = LINE ( 'NONE', #103400, #102967 ) ;
#94216 = DIRECTION ( 'NONE',  ( -0.000000000000000000, 1.000000000000000000, -0.000000000000000000 ) ) ;
#94217 = DIRECTION ( 'NONE',  ( 0.000000000000000000, 1.000000000000000000, 0.000000000000000000 ) ) ;
#94218 = VERTEX_POINT ( 'NONE', #129273 ) ;
#94219 = ORIENTED_EDGE ( 'NONE', *, *, #40242, .T. ) ;
#94220 = CARTESIAN_POINT ( 'NONE',  ( 11.84999999999990727, 2.500000000000000000, 6.841600689897072485 ) ) ;
#94221 = DIRECTION ( 'NONE',  ( 0.000000000000000000, -0.9999939076577903929, 0.003490651415223739937 ) ) ;
#94222 = CARTESIAN_POINT ( 'NONE',  ( 5.199999999999935341, 2.500000000000000000, -4.083716857408426826 ) ) ;
#94224 = ORIENTED_EDGE ( 'NONE', *, *, #28582, .F. ) ;
#94223 = ORIENTED_EDGE ( 'NONE', *, *, #80567, .F. ) ;
#94225 = EDGE_LOOP ( 'NONE', ( #5095, #15331 ) ) ;
#94226 = CARTESIAN_POINT ( 'NONE',  ( -2.499999999999996003, 2.500000000000000000, 0.09999999999999772959 ) ) ;
#94227 = VECTOR ( 'NONE', #7968, 1000.000000000000000 ) ;
#94228 = DIRECTION ( 'NONE',  ( 0.000000000000000000, -0.000000000000000000, 1.000000000000000000 ) ) ;
#94229 = AXIS2_PLACEMENT_3D ( 'NONE', #18740, #119513, #39059 ) ;
#94230 = DIRECTION ( 'NONE',  ( 0.000000000000000000, 0.000000000000000000, 1.000000000000000000 ) ) ;
#94231 = DIRECTION ( 'NONE',  ( 0.000000000000000000, 0.000000000000000000, 1.000000000000000000 ) ) ;
#94232 = DIRECTION ( 'NONE',  ( 0.000000000000000000, -0.9999939076577903929, 0.003490651415223739937 ) ) ;
#94233 = CARTESIAN_POINT ( 'NONE',  ( 8.549999999999922551, 2.500000000000000000, 2.411473670974873862 ) ) ;
#94234 = CARTESIAN_POINT ( 'NONE',  ( 0.5999999999999547917, 2.500000000000000000, 3.883716857408420431 ) ) ;
#94235 = DIRECTION ( 'NONE',  ( 0.000000000000000000, 0.000000000000000000, 1.000000000000000000 ) ) ;
#94236 = CARTESIAN_POINT ( 'NONE',  ( -4.400000000000025224, 12.50000000000000000, 0.3464101615137735735 ) ) ;
#94238 = CIRCLE ( 'NONE', #4327, 0.1000000000000002554 ) ;
#94237 = DIRECTION ( 'NONE',  ( 0.000000000000000000, -0.000000000000000000, 1.000000000000000000 ) ) ;
#94239 = VECTOR ( 'NONE', #116618, 1000.000000000000000 ) ;
#94240 = EDGE_LOOP ( 'NONE', ( #121485, #74437, #47300, #40376 ) ) ;
#94241 = EDGE_CURVE ( 'NONE', #51418, #117845, #107197, .T. ) ;
#94242 = EDGE_CURVE ( 'NONE', #31947, #24001, #101075, .T. ) ;
#94243 = CARTESIAN_POINT ( 'NONE',  ( 12.09999999999990550, 12.50000000000000000, 4.265033745738159077 ) ) ;
#94244 = EDGE_LOOP ( 'NONE', ( #31697, #101111 ) ) ;
#94245 = EDGE_LOOP ( 'NONE', ( #117923, #52137 ) ) ;
#94246 = DIRECTION ( 'NONE',  ( 0.000000000000000000, -0.9999939076577903929, 0.003490651415223739937 ) ) ;
#94247 = DIRECTION ( 'NONE',  ( 0.000000000000000000, 1.000000000000000000, 0.000000000000000000 ) ) ;
#94248 = CARTESIAN_POINT ( 'NONE',  ( -8.100000000000010303, 2.500000000000000000, 3.883716857408421319 ) ) ;
#94249 = AXIS2_PLACEMENT_3D ( 'NONE', #73852, #33306, #43135 ) ;
#94250 = DIRECTION ( 'NONE',  ( -0.000000000000000000, -1.000000000000000000, -0.000000000000000000 ) ) ;
#94251 = CIRCLE ( 'NONE', #48380, 0.09999999999999999167 ) ;
#94252 = CARTESIAN_POINT ( 'NONE',  ( -5.850000000000022737, 2.500000000000000000, -2.165063509461101710 ) ) ;
#94253 = DIRECTION ( 'NONE',  ( 0.000000000000000000, -0.9999939076577903929, 0.003490651415223739937 ) ) ;
#94254 = CARTESIAN_POINT ( 'NONE',  ( -12.89999999999999147, 2.500000000000000000, 5.122947341949749323 ) ) ;
#94255 = ORIENTED_EDGE ( 'NONE', *, *, #977, .T. ) ;
#94256 = DIRECTION ( 'NONE',  ( 0.000000000000000000, 0.000000000000000000, -1.000000000000000000 ) ) ;
#94257 = AXIS2_PLACEMENT_3D ( 'NONE', #128136, #77720, #120253 ) ;
#94258 = DIRECTION ( 'NONE',  ( -0.000000000000000000, 1.000000000000000000, -0.000000000000000000 ) ) ;
#94259 = EDGE_LOOP ( 'NONE', ( #9604, #62465, #52299, #55798 ) ) ;
#94260 = ORIENTED_EDGE ( 'NONE', *, *, #110440, .F. ) ;
#94261 = AXIS2_PLACEMENT_3D ( 'NONE', #31099, #61842, #31723 ) ;
#94262 = VERTEX_POINT ( 'NONE', #19943 ) ;
#94263 = VERTEX_POINT ( 'NONE', #10728 ) ;
#94264 = CARTESIAN_POINT ( 'NONE',  ( -11.64999999999999680, 2.500000000000000000, -2.957883832488649833 ) ) ;
#94265 = CARTESIAN_POINT ( 'NONE',  ( -11.05000000000000249, 2.500000000000000000, -1.718653347947322052 ) ) ;
#94266 = DIRECTION ( 'NONE',  ( -0.000000000000000000, 1.000000000000000000, -0.000000000000000000 ) ) ;
#94267 = DIRECTION ( 'NONE',  ( -0.000000000000000000, -1.000000000000000000, -0.000000000000000000 ) ) ;
#94268 = DIRECTION ( 'NONE',  ( 0.000000000000000000, 0.000000000000000000, -1.000000000000000000 ) ) ;
#94269 = ORIENTED_EDGE ( 'NONE', *, *, #105933, .F. ) ;
#94270 = CARTESIAN_POINT ( 'NONE',  ( 26.76176527441709396, -1.073658815337092731, 4.445806700577109360 ) ) ;
#94271 = DIRECTION ( 'NONE',  ( 0.000000000000000000, -0.9999939076577903929, 0.003490651415223739937 ) ) ;
#94272 = DIRECTION ( 'NONE',  ( 0.000000000000000000, -0.000000000000000000, 1.000000000000000000 ) ) ;
#94273 = EDGE_CURVE ( 'NONE', #97573, #48757, #111384, .T. ) ;
#94274 = EDGE_LOOP ( 'NONE', ( #81948, #74128, #4539, #92318 ) ) ;
#94275 = ORIENTED_EDGE ( 'NONE', *, *, #98526, .T. ) ;
#94276 = ORIENTED_EDGE ( 'NONE', *, *, #35722, .F. ) ;
#94277 = CONICAL_SURFACE ( 'NONE', #69227, 0.09999999999999982514, 0.003490658503988666988 ) ;
#94278 = DIRECTION ( 'NONE',  ( 0.000000000000000000, 0.000000000000000000, -1.000000000000000000 ) ) ;
#94279 = CIRCLE ( 'NONE', #110907, 0.1000000000000002554 ) ;
#94280 = CONICAL_SURFACE ( 'NONE', #85950, 0.1000000000000002554, 0.003490658503988666988 ) ;
#94281 = CARTESIAN_POINT ( 'NONE',  ( 1.449999999999949551, 12.50000000000000000, 6.841600689897072485 ) ) ;
#94282 = CARTESIAN_POINT ( 'NONE',  ( 1.899999999999951283, 2.500000000000000000, -4.083716857408426826 ) ) ;
#94285 = ORIENTED_EDGE ( 'NONE', *, *, #80285, .F. ) ;
#94284 = EDGE_CURVE ( 'NONE', #31101, #20569, #48623, .T. ) ;
#94283 = AXIS2_PLACEMENT_3D ( 'NONE', #80884, #11485, #71694 ) ;
#94286 = DIRECTION ( 'NONE',  ( -0.000000000000000000, 1.000000000000000000, -0.000000000000000000 ) ) ;
#94287 = CARTESIAN_POINT ( 'NONE',  ( -9.999999999999969802, 2.500000000000000000, -2.276824562219559311E-15 ) ) ;
#94288 = CARTESIAN_POINT ( 'NONE',  ( 184.5000000000000568, -7.615651362878065989, -0.4485267508106103307 ) ) ;
#94289 = ADVANCED_FACE ( 'NONE', ( #99790 ), #77952, .T. ) ;
#94290 = CARTESIAN_POINT ( 'NONE',  ( -9.600000000000006750, 2.500000000000000000, 3.737306695894644371 ) ) ;
#94291 = FACE_OUTER_BOUND ( 'NONE', #64442, .T. ) ;
#94292 = ORIENTED_EDGE ( 'NONE', *, *, #92511, .T. ) ;
#94293 = VERTEX_POINT ( 'NONE', #71607 ) ;
#94294 = ADVANCED_FACE ( 'NONE', ( #29129 ), #54966, .T. ) ;
#94295 = FACE_OUTER_BOUND ( 'NONE', #15346, .T. ) ;
#94296 = PLANE ( 'NONE',  #79100 ) ;
#94297 = CARTESIAN_POINT ( 'NONE',  ( -0.4000000000000392131, 2.500000000000000000, -5.122947341949753763 ) ) ;
#94298 = CARTESIAN_POINT ( 'NONE',  ( -12.89999999999999147, 12.50000000000000000, -5.022947341949751454 ) ) ;
#94299 = CARTESIAN_POINT ( 'NONE',  ( -3.350000000000028511, 2.500000000000000000, 2.757883832488649656 ) ) ;
#94300 = ORIENTED_EDGE ( 'NONE', *, *, #26535, .T. ) ;
#94301 = CIRCLE ( 'NONE', #125599, 0.06509327318403745899 ) ;
#94302 = ORIENTED_EDGE ( 'NONE', *, *, #59324, .T. ) ;
#94303 = DIRECTION ( 'NONE',  ( -0.000000000000000000, -1.000000000000000000, -0.000000000000000000 ) ) ;
#94304 = FACE_OUTER_BOUND ( 'NONE', #35512, .T. ) ;
#94305 = DIRECTION ( 'NONE',  ( 0.000000000000000000, -0.9999939076577903929, 0.003490651415223739937 ) ) ;
#94306 = DIRECTION ( 'NONE',  ( 1.000000000000000000, 0.000000000000000000, 0.000000000000000000 ) ) ;
#94307 = ORIENTED_EDGE ( 'NONE', *, *, #93468, .T. ) ;
#94308 = AXIS2_PLACEMENT_3D ( 'NONE', #94917, #45184, #3314 ) ;
#94309 = DIRECTION ( 'NONE',  ( 0.000000000000000000, 1.000000000000000000, 0.000000000000000000 ) ) ;
#94310 = VECTOR ( 'NONE', #55298, 1000.000000000000000 ) ;
#94311 = CARTESIAN_POINT ( 'NONE',  ( 8.149999999999920419, 2.500000000000000000, 6.048780366869521252 ) ) ;
#94312 = VERTEX_POINT ( 'NONE', #39605 ) ;
#94313 = DIRECTION ( 'NONE',  ( 0.000000000000000000, 1.000000000000000000, 0.000000000000000000 ) ) ;
#94314 = ORIENTED_EDGE ( 'NONE', *, *, #124902, .T. ) ;
#94315 = CIRCLE ( 'NONE', #44158, 0.06509327318403745899 ) ;
#94316 = CARTESIAN_POINT ( 'NONE',  ( 13.74999999999993427, 12.50000000000000000, 2.099970236277060032 ) ) ;
#94317 = EDGE_CURVE ( 'NONE', #72203, #20272, #80010, .T. ) ;
#94318 = VERTEX_POINT ( 'NONE', #10119 ) ;
#94319 = DIRECTION ( 'NONE',  ( 0.000000000000000000, 1.000000000000000000, 0.000000000000000000 ) ) ;
#94320 = CARTESIAN_POINT ( 'NONE',  ( -8.550000000000007816, 2.500000000000000000, 6.148780366869520009 ) ) ;
#94321 = ORIENTED_EDGE ( 'NONE', *, *, #65790, .T. ) ;
#94322 = ORIENTED_EDGE ( 'NONE', *, *, #30085, .F. ) ;
#94323 = ADVANCED_FACE ( 'NONE', ( #90600 ), #88405, .T. ) ;
#94324 = CARTESIAN_POINT ( 'NONE',  ( 187.1718750003414016, 9.264065473108010111E-16, -7.564683531250000925 ) ) ;
#94325 = EDGE_CURVE ( 'NONE', #37140, #49253, #15236, .T. ) ;
#94327 = CARTESIAN_POINT ( 'NONE',  ( 185.2968750003414300, 8.734944146203032389, 5.348610694689227483E-16 ) ) ;
#94326 = AXIS2_PLACEMENT_3D ( 'NONE', #108459, #7672, #109092 ) ;
#94328 = CARTESIAN_POINT ( 'NONE',  ( -5.650000000000019895, 12.50000000000000000, 6.148780366869520009 ) ) ;
#94329 = CARTESIAN_POINT ( 'NONE',  ( -11.05000000000000249, 2.500000000000000000, -6.248780366869523206 ) ) ;
#94330 = CIRCLE ( 'NONE', #40067, 0.06509327318403745899 ) ;
#94331 = DIRECTION ( 'NONE',  ( -4.274815082592931898E-19, -0.9999939076577903929, -0.003490651415223739937 ) ) ;
#94332 = ADVANCED_FACE ( 'NONE', ( #31694 ), #42369, .T. ) ;
#94333 = EDGE_CURVE ( 'NONE', #69856, #108500, #105136, .T. ) ;
#94334 = CARTESIAN_POINT ( 'NONE',  ( 1.649999999999951505, 12.50000000000000000, -1.472243186433550122 ) ) ;
#94335 = CARTESIAN_POINT ( 'NONE',  ( 7.949999999999922018, 2.500000000000000000, 6.395190528383296602 ) ) ;
#94336 = ADVANCED_FACE ( 'NONE', ( #69022 ), #128630, .T. ) ;
#94338 = EDGE_CURVE ( 'NONE', #60021, #52226, #113460, .T. ) ;
#94337 = AXIS2_PLACEMENT_3D ( 'NONE', #32530, #62625, #61329 ) ;
#94339 = ORIENTED_EDGE ( 'NONE', *, *, #52520, .F. ) ;
#94340 = ORIENTED_EDGE ( 'NONE', *, *, #123160, .T. ) ;
#94341 = CARTESIAN_POINT ( 'NONE',  ( 0.3999999999999555023, 12.50000000000000000, 4.395220292106234439 ) ) ;
#94342 = EDGE_CURVE ( 'NONE', #58914, #5985, #2631, .T. ) ;
#94343 = CIRCLE ( 'NONE', #60906, 0.06509327318403745899 ) ;
#94344 = CIRCLE ( 'NONE', #27442, 0.06509327318403741736 ) ;
#94345 = DIRECTION ( 'NONE',  ( -4.274815082592931898E-19, -0.9999939076577903929, -0.003490651415223739937 ) ) ;
#94346 = DIRECTION ( 'NONE',  ( 0.000000000000000000, 1.000000000000000000, 0.000000000000000000 ) ) ;
#94347 = PLANE ( 'NONE',  #76228 ) ;
#94349 = VERTEX_POINT ( 'NONE', #43461 ) ;
#94348 = ORIENTED_EDGE ( 'NONE', *, *, #72342, .F. ) ;
#94350 = CARTESIAN_POINT ( 'NONE',  ( -0.4000000000000396572, 2.500000000000000000, 3.637306695894644726 ) ) ;
#94351 = ORIENTED_EDGE ( 'NONE', *, *, #43501, .F. ) ;
#94352 = DIRECTION ( 'NONE',  ( -0.000000000000000000, 1.000000000000000000, -0.000000000000000000 ) ) ;
#94353 = CARTESIAN_POINT ( 'NONE',  ( -5.000000000000024869, 12.50000000000000000, -5.088040615133791356 ) ) ;
#94354 = ADVANCED_FACE ( 'NONE', ( #34930 ), #36110, .T. ) ;
#94355 = VERTEX_POINT ( 'NONE', #2879 ) ;
#94356 = DIRECTION ( 'NONE',  ( -0.000000000000000000, -1.000000000000000000, -0.000000000000000000 ) ) ;
#94357 = DIRECTION ( 'NONE',  ( 0.000000000000000000, -0.9999939076577903929, 0.003490651415223739937 ) ) ;
#94358 = FACE_OUTER_BOUND ( 'NONE', #106991, .T. ) ;
#94359 = DIRECTION ( 'NONE',  ( -0.000000000000000000, 1.000000000000000000, -0.000000000000000000 ) ) ;
#94360 = DIRECTION ( 'NONE',  ( 0.000000000000000000, 0.000000000000000000, 1.000000000000000000 ) ) ;
#94361 = DIRECTION ( 'NONE',  ( 0.000000000000000000, 1.000000000000000000, 0.000000000000000000 ) ) ;
#94362 = CARTESIAN_POINT ( 'NONE',  ( 185.8593750003413732, 0.000000000000000000, 7.564683531250000925 ) ) ;
#94363 = CARTESIAN_POINT ( 'NONE',  ( 1.049999999999952971, 2.500000000000000000, 6.148780366869520897 ) ) ;
#94364 = DIRECTION ( 'NONE',  ( -0.000000000000000000, 1.000000000000000000, -0.000000000000000000 ) ) ;
#94365 = VERTEX_POINT ( 'NONE', #73531 ) ;
#94366 = ORIENTED_EDGE ( 'NONE', *, *, #119637, .F. ) ;
#94367 = ORIENTED_EDGE ( 'NONE', *, *, #2702, .F. ) ;
#94368 = CARTESIAN_POINT ( 'NONE',  ( -8.150000000000014566, 12.50000000000000000, -6.906693963081110610 ) ) ;
#94369 = ORIENTED_EDGE ( 'NONE', *, *, #31645, .T. ) ;
#94370 = CIRCLE ( 'NONE', #21124, 0.1000000000000000056 ) ;
#94371 = DIRECTION ( 'NONE',  ( -0.000000000000000000, 1.000000000000000000, -0.000000000000000000 ) ) ;
#94372 = AXIS2_PLACEMENT_3D ( 'NONE', #86198, #126142, #94744 ) ;
#94373 = CIRCLE ( 'NONE', #123697, 0.09999999999999999167 ) ;
#94375 = ORIENTED_EDGE ( 'NONE', *, *, #45394, .T. ) ;
#94374 = EDGE_LOOP ( 'NONE', ( #10266, #25736, #68879, #26141 ) ) ;
#94376 = EDGE_LOOP ( 'NONE', ( #74906, #19057 ) ) ;
#94377 = PLANE ( 'NONE',  #77266 ) ;
#94378 = VECTOR ( 'NONE', #110562, 1000.000000000000000 ) ;
#94379 = CARTESIAN_POINT ( 'NONE',  ( 5.599999999999931255, 2.500000000000000000, 4.576537180435972019 ) ) ;
#94380 = CIRCLE ( 'NONE', #65121, 0.09999999999999982514 ) ;
#94381 = LINE ( 'NONE', #15157, #1219 ) ;
#94382 = PLANE ( 'NONE',  #85312 ) ;
#94383 = AXIS2_PLACEMENT_3D ( 'NONE', #121933, #81381, #82001 ) ;
#94384 = CARTESIAN_POINT ( 'NONE',  ( 9.349999999999916156, 2.500000000000000000, 6.841600689897072485 ) ) ;
#94385 = ORIENTED_EDGE ( 'NONE', *, *, #39686, .T. ) ;
#94386 = CARTESIAN_POINT ( 'NONE',  ( 1.699999999999950218, 2.500000000000000000, 4.430127018922196847 ) ) ;
#94387 = ORIENTED_EDGE ( 'NONE', *, *, #80467, .T. ) ;
#94388 = VERTEX_POINT ( 'NONE', #74839 ) ;
#94389 = ADVANCED_FACE ( 'NONE', ( #122011 ), #52822, .T. ) ;
#94390 = EDGE_LOOP ( 'NONE', ( #40218, #39359, #2942, #100012 ) ) ;
#94391 = DIRECTION ( 'NONE',  ( 0.000000000000000000, 0.000000000000000000, -1.000000000000000000 ) ) ;
#94392 = EDGE_LOOP ( 'NONE', ( #87737, #47371, #119619, #50985 ) ) ;
#94393 = ORIENTED_EDGE ( 'NONE', *, *, #69301, .T. ) ;
#94394 = ORIENTED_EDGE ( 'NONE', *, *, #20054, .F. ) ;
#94395 = DIRECTION ( 'NONE',  ( -0.000000000000000000, 1.000000000000000000, -0.000000000000000000 ) ) ;
#94396 = ADVANCED_FACE ( 'NONE', ( #94460 ), #40321, .T. ) ;
#94397 = CARTESIAN_POINT ( 'NONE',  ( 14.54999999999989591, 2.500000000000000000, 2.265063509461097357 ) ) ;
#94398 = CARTESIAN_POINT ( 'NONE',  ( -14.14999999999998614, 12.50000000000000000, 1.407149913249511997 ) ) ;
#94399 = PLANE ( 'NONE',  #121556 ) ;
#94400 = DIRECTION ( 'NONE',  ( -0.000000000000000000, 1.000000000000000000, -0.000000000000000000 ) ) ;
#94401 = CARTESIAN_POINT ( 'NONE',  ( 4.349999999999941025, 12.50000000000000000, -1.818653347947326138 ) ) ;
#94402 = VERTEX_POINT ( 'NONE', #53909 ) ;
#94403 = FACE_OUTER_BOUND ( 'NONE', #87252, .T. ) ;
#94404 = AXIS2_PLACEMENT_3D ( 'NONE', #32653, #14255, #5081 ) ;
#94405 = AXIS2_PLACEMENT_3D ( 'NONE', #25179, #7469, #106327 ) ;
#94406 = VERTEX_POINT ( 'NONE', #114113 ) ;
#94407 = LINE ( 'NONE', #34881, #81877 ) ;
#94408 = ORIENTED_EDGE ( 'NONE', *, *, #122700, .F. ) ;
#94409 = DIRECTION ( 'NONE',  ( 0.000000000000000000, 1.000000000000000000, 0.000000000000000000 ) ) ;
#94410 = ORIENTED_EDGE ( 'NONE', *, *, #109405, .F. ) ;
#94411 = EDGE_LOOP ( 'NONE', ( #99538, #3557, #121016, #32244 ) ) ;
#94412 = CONICAL_SURFACE ( 'NONE', #98516, 0.1000000000000002554, 0.003490658503988666988 ) ;
#94413 = DIRECTION ( 'NONE',  ( -4.274815082592931898E-19, -0.9999939076577903929, -0.003490651415223739937 ) ) ;
#94414 = DIRECTION ( 'NONE',  ( 0.000000000000000000, 1.000000000000000000, 0.000000000000000000 ) ) ;
#94415 = VECTOR ( 'NONE', #16940, 1000.000000000000000 ) ;
#94416 = CONICAL_SURFACE ( 'NONE', #102726, 0.09999999999999999167, 0.003490658503988666988 ) ;
#94417 = CARTESIAN_POINT ( 'NONE',  ( -7.500000000000016875, 2.500000000000000000, -3.637306695894650055 ) ) ;
#94418 = EDGE_LOOP ( 'NONE', ( #23996, #99022, #107441, #44004 ) ) ;
#94419 = LINE ( 'NONE', #82204, #65878 ) ;
#94420 = ORIENTED_EDGE ( 'NONE', *, *, #116844, .F. ) ;
#94421 = CARTESIAN_POINT ( 'NONE',  ( -9.150000000000009237, 2.500000000000000000, -2.265063509461101798 ) ) ;
#94422 = CARTESIAN_POINT ( 'NONE',  ( -1.650000000000035660, 2.500000000000000000, 7.288010851410849256 ) ) ;
#94423 = PLANE ( 'NONE',  #73194 ) ;
#94424 = CARTESIAN_POINT ( 'NONE',  ( -9.150000000000011013, 2.500000000000000000, -5.802370205355744659 ) ) ;
#94425 = VECTOR ( 'NONE', #58585, 1000.000000000000000 ) ;
#94426 = AXIS2_PLACEMENT_3D ( 'NONE', #85054, #83770, #5194 ) ;
#94427 = CARTESIAN_POINT ( 'NONE',  ( 6.699999999999928235, 12.50000000000000000, -0.06509327318403970719 ) ) ;
#94428 = EDGE_CURVE ( 'NONE', #43830, #72875, #29845, .T. ) ;
#94429 = ORIENTED_EDGE ( 'NONE', *, *, #106786, .F. ) ;
#94430 = CIRCLE ( 'NONE', #109187, 0.06509327318403745899 ) ;
#94431 = VECTOR ( 'NONE', #68438, 1000.000000000000000 ) ;
#94432 = AXIS2_PLACEMENT_3D ( 'NONE', #77567, #118149, #97860 ) ;
#94433 = ORIENTED_EDGE ( 'NONE', *, *, #53577, .T. ) ;
#94434 = FACE_OUTER_BOUND ( 'NONE', #22160, .T. ) ;
#94436 = ADVANCED_FACE ( 'NONE', ( #123290 ), #74195, .T. ) ;
#94435 = DIRECTION ( 'NONE',  ( -0.000000000000000000, 1.000000000000000000, -0.000000000000000000 ) ) ;
#94437 = EDGE_CURVE ( 'NONE', #39788, #64883, #124585, .T. ) ;
#94438 = CARTESIAN_POINT ( 'NONE',  ( 184.3802083336747444, 4.367472073101515306, 7.564683531250000925 ) ) ;
#94439 = CARTESIAN_POINT ( 'NONE',  ( 1.249999999999953815, 2.500000000000000000, -2.957883832488653830 ) ) ;
#94440 = DIRECTION ( 'NONE',  ( 0.000000000000000000, 0.000000000000000000, 1.000000000000000000 ) ) ;
#94441 = CARTESIAN_POINT ( 'NONE',  ( 3.149999999999946176, 2.500000000000000000, -1.818653347947325916 ) ) ;
#94442 = EDGE_CURVE ( 'NONE', #34687, #118817, #25720, .T. ) ;
#94443 = DIRECTION ( 'NONE',  ( 0.000000000000000000, -0.9999939076577903929, 0.003490651415223739937 ) ) ;
#94444 = ORIENTED_EDGE ( 'NONE', *, *, #68202, .F. ) ;
#94445 = CARTESIAN_POINT ( 'NONE',  ( -10.65000000000000391, 2.500000000000000000, -6.941600689897075682 ) ) ;
#94447 = DIRECTION ( 'NONE',  ( -0.000000000000000000, 1.000000000000000000, -0.000000000000000000 ) ) ;
#94446 = B_SPLINE_CURVE_WITH_KNOTS ( 'NONE', 3,
 ( #107873, #86943, #96749, #127523, #106581, #38517, #16875, #48313 ),
 .UNSPECIFIED., .F., .F.,
 ( 4, 2, 2, 4 ),
 ( 0.000000000000000000, 0.001904977314310103524, 0.002857465971465155286, 0.003809954628620207048 ),
 .UNSPECIFIED. ) ;
#94448 = DIRECTION ( 'NONE',  ( -0.000000000000000000, -1.000000000000000000, -0.000000000000000000 ) ) ;
#94449 = ADVANCED_FACE ( 'NONE', ( #32370 ), #98880, .T. ) ;
#94450 = EDGE_LOOP ( 'NONE', ( #123706, #65491 ) ) ;
#94451 = EDGE_CURVE ( 'NONE', #119417, #72819, #48821, .T. ) ;
#94452 = CARTESIAN_POINT ( 'NONE',  ( 184.5000000000000000, 0.000000000000000000, -5.200000000000000178 ) ) ;
#94453 = ORIENTED_EDGE ( 'NONE', *, *, #126272, .T. ) ;
#94454 = CARTESIAN_POINT ( 'NONE',  ( 2.099999999999949463, 2.500000000000000000, 0.6928203230275494784 ) ) ;
#94455 = AXIS2_PLACEMENT_3D ( 'NONE', #90946, #1273, #123610 ) ;
#94456 = AXIS2_PLACEMENT_3D ( 'NONE', #110991, #101843, #11524 ) ;
#94457 = VECTOR ( 'NONE', #74137, 1000.000000000000000 ) ;
#94458 = EDGE_LOOP ( 'NONE', ( #34795, #32884 ) ) ;
#94459 = DIRECTION ( 'NONE',  ( 0.000000000000000000, 0.000000000000000000, 1.000000000000000000 ) ) ;
#94460 = FACE_OUTER_BOUND ( 'NONE', #77954, .T. ) ;
#94461 = DIRECTION ( 'NONE',  ( -0.000000000000000000, -1.000000000000000000, -0.000000000000000000 ) ) ;
#94462 = ORIENTED_EDGE ( 'NONE', *, *, #116381, .T. ) ;
#94464 = CARTESIAN_POINT ( 'NONE',  ( 185.6979166673494603, 6.668395609140176816, 3.850000000000000977 ) ) ;
#94463 = AXIS2_PLACEMENT_3D ( 'NONE', #7681, #74511, #47629 ) ;
#94465 = AXIS2_PLACEMENT_3D ( 'NONE', #26940, #23220, #63153 ) ;
#94466 = FACE_OUTER_BOUND ( 'NONE', #14250, .T. ) ;
#94467 = VECTOR ( 'NONE', #122712, 1000.000000000000000 ) ;
#94468 = CIRCLE ( 'NONE', #102782, 0.06509327318403745899 ) ;
#94469 = ORIENTED_EDGE ( 'NONE', *, *, #37170, .T. ) ;
#94470 = CIRCLE ( 'NONE', #19156, 0.1000000000000002554 ) ;
#94471 = DIRECTION ( 'NONE',  ( 0.000000000000000000, 0.000000000000000000, -1.000000000000000000 ) ) ;
#94472 = ORIENTED_EDGE ( 'NONE', *, *, #98179, .T. ) ;
#94473 = ORIENTED_EDGE ( 'NONE', *, *, #68314, .T. ) ;
#94474 = CARTESIAN_POINT ( 'NONE',  ( 11.04999999999990656, 12.50000000000000000, 2.511473670974873507 ) ) ;
#94475 = CARTESIAN_POINT ( 'NONE',  ( -0.6000000000000323963, 2.500000000000000000, 0.2464101615137759549 ) ) ;
#94476 = ORIENTED_EDGE ( 'NONE', *, *, #12863, .T. ) ;
#94477 = DIRECTION ( 'NONE',  ( -4.274815082592931898E-19, -0.9999939076577903929, -0.003490651415223739937 ) ) ;
#94478 = DIRECTION ( 'NONE',  ( -4.274815082592931898E-19, -0.9999939076577903929, -0.003490651415223739937 ) ) ;
#94479 = ORIENTED_EDGE ( 'NONE', *, *, #91388, .T. ) ;
#94480 = EDGE_CURVE ( 'NONE', #59346, #38624, #91900, .T. ) ;
#94481 = CARTESIAN_POINT ( 'NONE',  ( 9.999999999999916511, 2.500000000000000000, -0.7928203230275542301 ) ) ;
#94482 = CARTESIAN_POINT ( 'NONE',  ( 8.749999999999918288, 2.500000000000000000, 7.188010851410848723 ) ) ;
#94484 = ADVANCED_FACE ( 'NONE', ( #104298 ), #82072, .T. ) ;
#94483 = DIRECTION ( 'NONE',  ( -4.274815082592931898E-19, -0.9999939076577903929, -0.003490651415223739937 ) ) ;
#94485 = CARTESIAN_POINT ( 'NONE',  ( 17.49149641758750562, -2.499999999999849010, -4.292093396893348789 ) ) ;
#94486 = CARTESIAN_POINT ( 'NONE',  ( -14.14999999999998614, 2.500000000000000000, 1.572243186433549544 ) ) ;
#94487 = ADVANCED_FACE ( 'NONE', ( #63081 ), #94772, .T. ) ;
#94488 = DIRECTION ( 'NONE',  ( 0.000000000000000000, 0.000000000000000000, 1.000000000000000000 ) ) ;
#94489 = DIRECTION ( 'NONE',  ( 0.000000000000000000, 0.000000000000000000, 1.000000000000000000 ) ) ;
#94490 = EDGE_CURVE ( 'NONE', #1350, #110433, #4780, .T. ) ;
#94491 = ADVANCED_FACE ( 'NONE', ( #32996 ), #113555, .T. ) ;
#94492 = AXIS2_PLACEMENT_3D ( 'NONE', #69153, #79631, #109062 ) ;
#94493 = VECTOR ( 'NONE', #83940, 1000.000000000000000 ) ;
#94494 = EDGE_LOOP ( 'NONE', ( #112276, #94174 ) ) ;
#94495 = VERTEX_POINT ( 'NONE', #23152 ) ;
#94497 = ORIENTED_EDGE ( 'NONE', *, *, #69141, .T. ) ;
#94496 = EDGE_CURVE ( 'NONE', #103868, #17323, #46661, .T. ) ;
#94498 = EDGE_LOOP ( 'NONE', ( #25235, #100240 ) ) ;
#94499 = LINE ( 'NONE', #114785, #62061 ) ;
#94500 = CARTESIAN_POINT ( 'NONE',  ( -0.4500000000000397571, 2.500000000000000000, -6.495190528383302464 ) ) ;
#94501 = CARTESIAN_POINT ( 'NONE',  ( -13.94999999999998863, 2.500000000000000000, 2.511473670974877503 ) ) ;
#94502 = ORIENTED_EDGE ( 'NONE', *, *, #60767, .T. ) ;
#94503 = FACE_BOUND ( 'NONE', #87012, .T. ) ;
#94504 = AXIS2_PLACEMENT_3D ( 'NONE', #109770, #79657, #59404 ) ;
#94505 = DIRECTION ( 'NONE',  ( 0.000000000000000000, 0.000000000000000000, 1.000000000000000000 ) ) ;
#94506 = CARTESIAN_POINT ( 'NONE',  ( 10.44999999999991402, 2.500000000000000000, -2.165063509461101710 ) ) ;
#94507 = AXIS2_PLACEMENT_3D ( 'NONE', #45481, #23900, #63821 ) ;
#94508 = EDGE_CURVE ( 'NONE', #34729, #45548, #17387, .T. ) ;
#94510 = DIRECTION ( 'NONE',  ( 0.000000000000000000, 0.000000000000000000, -1.000000000000000000 ) ) ;
#94509 = CIRCLE ( 'NONE', #6651, 0.1000000000000002554 ) ;
#94511 = EDGE_CURVE ( 'NONE', #53510, #120782, #35566, .T. ) ;
#94512 = VECTOR ( 'NONE', #73661, 1000.000000000000000 ) ;
#94513 = LINE ( 'NONE', #76822, #15740 ) ;
#94514 = DIRECTION ( 'NONE',  ( 0.000000000000000000, 1.000000000000000000, 0.000000000000000000 ) ) ;
#94515 = PLANE ( 'NONE',  #9930 ) ;
#94516 = CARTESIAN_POINT ( 'NONE',  ( -11.64999999999999680, 2.500000000000000000, -6.495190528383298911 ) ) ;
#94517 = CARTESIAN_POINT ( 'NONE',  ( 1.649999999999950617, 2.500000000000000000, -2.165063509461101710 ) ) ;
#94518 = CARTESIAN_POINT ( 'NONE',  ( 6.249999999999968914, 12.50000000000000000, -6.495190528383302464 ) ) ;
#94519 = AXIS2_PLACEMENT_3D ( 'NONE', #104136, #120076, #50066 ) ;
#94520 = CARTESIAN_POINT ( 'NONE',  ( -4.350000000000023626, 2.500000000000000000, -1.818653347947325916 ) ) ;
#94521 = AXIS2_PLACEMENT_3D ( 'NONE', #24307, #35428, #43956 ) ;
#94522 = EDGE_LOOP ( 'NONE', ( #110179, #121967 ) ) ;
#94523 = ORIENTED_EDGE ( 'NONE', *, *, #3963, .F. ) ;
#94524 = EDGE_LOOP ( 'NONE', ( #974, #95033 ) ) ;
#94526 = VERTEX_POINT ( 'NONE', #57782 ) ;
#94525 = AXIS2_PLACEMENT_3D ( 'NONE', #66315, #97072, #85942 ) ;
#94527 = AXIS2_PLACEMENT_3D ( 'NONE', #96974, #129046, #7294 ) ;
#94528 = CIRCLE ( 'NONE', #107035, 0.09999999999999999167 ) ;
#94529 = DIRECTION ( 'NONE',  ( 0.000000000000000000, 1.000000000000000000, 0.000000000000000000 ) ) ;
#94530 = ORIENTED_EDGE ( 'NONE', *, *, #12811, .F. ) ;
#94531 = FACE_OUTER_BOUND ( 'NONE', #8680, .T. ) ;
#94532 = ORIENTED_EDGE ( 'NONE', *, *, #84990, .T. ) ;
#94533 = EDGE_LOOP ( 'NONE', ( #199, #117878 ) ) ;
#94534 = CIRCLE ( 'NONE', #63147, 0.06509327318403745899 ) ;
#94535 = AXIS2_PLACEMENT_3D ( 'NONE', #31420, #40617, #32723 ) ;
#94536 = CARTESIAN_POINT ( 'NONE',  ( 7.314170287631764467, -1.500000000000000222, 9.688393442221800100 ) ) ;
#94537 = FACE_OUTER_BOUND ( 'NONE', #46676, .T. ) ;
#94538 = DIRECTION ( 'NONE',  ( 0.000000000000000000, 0.000000000000000000, 1.000000000000000000 ) ) ;
#94539 = CARTESIAN_POINT ( 'NONE',  ( 6.649999999999929301, 12.50000000000000000, -2.165063509461101710 ) ) ;
#94540 = VERTEX_POINT ( 'NONE', #36212 ) ;
#94541 = VERTEX_POINT ( 'NONE', #27029 ) ;
#94542 = ORIENTED_EDGE ( 'NONE', *, *, #20456, .T. ) ;
#94544 = ORIENTED_EDGE ( 'NONE', *, *, #37558, .T. ) ;
#94543 = DIRECTION ( 'NONE',  ( -4.274815082592931898E-19, -0.9999939076577903929, -0.003490651415223739937 ) ) ;
#94545 = DIRECTION ( 'NONE',  ( 0.000000000000000000, 1.000000000000000000, 0.000000000000000000 ) ) ;
#94546 = ORIENTED_EDGE ( 'NONE', *, *, #72415, .T. ) ;
#94547 = ORIENTED_EDGE ( 'NONE', *, *, #46757, .F. ) ;
#94548 = DIRECTION ( 'NONE',  ( 0.000000000000000000, 0.000000000000000000, 1.000000000000000000 ) ) ;
#94549 = EDGE_CURVE ( 'NONE', #112302, #21997, #116683, .T. ) ;
#94550 = CARTESIAN_POINT ( 'NONE',  ( -15.59999999999998010, 2.500000000000000000, -0.4464101615137759382 ) ) ;
#94551 = CARTESIAN_POINT ( 'NONE',  ( -1.850000000000033396, 2.500000000000000000, -1.918653347947325782 ) ) ;
#94553 = DIRECTION ( 'NONE',  ( 0.000000000000000000, 1.000000000000000000, 0.000000000000000000 ) ) ;
#94552 = AXIS2_PLACEMENT_3D ( 'NONE', #48947, #79055, #20119 ) ;
#94554 = VECTOR ( 'NONE', #129020, 1000.000000000000000 ) ;
#94555 = CIRCLE ( 'NONE', #10907, 0.06509327318403745899 ) ;
#94556 = PLANE ( 'NONE',  #8492 ) ;
#94557 = ORIENTED_EDGE ( 'NONE', *, *, #31062, .T. ) ;
#94558 = DIRECTION ( 'NONE',  ( 0.000000000000000000, 0.000000000000000000, 1.000000000000000000 ) ) ;
#94560 = EDGE_LOOP ( 'NONE', ( #629, #74951, #102689, #79713 ) ) ;
#94559 = CIRCLE ( 'NONE', #6799, 0.1000000000000002554 ) ;
#94561 = DIRECTION ( 'NONE',  ( -0.000000000000000000, -1.000000000000000000, -0.000000000000000000 ) ) ;
#94562 = CONICAL_SURFACE ( 'NONE', #123794, 0.1000000000000002554, 0.003490658503988666988 ) ;
#94563 = VERTEX_POINT ( 'NONE', #87218 ) ;
#94564 = CARTESIAN_POINT ( 'NONE',  ( 13.09999999999990195, 12.50000000000000000, -4.611443907251940644 ) ) ;
#94565 = DIRECTION ( 'NONE',  ( 0.000000000000000000, 0.000000000000000000, 1.000000000000000000 ) ) ;
#94566 = AXIS2_PLACEMENT_3D ( 'NONE', #34999, #4202, #74905 ) ;
#94567 = CARTESIAN_POINT ( 'NONE',  ( 10.59999999999991260, 2.500000000000000000, -0.3464101615137783474 ) ) ;
#94568 = DIRECTION ( 'NONE',  ( -0.000000000000000000, -1.000000000000000000, -0.000000000000000000 ) ) ;
#94569 = EDGE_LOOP ( 'NONE', ( #48916, #9306 ) ) ;
#94570 = CIRCLE ( 'NONE', #102882, 0.06509327318403745899 ) ;
#94571 = SURFACE_SIDE_STYLE ('',( #45499 ) ) ;
#94572 = CARTESIAN_POINT ( 'NONE',  ( 9.399999999999915090, 2.500000000000000000, -3.983716857408426293 ) ) ;
#94573 = EDGE_LOOP ( 'NONE', ( #95445, #95798, #119537, #97830 ) ) ;
#94574 = ORIENTED_EDGE ( 'NONE', *, *, #54583, .T. ) ;
#94575 = ORIENTED_EDGE ( 'NONE', *, *, #112280, .F. ) ;
#94576 = CARTESIAN_POINT ( 'NONE',  ( -13.34999999999999076, 2.500000000000000000, -2.265063509461099578 ) ) ;
#94577 = CARTESIAN_POINT ( 'NONE',  ( 8.149999999999920419, 12.50000000000000000, -1.818653347947325916 ) ) ;
#94578 = CARTESIAN_POINT ( 'NONE',  ( 185.4427083336747160, -6.551208109652278289, 3.782341765624995134 ) ) ;
#94579 = DIRECTION ( 'NONE',  ( -0.000000000000000000, 1.000000000000000000, -0.000000000000000000 ) ) ;
#94580 = VECTOR ( 'NONE', #107821, 1000.000000000000000 ) ;
#94581 = CARTESIAN_POINT ( 'NONE',  ( 8.949999999999917577, 2.500000000000000000, 6.148780366869520009 ) ) ;
#94582 = LINE ( 'NONE', #4911, #38246 ) ;
#94583 = VERTEX_POINT ( 'NONE', #95765 ) ;
#94584 = DIRECTION ( 'NONE',  ( 0.000000000000000000, 0.000000000000000000, 1.000000000000000000 ) ) ;
#94585 = EDGE_CURVE ( 'NONE', #56480, #59007, #109347, .T. ) ;
#94586 = ORIENTED_EDGE ( 'NONE', *, *, #33531, .F. ) ;
#94587 = ADVANCED_FACE ( 'NONE', ( #85293 ), #101039, .T. ) ;
#94588 = CARTESIAN_POINT ( 'NONE',  ( -0.6500000000000398792, 2.500000000000000000, -2.411473670974877859 ) ) ;
#94589 = CARTESIAN_POINT ( 'NONE',  ( 127.5000000000000000, 5.000000000000000000, -4.999999999999998224 ) ) ;
#94590 = LINE ( 'NONE', #54042, #77287 ) ;
#94591 = VECTOR ( 'NONE', #27820, 1000.000000000000000 ) ;
#94592 = ADVANCED_FACE ( 'NONE', ( #106852 ), #92628, .T. ) ;
#94593 = CIRCLE ( 'NONE', #50690, 0.06509327318403745899 ) ;
#94594 = EDGE_LOOP ( 'NONE', ( #33582, #45340 ) ) ;
#94595 = CONICAL_SURFACE ( 'NONE', #117564, 0.09999999999999982514, 0.003490658503988666988 ) ;
#94596 = CONICAL_SURFACE ( 'NONE', #15167, 0.1000000000000002554, 0.003490658503988666988 ) ;
#94597 = DIRECTION ( 'NONE',  ( 0.000000000000000000, 0.000000000000000000, -1.000000000000000000 ) ) ;
#94598 = DIRECTION ( 'NONE',  ( 0.000000000000000000, 0.000000000000000000, 1.000000000000000000 ) ) ;
#94599 = ADVANCED_FACE ( 'NONE', ( #47313 ), #26391, .T. ) ;
#94600 = ADVANCED_FACE ( 'NONE', ( #16534 ), #44600, .T. ) ;
#94601 = EDGE_CURVE ( 'NONE', #21869, #110514, #67566, .T. ) ;
#94602 = ADVANCED_FACE ( 'NONE', ( #46666 ), #23669, .T. ) ;
#94603 = ORIENTED_EDGE ( 'NONE', *, *, #86303, .T. ) ;
#94605 = AXIS2_PLACEMENT_3D ( 'NONE', #70040, #100149, #40608 ) ;
#94604 = DIRECTION ( 'NONE',  ( 0.000000000000000000, -0.000000000000000000, 1.000000000000000000 ) ) ;
#94606 = ORIENTED_EDGE ( 'NONE', *, *, #110627, .F. ) ;
#94607 = AXIS2_PLACEMENT_3D ( 'NONE', #58829, #120330, #20839 ) ;
#94609 = VERTEX_POINT ( 'NONE', #97054 ) ;
#94608 = CIRCLE ( 'NONE', #52758, 0.06509327318403745899 ) ;
#94610 = VECTOR ( 'NONE', #39350, 1000.000000000000000 ) ;
#94611 = DIRECTION ( 'NONE',  ( 0.000000000000000000, 1.000000000000000000, 0.000000000000000000 ) ) ;
#94612 = EDGE_CURVE ( 'NONE', #46131, #129259, #678, .T. ) ;
#94614 = ORIENTED_EDGE ( 'NONE', *, *, #95815, .F. ) ;
#94613 = AXIS2_PLACEMENT_3D ( 'NONE', #90801, #80349, #67934 ) ;
#94615 = DIRECTION ( 'NONE',  ( 0.000000000000000000, 0.000000000000000000, 1.000000000000000000 ) ) ;
#94616 = DIRECTION ( 'NONE',  ( 0.000000000000000000, 0.000000000000000000, 1.000000000000000000 ) ) ;
#94617 = DIRECTION ( 'NONE',  ( 0.000000000000000000, -0.9999939076577903929, 0.003490651415223739937 ) ) ;
#94618 = ORIENTED_EDGE ( 'NONE', *, *, #116176, .F. ) ;
#94619 = FACE_BOUND ( 'NONE', #19732, .T. ) ;
#94620 = AXIS2_PLACEMENT_3D ( 'NONE', #42373, #82303, #29983 ) ;
#94621 = CARTESIAN_POINT ( 'NONE',  ( 9.799999999999913669, 2.500000000000000000, 4.676537180435972552 ) ) ;
#94623 = ORIENTED_EDGE ( 'NONE', *, *, #50906, .T. ) ;
#94622 = DIRECTION ( 'NONE',  ( -4.274815082592931898E-19, -0.9999939076577903929, -0.003490651415223739937 ) ) ;
#94624 = DIRECTION ( 'NONE',  ( 0.000000000000000000, 1.000000000000000000, 0.000000000000000000 ) ) ;
#94625 = CARTESIAN_POINT ( 'NONE',  ( -7.300000000000018474, 12.50000000000000000, -4.048810130592463530 ) ) ;
#94626 = ORIENTED_EDGE ( 'NONE', *, *, #111878, .T. ) ;
#94627 = EDGE_LOOP ( 'NONE', ( #40552, #88873 ) ) ;
#94628 = ORIENTED_EDGE ( 'NONE', *, *, #122795, .F. ) ;
#94629 = DIRECTION ( 'NONE',  ( -0.000000000000000000, -1.000000000000000000, -0.000000000000000000 ) ) ;
#94630 = CARTESIAN_POINT ( 'NONE',  ( -4.400000000000028777, 2.500000000000000000, -4.676537180435978769 ) ) ;
#94631 = CARTESIAN_POINT ( 'NONE',  ( 7.099999999999927702, 2.500000000000000000, 5.022947341949748790 ) ) ;
#94632 = AXIS2_PLACEMENT_3D ( 'NONE', #3956, #43903, #34077 ) ;
#94633 = FACE_BOUND ( 'NONE', #30464, .T. ) ;
#94634 = ORIENTED_EDGE ( 'NONE', *, *, #12843, .T. ) ;
#94635 = CARTESIAN_POINT ( 'NONE',  ( 186.1510416670080588, 4.367472073101518859, -7.564683531249999149 ) ) ;
#94636 = CARTESIAN_POINT ( 'NONE',  ( 10.59999999999991260, 2.500000000000000000, -0.3464101615137783474 ) ) ;
#94637 = DIRECTION ( 'NONE',  ( 0.000000000000000000, 0.000000000000000000, -1.000000000000000000 ) ) ;
#94638 = FACE_OUTER_BOUND ( 'NONE', #74420, .T. ) ;
#94639 = AXIS2_PLACEMENT_3D ( 'NONE', #88027, #38327, #65171 ) ;
#94641 = VECTOR ( 'NONE', #3936, 1000.000000000000000 ) ;
#94640 = CARTESIAN_POINT ( 'NONE',  ( -5.400000000000019895, 2.500000000000000000, 3.737306695894644371 ) ) ;
#94642 = CARTESIAN_POINT ( 'NONE',  ( -1.050000000000038236, 2.500000000000000000, -6.248780366869526759 ) ) ;
#94643 = ADVANCED_FACE ( 'NONE', ( #105594 ), #80114, .T. ) ;
#94644 = FACE_OUTER_BOUND ( 'NONE', #91387, .T. ) ;
#94645 = EDGE_CURVE ( 'NONE', #114219, #67325, #96820, .T. ) ;
#94646 = CONICAL_SURFACE ( 'NONE', #31985, 0.1000000000000002554, 0.003490658503988666988 ) ;
#94647 = CARTESIAN_POINT ( 'NONE',  ( -14.99999999999994671, 12.50000000000000000, 0.000000000000000000 ) ) ;
#94648 = EDGE_CURVE ( 'NONE', #84209, #20024, #21620, .T. ) ;
#94649 = AXIS2_PLACEMENT_3D ( 'NONE', #46797, #66417, #125346 ) ;
#94650 = VERTEX_POINT ( 'NONE', #117970 ) ;
#94651 = EDGE_LOOP ( 'NONE', ( #98159, #90896 ) ) ;
#94652 = ORIENTED_EDGE ( 'NONE', *, *, #48590, .T. ) ;
#94653 = ORIENTED_EDGE ( 'NONE', *, *, #32658, .F. ) ;
#94655 = VERTEX_POINT ( 'NONE', #5436 ) ;
#94654 = AXIS2_PLACEMENT_3D ( 'NONE', #81979, #32270, #29665 ) ;
#94656 = DIRECTION ( 'NONE',  ( 0.000000000000000000, -0.000000000000000000, 1.000000000000000000 ) ) ;
#94657 = VECTOR ( 'NONE', #33248, 1000.000000000000000 ) ;
#94658 = LINE ( 'NONE', #35126, #113495 ) ;
#94660 = EDGE_CURVE ( 'NONE', #31405, #59442, #15332, .T. ) ;
#94659 = ORIENTED_EDGE ( 'NONE', *, *, #68573, .F. ) ;
#94661 = FACE_BOUND ( 'NONE', #104609, .T. ) ;
#94662 = VECTOR ( 'NONE', #54807, 1000.000000000000000 ) ;
#94663 = LINE ( 'NONE', #123476, #31076 ) ;
#94664 = EDGE_CURVE ( 'NONE', #43749, #104669, #32099, .T. ) ;
#94665 = EDGE_CURVE ( 'NONE', #103959, #7038, #48729, .T. ) ;
#94666 = EDGE_CURVE ( 'NONE', #109430, #96170, #86353, .T. ) ;
#94667 = DIRECTION ( 'NONE',  ( 0.000000000000000000, 0.000000000000000000, 1.000000000000000000 ) ) ;
#94668 = VERTEX_POINT ( 'NONE', #119258 ) ;
#94669 = DIRECTION ( 'NONE',  ( 0.000000000000000000, 0.000000000000000000, -1.000000000000000000 ) ) ;
#94670 = CARTESIAN_POINT ( 'NONE',  ( 186.9166666666666856, 6.668395609140176816, 3.850000000000000977 ) ) ;
#94671 = CARTESIAN_POINT ( 'NONE',  ( 12.49999999999990230, 2.500000000000000000, -0.7928203230275542301 ) ) ;
#94672 = ORIENTED_EDGE ( 'NONE', *, *, #46165, .F. ) ;
#94673 = CARTESIAN_POINT ( 'NONE',  ( -6.900000000000019007, 2.500000000000000000, 0.3464101615137735735 ) ) ;
#94674 = EDGE_CURVE ( 'NONE', #69453, #94894, #8991, .T. ) ;
#94675 = AXIS2_PLACEMENT_3D ( 'NONE', #120075, #9472, #1573 ) ;
#94676 = VERTEX_POINT ( 'NONE', #110725 ) ;
#94677 = VERTEX_POINT ( 'NONE', #773 ) ;
#94678 = VERTEX_POINT ( 'NONE', #99636 ) ;
#94679 = DIRECTION ( 'NONE',  ( -0.000000000000000000, 1.000000000000000000, -0.000000000000000000 ) ) ;
#94680 = CARTESIAN_POINT ( 'NONE',  ( -7.900000000000014566, 2.500000000000000000, -4.330127018922201643 ) ) ;
#94681 = LINE ( 'NONE', #117517, #2865 ) ;
#94682 = ORIENTED_EDGE ( 'NONE', *, *, #66978, .F. ) ;
#94683 = CARTESIAN_POINT ( 'NONE',  ( 2.500000000000002220, 2.499999999999998668, -9.999999999999998224 ) ) ;
#94684 = CIRCLE ( 'NONE', #38268, 0.06509327318403745899 ) ;
#94686 = FACE_OUTER_BOUND ( 'NONE', #12278, .T. ) ;
#94685 = AXIS2_PLACEMENT_3D ( 'NONE', #37381, #77930, #98856 ) ;
#94687 = DIRECTION ( 'NONE',  ( 0.000000000000000000, 0.000000000000000000, 1.000000000000000000 ) ) ;
#94688 = CARTESIAN_POINT ( 'NONE',  ( 184.9479166673494603, -6.668395609140176816, -3.850000000000003642 ) ) ;
#94689 = CARTESIAN_POINT ( 'NONE',  ( 3.149999999999946176, 12.50000000000000000, -1.883746621131363375 ) ) ;
#94690 = DIRECTION ( 'NONE',  ( -4.274815082592931898E-19, -0.9999939076577903929, -0.003490651415223739937 ) ) ;
#94691 = ADVANCED_FACE ( 'NONE', ( #21056 ), #29596, .T. ) ;
#94692 = ORIENTED_EDGE ( 'NONE', *, *, #95051, .F. ) ;
#94693 = FACE_OUTER_BOUND ( 'NONE', #24659, .T. ) ;
#94694 = PRESENTATION_LAYER_ASSIGNMENT (  '', '', ( #48647 ) ) ;
#94695 = AXIS2_PLACEMENT_3D ( 'NONE', #66823, #28209, #26919 ) ;
#94696 = ORIENTED_EDGE ( 'NONE', *, *, #51225, .T. ) ;
#94697 = CONICAL_SURFACE ( 'NONE', #90486, 0.09999999999999999167, 0.003490658503988666988 ) ;
#94698 = ORIENTED_EDGE ( 'NONE', *, *, #113030, .T. ) ;
#94699 = CARTESIAN_POINT ( 'NONE',  ( 4.999999999999938716, 2.500000000000000000, -5.022947341949754119 ) ) ;
#94700 = DIRECTION ( 'NONE',  ( 0.000000000000000000, 1.000000000000000000, 0.000000000000000000 ) ) ;
#94701 = CARTESIAN_POINT ( 'NONE',  ( 13.54999999999989946, 2.500000000000000000, 2.511473670974873507 ) ) ;
#94702 = CARTESIAN_POINT ( 'NONE',  ( -8.350000000000012079, 2.500000000000000000, -1.572243186433550211 ) ) ;
#94703 = DIRECTION ( 'NONE',  ( 0.000000000000000000, -0.000000000000000000, 1.000000000000000000 ) ) ;
#94704 = AXIS2_PLACEMENT_3D ( 'NONE', #24784, #64696, #25398 ) ;
#94705 = ORIENTED_EDGE ( 'NONE', *, *, #39169, .F. ) ;
#94706 = ORIENTED_EDGE ( 'NONE', *, *, #46463, .T. ) ;
#94707 = DIRECTION ( 'NONE',  ( 0.000000000000000000, -0.000000000000000000, 1.000000000000000000 ) ) ;
#94708 = EDGE_CURVE ( 'NONE', #12428, #76477, #90429, .T. ) ;
#94710 = AXIS2_PLACEMENT_3D ( 'NONE', #72528, #112451, #22149 ) ;
#94709 = DIRECTION ( 'NONE',  ( 0.000000000000000000, -0.9999939076577903929, 0.003490651415223739937 ) ) ;
#94711 = VECTOR ( 'NONE', #92644, 1000.000000000000000 ) ;
#94712 = LINE ( 'NONE', #25313, #112973 ) ;
#94713 = ORIENTED_EDGE ( 'NONE', *, *, #119742, .F. ) ;
#94714 = ORIENTED_EDGE ( 'NONE', *, *, #84997, .T. ) ;
#94715 = CARTESIAN_POINT ( 'NONE',  ( 5.649999999999934630, 2.500000000000000000, -1.718653347947325827 ) ) ;
#94716 = AXIS2_PLACEMENT_3D ( 'NONE', #88870, #90136, #39792 ) ;
#94717 = ORIENTED_EDGE ( 'NONE', *, *, #105764, .T. ) ;
#94718 = CARTESIAN_POINT ( 'NONE',  ( -7.500000000000013323, 2.500000000000000000, 4.922947341949748257 ) ) ;
#94719 = DIRECTION ( 'NONE',  ( 0.000000000000000000, 1.000000000000000000, 0.000000000000000000 ) ) ;
#94720 = ORIENTED_EDGE ( 'NONE', *, *, #106725, .T. ) ;
#94721 = CIRCLE ( 'NONE', #82210, 0.06509327318403745899 ) ;
#94722 = CARTESIAN_POINT ( 'NONE',  ( 0.1999999999999576006, 12.50000000000000000, -4.676537180435978769 ) ) ;
#94723 = CARTESIAN_POINT ( 'NONE',  ( 5.399999999999936406, 12.50000000000000000, -5.022947341949754119 ) ) ;
#94724 = CARTESIAN_POINT ( 'NONE',  ( 3.749999999999940492, 12.50000000000000000, 2.857883832488649301 ) ) ;
#94725 = EDGE_CURVE ( 'NONE', #97446, #54303, #19788, .T. ) ;
#94726 = CARTESIAN_POINT ( 'NONE',  ( -6.249999999999984901, 2.500000000000000000, -6.395190528383301931 ) ) ;
#94727 = EDGE_LOOP ( 'NONE', ( #61700, #6119 ) ) ;
#94728 = LINE ( 'NONE', #55458, #121891 ) ;
#94729 = DIRECTION ( 'NONE',  ( -0.000000000000000000, 1.000000000000000000, -0.000000000000000000 ) ) ;
#94730 = ORIENTED_EDGE ( 'NONE', *, *, #38153, .T. ) ;
#94731 = ORIENTED_EDGE ( 'NONE', *, *, #100387, .T. ) ;
#94732 = CIRCLE ( 'NONE', #52973, 0.09999999999999982514 ) ;
#94733 = AXIS2_PLACEMENT_3D ( 'NONE', #69309, #11691, #9763 ) ;
#94734 = CARTESIAN_POINT ( 'NONE',  ( 184.5052083336747444, -6.551208109652278289, 3.782341765624995134 ) ) ;
#94735 = DIRECTION ( 'NONE',  ( 0.000000000000000000, -0.000000000000000000, 1.000000000000000000 ) ) ;
#94736 = DIRECTION ( 'NONE',  ( 0.000000000000000000, 1.000000000000000000, 0.000000000000000000 ) ) ;
#94737 = DIRECTION ( 'NONE',  ( 0.000000000000000000, 0.000000000000000000, 1.000000000000000000 ) ) ;
#94738 = CARTESIAN_POINT ( 'NONE',  ( -11.05000000000000249, 2.500000000000000000, -1.918653347947322230 ) ) ;
#94739 = VECTOR ( 'NONE', #107671, 1000.000000000000000 ) ;
#94740 = DIRECTION ( 'NONE',  ( 0.000000000000000000, 0.000000000000000000, -1.000000000000000000 ) ) ;
#94741 = VECTOR ( 'NONE', #57646, 1000.000000000000000 ) ;
#94742 = DIRECTION ( 'NONE',  ( 0.000000000000000000, -0.9999939076577903929, 0.003490651415223739937 ) ) ;
#94743 = DIRECTION ( 'NONE',  ( 0.000000000000000000, 0.000000000000000000, 1.000000000000000000 ) ) ;
#94745 = CIRCLE ( 'NONE', #40386, 0.1000000000000002554 ) ;
#94744 = DIRECTION ( 'NONE',  ( 0.000000000000000000, 0.000000000000000000, 1.000000000000000000 ) ) ;
#94746 = AXIS2_PLACEMENT_3D ( 'NONE', #115493, #65757, #114229 ) ;
#94747 = CARTESIAN_POINT ( 'NONE',  ( -5.850000000000019185, 12.50000000000000000, 6.495190528383297135 ) ) ;
#94748 = EDGE_LOOP ( 'NONE', ( #64907, #99265, #91870, #109563 ) ) ;
#94749 = CONICAL_SURFACE ( 'NONE', #126147, 0.1000000000000002554, 0.003490658503988666988 ) ;
#94750 = VERTEX_POINT ( 'NONE', #88506 ) ;
#94751 = CIRCLE ( 'NONE', #11214, 0.1000000000000002554 ) ;
#94753 = ADVANCED_FACE ( 'NONE', ( #100901 ), #69511, .T. ) ;
#94752 = CONICAL_SURFACE ( 'NONE', #84289, 0.1000000000000002554, 0.003490658503988666988 ) ;
#94754 = ORIENTED_EDGE ( 'NONE', *, *, #49552, .T. ) ;
#94755 = VECTOR ( 'NONE', #1806, 1000.000000000000000 ) ;
#94756 = AXIS2_PLACEMENT_3D ( 'NONE', #28909, #26330, #96991 ) ;
#94757 = ORIENTED_EDGE ( 'NONE', *, *, #44111, .F. ) ;
#94758 = DIRECTION ( 'NONE',  ( -0.000000000000000000, -1.000000000000000000, -0.000000000000000000 ) ) ;
#94759 = DIRECTION ( 'NONE',  ( 0.000000000000000000, 0.000000000000000000, 1.000000000000000000 ) ) ;
#94760 = CARTESIAN_POINT ( 'NONE',  ( 11.84999999999990372, 12.50000000000000000, -6.841600689897078702 ) ) ;
#94762 = EDGE_CURVE ( 'NONE', #88981, #22544, #98324, .T. ) ;
#94761 = AXIS2_PLACEMENT_3D ( 'NONE', #67520, #47922, #127756 ) ;
#94763 = ORIENTED_EDGE ( 'NONE', *, *, #119266, .T. ) ;
#94764 = DIRECTION ( 'NONE',  ( 0.000000000000000000, 1.000000000000000000, 0.000000000000000000 ) ) ;
#94765 = CARTESIAN_POINT ( 'NONE',  ( -11.64999999999999680, 2.500000000000000000, -2.757883832488650100 ) ) ;
#94767 = ORIENTED_EDGE ( 'NONE', *, *, #103073, .F. ) ;
#94766 = CARTESIAN_POINT ( 'NONE',  ( -9.800000000000007816, 12.50000000000000000, -3.918623584224384615 ) ) ;
#94768 = EDGE_CURVE ( 'NONE', #37234, #6735, #115688, .T. ) ;
#94769 = EDGE_CURVE ( 'NONE', #70723, #26135, #48602, .T. ) ;
#94770 = EDGE_CURVE ( 'NONE', #127507, #112646, #71899, .T. ) ;
#94771 = EDGE_CURVE ( 'NONE', #43418, #65087, #34253, .T. ) ;
#94773 = DIRECTION ( 'NONE',  ( 0.000000000000000000, 1.000000000000000000, 0.000000000000000000 ) ) ;
#94772 = CONICAL_SURFACE ( 'NONE', #57114, 0.09999999999999982514, 0.003490658503988666988 ) ;
#94774 = ORIENTED_EDGE ( 'NONE', *, *, #42177, .T. ) ;
#94775 = VERTEX_POINT ( 'NONE', #78719 ) ;
#94776 = VERTEX_POINT ( 'NONE', #11232 ) ;
#94777 = ORIENTED_EDGE ( 'NONE', *, *, #2644, .F. ) ;
#94778 = DIRECTION ( 'NONE',  ( 0.000000000000000000, 1.000000000000000000, 0.000000000000000000 ) ) ;
#94779 = ADVANCED_FACE ( 'NONE', ( #79359 ), #15426, .T. ) ;
#94781 = AXIS2_PLACEMENT_3D ( 'NONE', #111180, #115696, #122960 ) ;
#94780 = DIRECTION ( 'NONE',  ( 0.000000000000000000, 0.000000000000000000, 1.000000000000000000 ) ) ;
#94782 = FACE_OUTER_BOUND ( 'NONE', #55667, .T. ) ;
#94784 = EDGE_CURVE ( 'NONE', #60953, #124470, #61440, .T. ) ;
#94783 = AXIS2_PLACEMENT_3D ( 'NONE', #79384, #49291, #118646 ) ;
#94785 = CARTESIAN_POINT ( 'NONE',  ( -8.100000000000013856, 2.500000000000000000, -0.3464101615137782364 ) ) ;
#94786 = AXIS2_PLACEMENT_3D ( 'NONE', #12825, #10891, #102521 ) ;
#94788 = ORIENTED_EDGE ( 'NONE', *, *, #73819, .T. ) ;
#94787 = EDGE_CURVE ( 'NONE', #40128, #96953, #9184, .T. ) ;
#94789 = DIRECTION ( 'NONE',  ( 0.000000000000000000, 1.000000000000000000, 0.000000000000000000 ) ) ;
#94790 = ORIENTED_EDGE ( 'NONE', *, *, #116178, .F. ) ;
#94791 = CARTESIAN_POINT ( 'NONE',  ( 87.50000000000001421, -3.974992050023849810, -6.359987280038161828 ) ) ;
#94792 = DIRECTION ( 'NONE',  ( -0.000000000000000000, 1.000000000000000000, -0.000000000000000000 ) ) ;
#94793 = CARTESIAN_POINT ( 'NONE',  ( 14.59999999999989484, 2.500000000000000000, -2.276824562219559311E-15 ) ) ;
#94794 = CARTESIAN_POINT ( 'NONE',  ( 16.84158739990380482, -0.4722467112502861109, 5.802037699230406353 ) ) ;
#94795 = CONICAL_SURFACE ( 'NONE', #98994, 0.09999999999999982514, 0.003490658503988666988 ) ;
#94796 = VECTOR ( 'NONE', #47579, 1000.000000000000000 ) ;
#94797 = AXIS2_PLACEMENT_3D ( 'NONE', #108696, #79252, #48490 ) ;
#94798 = EDGE_LOOP ( 'NONE', ( #118465, #76188 ) ) ;
#94799 = ORIENTED_EDGE ( 'NONE', *, *, #8511, .T. ) ;
#94800 = EDGE_LOOP ( 'NONE', ( #83571, #100516, #100655, #19420 ) ) ;
#94801 = CARTESIAN_POINT ( 'NONE',  ( 7.899999999999924860, 2.500000000000000000, 4.430127018922196847 ) ) ;
#94802 = CARTESIAN_POINT ( 'NONE',  ( 10.19999999999991402, 2.500000000000000000, 0.3464101615137735735 ) ) ;
#94803 = CARTESIAN_POINT ( 'NONE',  ( -11.84999999999999609, 2.500000000000000000, 6.148780366869520897 ) ) ;
#94804 = FACE_BOUND ( 'NONE', #79943, .T. ) ;
#94805 = VECTOR ( 'NONE', #5005, 1000.000000000000000 ) ;
#94806 = DIRECTION ( 'NONE',  ( 0.000000000000000000, 1.000000000000000000, 0.000000000000000000 ) ) ;
#94807 = CARTESIAN_POINT ( 'NONE',  ( 3.549999999999942091, 2.500000000000000000, 2.411473670974873862 ) ) ;
#94808 = DIRECTION ( 'NONE',  ( -0.000000000000000000, -1.000000000000000000, -0.000000000000000000 ) ) ;
#94809 = AXIS2_PLACEMENT_3D ( 'NONE', #120718, #81446, #92539 ) ;
#94810 = AXIS2_PLACEMENT_3D ( 'NONE', #26492, #16641, #96490 ) ;
#94811 = AXIS2_PLACEMENT_3D ( 'NONE', #125453, #105820, #64600 ) ;
#94812 = CARTESIAN_POINT ( 'NONE',  ( -1.900000000000034994, 12.50000000000000000, -4.741630453620016006 ) ) ;
#94813 = DIRECTION ( 'NONE',  ( 0.000000000000000000, 0.000000000000000000, 1.000000000000000000 ) ) ;
#94814 = AXIS2_PLACEMENT_3D ( 'NONE', #89367, #18683, #129314 ) ;
#94815 = DIRECTION ( 'NONE',  ( 0.000000000000000000, 1.000000000000000000, 0.000000000000000000 ) ) ;
#94816 = ORIENTED_EDGE ( 'NONE', *, *, #114389, .F. ) ;
#94817 = FACE_OUTER_BOUND ( 'NONE', #49570, .T. ) ;
#94818 = ORIENTED_EDGE ( 'NONE', *, *, #27506, .F. ) ;
#94819 = VERTEX_POINT ( 'NONE', #41374 ) ;
#94820 = EDGE_LOOP ( 'NONE', ( #55016, #93981, #77851, #25146 ) ) ;
#94821 = ORIENTED_EDGE ( 'NONE', *, *, #6678, .F. ) ;
#94822 = CARTESIAN_POINT ( 'NONE',  ( 1.849999999999950573, 2.500000000000000000, -1.718653347947326049 ) ) ;
#94823 = EDGE_CURVE ( 'NONE', #47303, #105454, #59293, .T. ) ;
#94824 = FACE_BOUND ( 'NONE', #94458, .T. ) ;
#94825 = FACE_OUTER_BOUND ( 'NONE', #16704, .T. ) ;
#94826 = EDGE_CURVE ( 'NONE', #22036, #8336, #88609, .T. ) ;
#94827 = ADVANCED_FACE ( 'NONE', ( #61650 ), #104141, .T. ) ;
#94828 = ORIENTED_EDGE ( 'NONE', *, *, #14338, .F. ) ;
#94830 = AXIS2_PLACEMENT_3D ( 'NONE', #20949, #90978, #1304 ) ;
#94829 = CARTESIAN_POINT ( 'NONE',  ( 35.03103265460730142, 3.271231620377792026, 3.345711933278367578 ) ) ;
#94831 = DIRECTION ( 'NONE',  ( 0.000000000000000000, -0.000000000000000000, 1.000000000000000000 ) ) ;
#94832 = ORIENTED_EDGE ( 'NONE', *, *, #116344, .F. ) ;
#94833 = CARTESIAN_POINT ( 'NONE',  ( 184.5000000000000000, 0.000000000000000000, 0.000000000000000000 ) ) ;
#94834 = DIRECTION ( 'NONE',  ( -0.000000000000000000, 1.000000000000000000, -0.000000000000000000 ) ) ;
#94835 = ADVANCED_FACE ( 'NONE', ( #34774 ), #11882, .T. ) ;
#94836 = AXIS2_PLACEMENT_3D ( 'NONE', #53273, #93194, #84652 ) ;
#94837 = CIRCLE ( 'NONE', #69704, 0.1000000000000002554 ) ;
#94838 = VECTOR ( 'NONE', #67259, 1000.000000000000000 ) ;
#94839 = AXIS2_PLACEMENT_3D ( 'NONE', #16763, #96618, #6940 ) ;
#94840 = CIRCLE ( 'NONE', #32171, 0.09999999999999982514 ) ;
#94841 = ORIENTED_EDGE ( 'NONE', *, *, #16176, .F. ) ;
#94842 = FACE_OUTER_BOUND ( 'NONE', #27131, .T. ) ;
#94843 = CARTESIAN_POINT ( 'NONE',  ( 4.599999999999940137, 12.50000000000000000, -4.265033745738164406 ) ) ;
#94844 = CIRCLE ( 'NONE', #73912, 0.09999999999999982514 ) ;
#94846 = EDGE_LOOP ( 'NONE', ( #62498, #16570 ) ) ;
#94845 = AXIS2_PLACEMENT_3D ( 'NONE', #15156, #95043, #106144 ) ;
#94847 = AXIS2_PLACEMENT_3D ( 'NONE', #37526, #117319, #27672 ) ;
#94848 = CARTESIAN_POINT ( 'NONE',  ( 8.349999999999919709, 2.500000000000000000, -2.757883832488654097 ) ) ;
#94849 = CARTESIAN_POINT ( 'NONE',  ( 12.09999999999990195, 12.50000000000000000, 0.7579135962115869374 ) ) ;
#94850 = DIRECTION ( 'NONE',  ( 0.000000000000000000, 0.000000000000000000, 1.000000000000000000 ) ) ;
#94852 = EDGE_LOOP ( 'NONE', ( #7228, #108660 ) ) ;
#94851 = AXIS2_PLACEMENT_3D ( 'NONE', #96824, #28100, #117098 ) ;
#94853 = ORIENTED_EDGE ( 'NONE', *, *, #43503, .F. ) ;
#94854 = CARTESIAN_POINT ( 'NONE',  ( 0.000000000000000000, 0.000000000000000000, -5.000000000000004441 ) ) ;
#94855 = EDGE_CURVE ( 'NONE', #41716, #40814, #92375, .T. ) ;
#94856 = VERTEX_POINT ( 'NONE', #123760 ) ;
#94857 = DIRECTION ( 'NONE',  ( 0.000000000000000000, 0.000000000000000000, 1.000000000000000000 ) ) ;
#94858 = DIRECTION ( 'NONE',  ( 0.000000000000000000, 1.000000000000000000, 0.000000000000000000 ) ) ;
#94859 = ORIENTED_EDGE ( 'NONE', *, *, #125823, .T. ) ;
#94860 = CARTESIAN_POINT ( 'NONE',  ( 115.5000000000000000, -1.500000000000000222, -1.322875655532295136 ) ) ;
#94861 = CARTESIAN_POINT ( 'NONE',  ( -8.750000000000012434, 2.500000000000000000, -5.802370205355744659 ) ) ;
#94862 = DIRECTION ( 'NONE',  ( 0.000000000000000000, 0.000000000000000000, 1.000000000000000000 ) ) ;
#94863 = FACE_OUTER_BOUND ( 'NONE', #119445, .T. ) ;
#94864 = CARTESIAN_POINT ( 'NONE',  ( -5.400000000000024336, 2.500000000000000000, -3.537306695894649966 ) ) ;
#94865 = AXIS2_PLACEMENT_3D ( 'NONE', #81284, #59067, #98984 ) ;
#94866 = VERTEX_POINT ( 'NONE', #41999 ) ;
#94867 = EDGE_LOOP ( 'NONE', ( #3628, #58086, #66817, #8052 ) ) ;
#94868 = CARTESIAN_POINT ( 'NONE',  ( -2.700000000000031264, 12.50000000000000000, 4.611443907251934426 ) ) ;
#94869 = ADVANCED_FACE ( 'NONE', ( #43943 ), #23777, .T. ) ;
#94870 = CARTESIAN_POINT ( 'NONE',  ( 2.099999999999949463, 12.50000000000000000, -3.702399969078687292 ) ) ;
#94871 = CARTESIAN_POINT ( 'NONE',  ( -0.6500000000000398792, 12.50000000000000000, -6.776507416713040577 ) ) ;
#94873 = ORIENTED_EDGE ( 'NONE', *, *, #77036, .T. ) ;
#94872 = ORIENTED_EDGE ( 'NONE', *, *, #113301, .F. ) ;
#94874 = ORIENTED_EDGE ( 'NONE', *, *, #49018, .T. ) ;
#94875 = DIRECTION ( 'NONE',  ( -0.000000000000000000, -1.000000000000000000, -0.000000000000000000 ) ) ;
#94876 = VECTOR ( 'NONE', #95278, 1000.000000000000000 ) ;
#94877 = AXIS2_PLACEMENT_3D ( 'NONE', #60402, #50543, #21090 ) ;
#94878 = DIRECTION ( 'NONE',  ( 0.000000000000000000, 1.000000000000000000, 0.000000000000000000 ) ) ;
#94879 = AXIS2_PLACEMENT_3D ( 'NONE', #54388, #72752, #24294 ) ;
#94880 = CARTESIAN_POINT ( 'NONE',  ( 6.449999999999931788, 2.500000000000000000, 6.248780366869520542 ) ) ;
#94881 = CARTESIAN_POINT ( 'NONE',  ( -10.65000000000000213, 12.50000000000000000, 6.148780366869520009 ) ) ;
#94882 = FACE_OUTER_BOUND ( 'NONE', #75536, .T. ) ;
#94883 = DIRECTION ( 'NONE',  ( -0.000000000000000000, 1.000000000000000000, -0.000000000000000000 ) ) ;
#94884 = FACE_OUTER_BOUND ( 'NONE', #7771, .T. ) ;
#94885 = DIRECTION ( 'NONE',  ( -0.000000000000000000, -1.000000000000000000, -0.000000000000000000 ) ) ;
#94886 = EDGE_CURVE ( 'NONE', #125089, #26581, #40516, .T. ) ;
#94887 = VECTOR ( 'NONE', #103187, 1000.000000000000000 ) ;
#94888 = VECTOR ( 'NONE', #50797, 1000.000000000000000 ) ;
#94889 = CARTESIAN_POINT ( 'NONE',  ( 14.34999999999989662, 12.50000000000000000, 2.511473670974873507 ) ) ;
#94890 = AXIS2_PLACEMENT_3D ( 'NONE', #40303, #101799, #41603 ) ;
#94891 = ORIENTED_EDGE ( 'NONE', *, *, #57268, .T. ) ;
#94892 = VECTOR ( 'NONE', #57929, 1000.000000000000000 ) ;
#94893 = DIRECTION ( 'NONE',  ( 0.000000000000000000, 0.000000000000000000, 1.000000000000000000 ) ) ;
#94894 = VERTEX_POINT ( 'NONE', #84504 ) ;
#94895 = EDGE_CURVE ( 'NONE', #44501, #3248, #67666, .T. ) ;
#94896 = ORIENTED_EDGE ( 'NONE', *, *, #66308, .F. ) ;
#94897 = DIRECTION ( 'NONE',  ( 0.000000000000000000, 1.000000000000000000, 0.000000000000000000 ) ) ;
#94898 = DIRECTION ( 'NONE',  ( -4.274815082592931898E-19, -0.9999939076577903929, -0.003490651415223739937 ) ) ;
#94899 = DIRECTION ( 'NONE',  ( 0.000000000000000000, -0.000000000000000000, 1.000000000000000000 ) ) ;
#94900 = DIRECTION ( 'NONE',  ( 0.000000000000000000, -1.000000000000000000, -0.000000000000000000 ) ) ;
#94901 = DIRECTION ( 'NONE',  ( -0.000000000000000000, 1.000000000000000000, -0.000000000000000000 ) ) ;
#94902 = CIRCLE ( 'NONE', #107420, 0.1000000000000000472 ) ;
#94903 = CARTESIAN_POINT ( 'NONE',  ( 2.049999999999948308, 12.50000000000000000, 6.560283801567334372 ) ) ;
#94904 = AXIS2_PLACEMENT_3D ( 'NONE', #9189, #2571, #43185 ) ;
#94905 = CONICAL_SURFACE ( 'NONE', #38494, 0.1000000000000002554, 0.003490658503988666988 ) ;
#94906 = DIRECTION ( 'NONE',  ( -0.000000000000000000, 1.000000000000000000, -0.000000000000000000 ) ) ;
#94907 = VERTEX_POINT ( 'NONE', #2057 ) ;
#94908 = DIRECTION ( 'NONE',  ( -0.000000000000000000, 1.000000000000000000, -0.000000000000000000 ) ) ;
#94909 = AXIS2_PLACEMENT_3D ( 'NONE', #129160, #19150, #79396 ) ;
#94910 = CIRCLE ( 'NONE', #25961, 0.1000000000000000056 ) ;
#94911 = CARTESIAN_POINT ( 'NONE',  ( -5.800000000000022027, 2.500000000000000000, -4.430127018922202176 ) ) ;
#94912 = ORIENTED_EDGE ( 'NONE', *, *, #67128, .F. ) ;
#94913 = ORIENTED_EDGE ( 'NONE', *, *, #90693, .T. ) ;
#94914 = EDGE_CURVE ( 'NONE', #18083, #60727, #17480, .T. ) ;
#94915 = ORIENTED_EDGE ( 'NONE', *, *, #112627, .T. ) ;
#94916 = ORIENTED_EDGE ( 'NONE', *, *, #87515, .F. ) ;
#94917 = CARTESIAN_POINT ( 'NONE',  ( 9.599999999999914380, 2.500000000000000000, -5.022947341949754119 ) ) ;
#94918 = CARTESIAN_POINT ( 'NONE',  ( -3.750000000000031086, 12.50000000000000000, -5.802370205355749988 ) ) ;
#94919 = EDGE_CURVE ( 'NONE', #113079, #100019, #101134, .T. ) ;
#94920 = DIRECTION ( 'NONE',  ( 0.000000000000000000, 0.000000000000000000, 1.000000000000000000 ) ) ;
#94921 = DIRECTION ( 'NONE',  ( 0.000000000000000000, 0.000000000000000000, 1.000000000000000000 ) ) ;
#94922 = VECTOR ( 'NONE', #63355, 1000.000000000000000 ) ;
#94923 = DIRECTION ( 'NONE',  ( 0.000000000000000000, -0.9999939076577903929, 0.003490651415223739937 ) ) ;
#94924 = ORIENTED_EDGE ( 'NONE', *, *, #41000, .F. ) ;
#94926 = CONICAL_SURFACE ( 'NONE', #53173, 0.09999999999999982514, 0.003490658503988666988 ) ;
#94925 = DIRECTION ( 'NONE',  ( -0.000000000000000000, 1.000000000000000000, -0.000000000000000000 ) ) ;
#94927 = EDGE_CURVE ( 'NONE', #92392, #117253, #57212, .T. ) ;
#94928 = VECTOR ( 'NONE', #43686, 1000.000000000000000 ) ;
#94929 = ADVANCED_FACE ( 'NONE', ( #94304 ), #111358, .T. ) ;
#94930 = ADVANCED_FACE ( 'NONE', ( #73379 ), #90659, .T. ) ;
#94931 = DIRECTION ( 'NONE',  ( 0.000000000000000000, 1.000000000000000000, 0.000000000000000000 ) ) ;
#94932 = EDGE_CURVE ( 'NONE', #100183, #104358, #22377, .T. ) ;
#94933 = CARTESIAN_POINT ( 'NONE',  ( 165.4999999999999716, 0.000000000000000000, 2.000000000000000000 ) ) ;
#94934 = EDGE_LOOP ( 'NONE', ( #9774, #116566, #26217, #59766 ) ) ;
#94935 = CIRCLE ( 'NONE', #2999, 0.06509327318403745899 ) ;
#94936 = CIRCLE ( 'NONE', #38519, 0.06509327318403745899 ) ;
#94937 = VECTOR ( 'NONE', #98454, 1000.000000000000000 ) ;
#94938 = ORIENTED_EDGE ( 'NONE', *, *, #96541, .F. ) ;
#94939 = CIRCLE ( 'NONE', #63548, 0.06509327318403745899 ) ;
#94941 = ORIENTED_EDGE ( 'NONE', *, *, #5831, .T. ) ;
#94940 = EDGE_CURVE ( 'NONE', #89101, #99935, #103501, .T. ) ;
#94942 = CARTESIAN_POINT ( 'NONE',  ( 4.149999999999939959, 12.50000000000000000, -6.495190528383302464 ) ) ;
#94943 = ADVANCED_FACE ( 'NONE', ( #122498 ), #4966, .T. ) ;
#94944 = EDGE_CURVE ( 'NONE', #18483, #54425, #113650, .T. ) ;
#94945 = DIRECTION ( 'NONE',  ( 0.000000000000000000, 1.000000000000000000, 0.000000000000000000 ) ) ;
#94946 = PLANE ( 'NONE',  #64 ) ;
#94947 = CIRCLE ( 'NONE', #63554, 0.1000000000000002554 ) ;
#94948 = EDGE_CURVE ( 'NONE', #92599, #29210, #72750, .T. ) ;
#94949 = AXIS2_PLACEMENT_3D ( 'NONE', #66851, #35482, #76687 ) ;
#94950 = CIRCLE ( 'NONE', #53193, 0.06509327318403745899 ) ;
#94951 = EDGE_CURVE ( 'NONE', #40542, #12969, #84397, .T. ) ;
#94952 = VECTOR ( 'NONE', #58224, 1000.000000000000000 ) ;
#94953 = ORIENTED_EDGE ( 'NONE', *, *, #13443, .T. ) ;
#94954 = DIRECTION ( 'NONE',  ( -0.000000000000000000, 1.000000000000000000, -0.000000000000000000 ) ) ;
#94955 = FACE_OUTER_BOUND ( 'NONE', #50983, .T. ) ;
#94956 = CARTESIAN_POINT ( 'NONE',  ( 3.749999999999975131, 12.50000000000000000, 6.495190528383297135 ) ) ;
#94957 = CARTESIAN_POINT ( 'NONE',  ( -10.40000000000000213, 2.500000000000000000, -0.6928203230275541413 ) ) ;
#94958 = CARTESIAN_POINT ( 'NONE',  ( 10.19999999999991402, 2.500000000000000000, 0.3464101615137735735 ) ) ;
#94959 = EDGE_CURVE ( 'NONE', #36386, #11332, #105333, .T. ) ;
#94960 = ORIENTED_EDGE ( 'NONE', *, *, #116067, .F. ) ;
#94961 = LINE ( 'NONE', #83208, #127199 ) ;
#94962 = ORIENTED_EDGE ( 'NONE', *, *, #29798, .F. ) ;
#94963 = ORIENTED_EDGE ( 'NONE', *, *, #320, .F. ) ;
#94964 = VERTEX_POINT ( 'NONE', #7208 ) ;
#94965 = CARTESIAN_POINT ( 'NONE',  ( -2.050000000000033129, 2.500000000000000000, 2.165063509461097713 ) ) ;
#94966 = FACE_BOUND ( 'NONE', #1656, .T. ) ;
#94967 = DIRECTION ( 'NONE',  ( -0.000000000000000000, -1.000000000000000000, -0.000000000000000000 ) ) ;
#94968 = FACE_OUTER_BOUND ( 'NONE', #116039, .T. ) ;
#94969 = DIRECTION ( 'NONE',  ( 0.000000000000000000, 0.000000000000000000, 1.000000000000000000 ) ) ;
#94970 = EDGE_LOOP ( 'NONE', ( #6557, #79110, #37789, #38175 ) ) ;
#94971 = DIRECTION ( 'NONE',  ( 0.000000000000000000, 1.000000000000000000, 0.000000000000000000 ) ) ;
#94972 = CARTESIAN_POINT ( 'NONE',  ( 10.84999999999990905, 2.500000000000000000, 1.472243186433545459 ) ) ;
#94973 = FACE_OUTER_BOUND ( 'NONE', #13567, .T. ) ;
#94974 = CARTESIAN_POINT ( 'NONE',  ( 9.599999999999917932, 12.50000000000000000, 0.6928203230275494784 ) ) ;
#94975 = ORIENTED_EDGE ( 'NONE', *, *, #21504, .F. ) ;
#94976 = AXIS2_PLACEMENT_3D ( 'NONE', #5945, #43967, #66168 ) ;
#94977 = AXIS2_PLACEMENT_3D ( 'NONE', #109294, #60845, #100746 ) ;
#94978 = DIRECTION ( 'NONE',  ( 0.000000000000000000, 1.000000000000000000, 0.000000000000000000 ) ) ;
#94979 = DIRECTION ( 'NONE',  ( 0.000000000000000000, 1.000000000000000000, 0.000000000000000000 ) ) ;
#94980 = VERTEX_POINT ( 'NONE', #26231 ) ;
#94981 = CARTESIAN_POINT ( 'NONE',  ( -7.100000000000014744, 12.50000000000000000, 4.395220292106234439 ) ) ;
#94982 = ORIENTED_EDGE ( 'NONE', *, *, #109076, .T. ) ;
#94983 = FACE_BOUND ( 'NONE', #42286, .T. ) ;
#94984 = CARTESIAN_POINT ( 'NONE',  ( 10.59999999999990905, 12.50000000000000000, 3.983716857408420076 ) ) ;
#94985 = VECTOR ( 'NONE', #23144, 1000.000000000000000 ) ;
#94986 = ADVANCED_FACE ( 'NONE', ( #77260 ), #19563, .T. ) ;
#94987 = ORIENTED_EDGE ( 'NONE', *, *, #104064, .F. ) ;
#94988 = CARTESIAN_POINT ( 'NONE',  ( -10.00000000000000355, 12.50000000000000000, -0.6928203230275541413 ) ) ;
#94989 = CARTESIAN_POINT ( 'NONE',  ( 3.549999999999940314, 2.500000000000000000, 6.841600689897072485 ) ) ;
#94990 = EDGE_CURVE ( 'NONE', #73565, #42572, #82267, .T. ) ;
#94991 = VERTEX_POINT ( 'NONE', #65493 ) ;
#94992 = EDGE_LOOP ( 'NONE', ( #126066, #9403, #3209, #112487 ) ) ;
#94993 = CARTESIAN_POINT ( 'NONE',  ( 186.1302083336747444, -4.367472073101514418, -7.564683531250002702 ) ) ;
#94994 = ORIENTED_EDGE ( 'NONE', *, *, #98927, .F. ) ;
#94995 = DIRECTION ( 'NONE',  ( 0.000000000000000000, 0.000000000000000000, 1.000000000000000000 ) ) ;
#94996 = DIRECTION ( 'NONE',  ( 0.000000000000000000, 1.000000000000000000, 0.000000000000000000 ) ) ;
#94997 = EDGE_CURVE ( 'NONE', #123263, #87864, #104757, .T. ) ;
#94998 = AXIS2_PLACEMENT_3D ( 'NONE', #24298, #3998, #104145 ) ;
#94999 = AXIS2_PLACEMENT_3D ( 'NONE', #1427, #102842, #13168 ) ;
#95000 = CARTESIAN_POINT ( 'NONE',  ( 14.14999999999989733, 2.500000000000000000, 2.957883832488649389 ) ) ;
#95001 = DIRECTION ( 'NONE',  ( 0.000000000000000000, 1.000000000000000000, 0.000000000000000000 ) ) ;
#95002 = DIRECTION ( 'NONE',  ( 0.000000000000000000, 0.000000000000000000, 1.000000000000000000 ) ) ;
#95003 = AXIS2_PLACEMENT_3D ( 'NONE', #80686, #121242, #30947 ) ;
#95004 = DIRECTION ( 'NONE',  ( -1.000000000000000000, -0.000000000000000000, -0.000000000000000000 ) ) ;
#95005 = CIRCLE ( 'NONE', #32337, 0.06509327318403745899 ) ;
#95006 = ORIENTED_EDGE ( 'NONE', *, *, #82237, .T. ) ;
#95007 = ORIENTED_EDGE ( 'NONE', *, *, #16278, .F. ) ;
#95008 = CARTESIAN_POINT ( 'NONE',  ( 8.549999999999922551, 2.500000000000000000, 2.611473670974873151 ) ) ;
#95009 = DIRECTION ( 'NONE',  ( 0.000000000000000000, 0.000000000000000000, -1.000000000000000000 ) ) ;
#95010 = DIRECTION ( 'NONE',  ( 0.000000000000000000, 1.000000000000000000, 0.000000000000000000 ) ) ;
#95011 = CARTESIAN_POINT ( 'NONE',  ( 11.84999999999990372, 12.50000000000000000, -6.213873640053564351 ) ) ;
#95013 = ORIENTED_EDGE ( 'NONE', *, *, #119973, .F. ) ;
#95012 = EDGE_LOOP ( 'NONE', ( #29387, #54573 ) ) ;
#95014 = FACE_BOUND ( 'NONE', #37587, .T. ) ;
#95015 = ORIENTED_EDGE ( 'NONE', *, *, #96121, .F. ) ;
#95016 = DIRECTION ( 'NONE',  ( -0.000000000000000000, 1.000000000000000000, -0.000000000000000000 ) ) ;
#95017 = DIRECTION ( 'NONE',  ( 0.000000000000000000, 1.000000000000000000, 0.000000000000000000 ) ) ;
#95018 = EDGE_LOOP ( 'NONE', ( #3760, #112067, #50773, #42450 ) ) ;
#95019 = DIRECTION ( 'NONE',  ( 0.000000000000000000, 0.000000000000000000, 1.000000000000000000 ) ) ;
#95020 = FACE_OUTER_BOUND ( 'NONE', #65814, .T. ) ;
#95021 = FACE_OUTER_BOUND ( 'NONE', #87520, .T. ) ;
#95023 = DIRECTION ( 'NONE',  ( -0.000000000000000000, 1.000000000000000000, -0.000000000000000000 ) ) ;
#95022 = VECTOR ( 'NONE', #29540, 1000.000000000000000 ) ;
#95024 = CIRCLE ( 'NONE', #72042, 0.06509327318403741736 ) ;
#95025 = DIRECTION ( 'NONE',  ( 0.000000000000000000, 0.000000000000000000, 1.000000000000000000 ) ) ;
#95026 = DIRECTION ( 'NONE',  ( 0.000000000000000000, 0.000000000000000000, 1.000000000000000000 ) ) ;
#95027 = CIRCLE ( 'NONE', #23925, 0.06509327318403745899 ) ;
#95028 = CARTESIAN_POINT ( 'NONE',  ( 186.9010416670080588, -4.367472073101520635, 7.564683531249999149 ) ) ;
#95029 = CARTESIAN_POINT ( 'NONE',  ( 3.549999999999944755, 2.500000000000000000, -6.941600689897077459 ) ) ;
#95030 = CARTESIAN_POINT ( 'NONE',  ( 10.64999999999991331, 12.50000000000000000, 6.841600689897072485 ) ) ;
#95031 = ADVANCED_FACE ( 'NONE', ( #56949 ), #46496, .F. ) ;
#95032 = ORIENTED_EDGE ( 'NONE', *, *, #60584, .F. ) ;
#95033 = ORIENTED_EDGE ( 'NONE', *, *, #116075, .T. ) ;
#95034 = DIRECTION ( 'NONE',  ( 0.000000000000000000, -0.9999939076577903929, 0.003490651415223739937 ) ) ;
#95035 = EDGE_LOOP ( 'NONE', ( #106520, #113639, #79306, #14307 ) ) ;
#95036 = CARTESIAN_POINT ( 'NONE',  ( -1.250000000000037970, 2.500000000000000000, 2.757883832488649656 ) ) ;
#95038 = EDGE_LOOP ( 'NONE', ( #71839, #92305 ) ) ;
#95037 = ORIENTED_EDGE ( 'NONE', *, *, #111123, .F. ) ;
#95039 = ORIENTED_EDGE ( 'NONE', *, *, #89075, .F. ) ;
#95040 = PLANE ( 'NONE',  #8098 ) ;
#95041 = AXIS2_PLACEMENT_3D ( 'NONE', #119055, #126944, #28093 ) ;
#95042 = AXIS2_PLACEMENT_3D ( 'NONE', #34653, #105301, #16246 ) ;
#95043 = DIRECTION ( 'NONE',  ( -0.000000000000000000, 1.000000000000000000, -0.000000000000000000 ) ) ;
#95044 = PRESENTATION_STYLE_ASSIGNMENT (( #13884 ) ) ;
#95045 = CARTESIAN_POINT ( 'NONE',  ( -3.550000000000030909, 12.50000000000000000, -6.841600689897078702 ) ) ;
#95046 = CARTESIAN_POINT ( 'NONE',  ( 115.5000000000000000, -5.000000000000000000, -4.999999999999997335 ) ) ;
#95047 = AXIS2_PLACEMENT_3D ( 'NONE', #35832, #75743, #26020 ) ;
#95048 = EDGE_CURVE ( 'NONE', #42483, #5536, #69734, .T. ) ;
#95049 = DIRECTION ( 'NONE',  ( -1.000000000000000000, -0.000000000000000000, -0.000000000000000000 ) ) ;
#95050 = ORIENTED_EDGE ( 'NONE', *, *, #75531, .T. ) ;
#95051 = EDGE_CURVE ( 'NONE', #50689, #8757, #46759, .T. ) ;
#95052 = DIRECTION ( 'NONE',  ( -4.274815082592931898E-19, -0.9999939076577903929, -0.003490651415223739937 ) ) ;
#95053 = VERTEX_POINT ( 'NONE', #25560 ) ;
#95054 = ORIENTED_EDGE ( 'NONE', *, *, #81891, .F. ) ;
#95055 = ORIENTED_EDGE ( 'NONE', *, *, #8599, .F. ) ;
#95056 = DIRECTION ( 'NONE',  ( -4.274815082592931898E-19, -0.9999939076577903929, -0.003490651415223739937 ) ) ;
#95057 = ORIENTED_EDGE ( 'NONE', *, *, #47438, .T. ) ;
#95058 = EDGE_CURVE ( 'NONE', #28288, #48604, #73939, .T. ) ;
#95059 = ORIENTED_EDGE ( 'NONE', *, *, #26493, .F. ) ;
#95060 = ORIENTED_EDGE ( 'NONE', *, *, #78079, .F. ) ;
#95061 = CIRCLE ( 'NONE', #126354, 0.1000000000000000472 ) ;
#95062 = CARTESIAN_POINT ( 'NONE',  ( 185.0312500006828031, 9.429780353434619030E-16, -7.700000000000000178 ) ) ;
#95063 = DIRECTION ( 'NONE',  ( 0.000000000000000000, 0.000000000000000000, -1.000000000000000000 ) ) ;
#95064 = DIRECTION ( 'NONE',  ( 0.000000000000000000, 0.000000000000000000, -1.000000000000000000 ) ) ;
#95065 = DIRECTION ( 'NONE',  ( 0.000000000000000000, 0.000000000000000000, 1.000000000000000000 ) ) ;
#95066 = DIRECTION ( 'NONE',  ( -4.274815082592931898E-19, -0.9999939076577903929, -0.003490651415223739937 ) ) ;
#95067 = DIRECTION ( 'NONE',  ( -0.000000000000000000, 1.000000000000000000, -0.000000000000000000 ) ) ;
#95068 = ORIENTED_EDGE ( 'NONE', *, *, #45921, .F. ) ;
#95069 = CARTESIAN_POINT ( 'NONE',  ( -0.8500000000000386136, 12.50000000000000000, 1.537336459617582918 ) ) ;
#95070 = AXIS2_PLACEMENT_3D ( 'NONE', #70376, #100477, #128686 ) ;
#95071 = EDGE_LOOP ( 'NONE', ( #83743, #122453 ) ) ;
#95072 = CARTESIAN_POINT ( 'NONE',  ( 10.84999999999990905, 12.50000000000000000, 2.165063509461097713 ) ) ;
#95073 = VERTEX_POINT ( 'NONE', #17679 ) ;
#95074 = CARTESIAN_POINT ( 'NONE',  ( 3.549999999999942979, 2.500000000000000000, 1.818653347947321475 ) ) ;
#95075 = ORIENTED_EDGE ( 'NONE', *, *, #4777, .T. ) ;
#95076 = ORIENTED_EDGE ( 'NONE', *, *, #88989, .F. ) ;
#95077 = CARTESIAN_POINT ( 'NONE',  ( -0.4000000000000331624, 2.500000000000000000, 0.1000000000000000056 ) ) ;
#95078 = CARTESIAN_POINT ( 'NONE',  ( -1.850000000000033840, 12.50000000000000000, 6.148780366869520897 ) ) ;
#95079 = EDGE_CURVE ( 'NONE', #96322, #2505, #24937, .T. ) ;
#95080 = DIRECTION ( 'NONE',  ( -0.000000000000000000, 1.000000000000000000, -0.000000000000000000 ) ) ;
#95081 = DIRECTION ( 'NONE',  ( 0.000000000000000000, -0.9999939076577903929, 0.003490651415223739937 ) ) ;
#95082 = ORIENTED_EDGE ( 'NONE', *, *, #2145, .F. ) ;
#95083 = CARTESIAN_POINT ( 'NONE',  ( -4.999999999999990230, 2.500000000000000000, -4.330127018922201643 ) ) ;
#95084 = DIRECTION ( 'NONE',  ( 0.000000000000000000, 0.000000000000000000, 1.000000000000000000 ) ) ;
#95085 = EDGE_CURVE ( 'NONE', #77033, #121438, #5066, .T. ) ;
#95086 = FACE_OUTER_BOUND ( 'NONE', #22728, .T. ) ;
#95087 = DIRECTION ( 'NONE',  ( 0.000000000000000000, 0.000000000000000000, 1.000000000000000000 ) ) ;
#95088 = EDGE_CURVE ( 'NONE', #62383, #43268, #106703, .T. ) ;
#95089 = DIRECTION ( 'NONE',  ( -0.000000000000000000, -1.000000000000000000, -0.000000000000000000 ) ) ;
#95090 = ORIENTED_EDGE ( 'NONE', *, *, #103648, .T. ) ;
#95091 = CIRCLE ( 'NONE', #28190, 0.06509327318403745899 ) ;
#95092 = AXIS2_PLACEMENT_3D ( 'NONE', #18035, #18687, #69728 ) ;
#95093 = ORIENTED_EDGE ( 'NONE', *, *, #106648, .T. ) ;
#95094 = EDGE_CURVE ( 'NONE', #91010, #384, #103286, .T. ) ;
#95095 = EDGE_CURVE ( 'NONE', #94262, #28931, #35409, .T. ) ;
#95096 = AXIS2_PLACEMENT_3D ( 'NONE', #103871, #89693, #119796 ) ;
#95097 = EDGE_CURVE ( 'NONE', #76936, #83004, #63572, .T. ) ;
#95098 = ORIENTED_EDGE ( 'NONE', *, *, #113680, .F. ) ;
#95099 = CIRCLE ( 'NONE', #38680, 0.1000000000000002554 ) ;
#95100 = CARTESIAN_POINT ( 'NONE',  ( 12.29999999999990479, 12.50000000000000000, -3.918623584224389056 ) ) ;
#95101 = FACE_OUTER_BOUND ( 'NONE', #106180, .T. ) ;
#95102 = EDGE_CURVE ( 'NONE', #110215, #997, #37347, .T. ) ;
#95103 = CARTESIAN_POINT ( 'NONE',  ( 184.0885416670080872, -6.551208109652273848, -3.782341765625003571 ) ) ;
#95104 = DIRECTION ( 'NONE',  ( -0.000000000000000000, -1.000000000000000000, -0.000000000000000000 ) ) ;
#95105 = DIRECTION ( 'NONE',  ( 0.000000000000000000, 1.000000000000000000, 0.000000000000000000 ) ) ;
#95106 = DIRECTION ( 'NONE',  ( -0.000000000000000000, -1.000000000000000000, -0.000000000000000000 ) ) ;
#95107 = CARTESIAN_POINT ( 'NONE',  ( 3.349999999999944578, 2.500000000000000000, -5.702370205355749455 ) ) ;
#95108 = ORIENTED_EDGE ( 'NONE', *, *, #48276, .F. ) ;
#95109 = EDGE_CURVE ( 'NONE', #23072, #87541, #107358, .T. ) ;
#95111 = DIRECTION ( 'NONE',  ( 0.000000000000000000, 1.000000000000000000, 0.000000000000000000 ) ) ;
#95110 = CIRCLE ( 'NONE', #26061, 0.09999999999999982514 ) ;
#95112 = DIRECTION ( 'NONE',  ( 0.000000000000000000, 1.000000000000000000, 0.000000000000000000 ) ) ;
#95113 = AXIS2_PLACEMENT_3D ( 'NONE', #40191, #38263, #108902 ) ;
#95114 = ORIENTED_EDGE ( 'NONE', *, *, #71633, .F. ) ;
#95115 = AXIS2_PLACEMENT_3D ( 'NONE', #116587, #26294, #105499 ) ;
#95116 = CARTESIAN_POINT ( 'NONE',  ( -0.8500000000000390576, 12.50000000000000000, -2.165063509461101710 ) ) ;
#95117 = CARTESIAN_POINT ( 'NONE',  ( 105.5000000000000142, 0.000000000000000000, 2.000000000000000000 ) ) ;
#95118 = CARTESIAN_POINT ( 'NONE',  ( 108.0000000000000142, 9.000000000000001776, 2.249999999999996891 ) ) ;
#95119 = CONICAL_SURFACE ( 'NONE', #99328, 0.09999999999999999167, 0.003490658503988666988 ) ;
#95120 = VECTOR ( 'NONE', #76509, 1000.000000000000000 ) ;
#95121 = EDGE_LOOP ( 'NONE', ( #99299, #96831, #20902, #36935 ) ) ;
#95122 = AXIS2_PLACEMENT_3D ( 'NONE', #87314, #39553, #89901 ) ;
#95123 = DIRECTION ( 'NONE',  ( -0.000000000000000000, 1.000000000000000000, -0.000000000000000000 ) ) ;
#95124 = ORIENTED_EDGE ( 'NONE', *, *, #112206, .F. ) ;
#95125 = CARTESIAN_POINT ( 'NONE',  ( 4.999999999999971578, 12.50000000000000000, -2.276824562219559311E-15 ) ) ;
#95126 = CARTESIAN_POINT ( 'NONE',  ( -0.8000000000000315747, 12.50000000000000000, 0.000000000000000000 ) ) ;
#95127 = DIRECTION ( 'NONE',  ( 0.000000000000000000, 0.000000000000000000, -1.000000000000000000 ) ) ;
#95128 = B_SPLINE_CURVE_WITH_KNOTS ( 'NONE', 3,
 ( #116542, #26883, #66790, #17015, #107374, #19650, #100143, #68735, #128326, #38662, #78582, #118475, #90963, #89031, #11091, #61520 ),
 .UNSPECIFIED., .F., .F.,
 ( 4, 2, 2, 2, 2, 2, 2, 4 ),
 ( 0.000000000000000000, 0.003502803217043994836, 0.007005606434087989672, 0.008757008042609990342, 0.01050840965113199015, 0.01225981125965399168, 0.01313551206391498985, 0.01401121286817599149 ),
 .UNSPECIFIED. ) ;
#95129 = ORIENTED_EDGE ( 'NONE', *, *, #42855, .T. ) ;
#95130 = CIRCLE ( 'NONE', #86713, 0.1000000000000000472 ) ;
#95131 = AXIS2_PLACEMENT_3D ( 'NONE', #117343, #36259, #127216 ) ;
#95132 = LINE ( 'NONE', #123927, #86485 ) ;
#95133 = DIRECTION ( 'NONE',  ( -0.000000000000000000, 1.000000000000000000, -0.000000000000000000 ) ) ;
#95134 = CIRCLE ( 'NONE', #97275, 0.06509327318403745899 ) ;
#95135 = ORIENTED_EDGE ( 'NONE', *, *, #62860, .T. ) ;
#95136 = CARTESIAN_POINT ( 'NONE',  ( -4.350000000000023626, 2.500000000000000000, 6.248780366869521430 ) ) ;
#95138 = ORIENTED_EDGE ( 'NONE', *, *, #22406, .T. ) ;
#95137 = EDGE_CURVE ( 'NONE', #118811, #60113, #5911, .T. ) ;
#95139 = EDGE_LOOP ( 'NONE', ( #77664, #109799 ) ) ;
#95140 = CARTESIAN_POINT ( 'NONE',  ( 7.299999999999924327, 2.500000000000000000, 0.3464101615137735735 ) ) ;
#95141 = DIRECTION ( 'NONE',  ( -0.000000000000000000, 1.000000000000000000, -0.000000000000000000 ) ) ;
#95142 = ORIENTED_EDGE ( 'NONE', *, *, #99345, .F. ) ;
#95143 = CARTESIAN_POINT ( 'NONE',  ( 9.549999999999915445, 12.50000000000000000, 6.495190528383297135 ) ) ;
#95144 = LINE ( 'NONE', #16556, #8741 ) ;
#95145 = CIRCLE ( 'NONE', #107666, 0.06509327318403745899 ) ;
#95146 = VERTEX_POINT ( 'NONE', #36051 ) ;
#95147 = EDGE_CURVE ( 'NONE', #28723, #107807, #55257, .T. ) ;
#95148 = DIRECTION ( 'NONE',  ( 0.000000000000000000, 1.000000000000000000, 0.000000000000000000 ) ) ;
#95149 = DIRECTION ( 'NONE',  ( 0.000000000000000000, -0.000000000000000000, 1.000000000000000000 ) ) ;
#95150 = DIRECTION ( 'NONE',  ( 0.000000000000000000, 0.000000000000000000, 1.000000000000000000 ) ) ;
#95151 = DIRECTION ( 'NONE',  ( 0.000000000000000000, 0.000000000000000000, 1.000000000000000000 ) ) ;
#95152 = DIRECTION ( 'NONE',  ( 0.000000000000000000, 1.000000000000000000, 0.000000000000000000 ) ) ;
#95153 = CONICAL_SURFACE ( 'NONE', #5349, 0.1000000000000002554, 0.003490658503988666988 ) ;
#95154 = CARTESIAN_POINT ( 'NONE',  ( -11.05000000000000071, 2.500000000000000000, 6.741600689897071952 ) ) ;
#95155 = AXIS2_PLACEMENT_3D ( 'NONE', #61859, #2261, #5482 ) ;
#95156 = AXIS2_PLACEMENT_3D ( 'NONE', #10302, #20767, #59429 ) ;
#95157 = EDGE_LOOP ( 'NONE', ( #27163, #8677 ) ) ;
#95158 = ORIENTED_EDGE ( 'NONE', *, *, #45561, .T. ) ;
#95159 = EDGE_LOOP ( 'NONE', ( #53757, #3418 ) ) ;
#95160 = ORIENTED_EDGE ( 'NONE', *, *, #31523, .T. ) ;
#95161 = CARTESIAN_POINT ( 'NONE',  ( 59.86274543073836440, 3.775833904478943737, 4.995381933851997580 ) ) ;
#95162 = CYLINDRICAL_SURFACE ( 'NONE', #42949, 2.000000000000000000 ) ;
#95163 = DIRECTION ( 'NONE',  ( 0.000000000000000000, -0.9999939076577903929, 0.003490651415223739937 ) ) ;
#95164 = ORIENTED_EDGE ( 'NONE', *, *, #87762, .F. ) ;
#95165 = FACE_BOUND ( 'NONE', #58899, .T. ) ;
#95166 = CARTESIAN_POINT ( 'NONE',  ( -1.850000000000033840, 2.500000000000000000, 2.611473670974873151 ) ) ;
#95167 = LINE ( 'NONE', #8062, #87744 ) ;
#95168 = CIRCLE ( 'NONE', #38762, 0.06509327318403745899 ) ;
#95169 = DIRECTION ( 'NONE',  ( 0.000000000000000000, -0.000000000000000000, 1.000000000000000000 ) ) ;
#95170 = FACE_OUTER_BOUND ( 'NONE', #111127, .T. ) ;
#95171 = CONICAL_SURFACE ( 'NONE', #74242, 0.1000000000000000472, 0.003490658503988666988 ) ;
#95172 = CARTESIAN_POINT ( 'NONE',  ( -1.650000000000034772, 12.50000000000000000, 5.737276932171707422 ) ) ;
#95173 = CARTESIAN_POINT ( 'NONE',  ( -11.64999999999999680, 2.500000000000000000, 2.165063509461097713 ) ) ;
#95174 = DIRECTION ( 'NONE',  ( -0.000000000000000000, 1.000000000000000000, -0.000000000000000000 ) ) ;
#95175 = DIRECTION ( 'NONE',  ( 0.000000000000000000, 0.000000000000000000, 1.000000000000000000 ) ) ;
#95176 = CARTESIAN_POINT ( 'NONE',  ( 4.999999999999971578, 12.50000000000000000, -0.06509327318403970719 ) ) ;
#95177 = DIRECTION ( 'NONE',  ( 0.000000000000000000, 1.000000000000000000, 0.000000000000000000 ) ) ;
#95178 = EDGE_CURVE ( 'NONE', #25799, #52300, #82368, .T. ) ;
#95179 = CIRCLE ( 'NONE', #40826, 0.06509327318403745899 ) ;
#95180 = ORIENTED_EDGE ( 'NONE', *, *, #9685, .T. ) ;
#95181 = ORIENTED_EDGE ( 'NONE', *, *, #1700, .F. ) ;
#95182 = CIRCLE ( 'NONE', #51376, 0.1000000000000002554 ) ;
#95183 = VERTEX_POINT ( 'NONE', #8497 ) ;
#95184 = ORIENTED_EDGE ( 'NONE', *, *, #29390, .F. ) ;
#95185 = DIRECTION ( 'NONE',  ( 0.000000000000000000, 1.000000000000000000, 0.000000000000000000 ) ) ;
#95186 = EDGE_LOOP ( 'NONE', ( #128009, #15254, #115081, #28510 ) ) ;
#95187 = CARTESIAN_POINT ( 'NONE',  ( 3.349999999999945466, 2.500000000000000000, -2.165063509461101710 ) ) ;
#95188 = ORIENTED_EDGE ( 'NONE', *, *, #11830, .T. ) ;
#95189 = VERTEX_POINT ( 'NONE', #80499 ) ;
#95190 = LINE ( 'NONE', #46735, #62611 ) ;
#95191 = EDGE_CURVE ( 'NONE', #20105, #81996, #42660, .T. ) ;
#95192 = CONICAL_SURFACE ( 'NONE', #38782, 0.1000000000000002554, 0.003490658503988666988 ) ;
#95193 = CARTESIAN_POINT ( 'NONE',  ( 10.06913504587715202, -2.500000000000000444, 8.158951466338434599 ) ) ;
#95194 = DIRECTION ( 'NONE',  ( 0.000000000000000000, 1.000000000000000000, 0.000000000000000000 ) ) ;
#95195 = CARTESIAN_POINT ( 'NONE',  ( 5.199999999999935341, 12.50000000000000000, -3.983716857408426293 ) ) ;
#95196 = DIRECTION ( 'NONE',  ( -0.000000000000000000, 1.000000000000000000, -0.000000000000000000 ) ) ;
#95197 = EDGE_CURVE ( 'NONE', #114600, #108081, #108645, .T. ) ;
#95198 = EDGE_CURVE ( 'NONE', #104829, #83303, #124207, .T. ) ;
#95199 = CONICAL_SURFACE ( 'NONE', #65845, 0.09999999999999982514, 0.003490658503988666988 ) ;
#95200 = ORIENTED_EDGE ( 'NONE', *, *, #97501, .T. ) ;
#95201 = ORIENTED_EDGE ( 'NONE', *, *, #29012, .F. ) ;
#95203 = ORIENTED_EDGE ( 'NONE', *, *, #122718, .F. ) ;
#95202 = CIRCLE ( 'NONE', #78497, 0.06509327318403745899 ) ;
#95205 = ORIENTED_EDGE ( 'NONE', *, *, #8764, .F. ) ;
#95204 = DIRECTION ( 'NONE',  ( 0.000000000000000000, 1.000000000000000000, 0.000000000000000000 ) ) ;
#95206 = EDGE_CURVE ( 'NONE', #11701, #50102, #107486, .T. ) ;
#95207 = AXIS2_PLACEMENT_3D ( 'NONE', #44862, #105041, #95246 ) ;
#95208 = CARTESIAN_POINT ( 'NONE',  ( 7.499999999999927169, 2.500000000000000000, -4.922947341949753586 ) ) ;
#95209 = ORIENTED_EDGE ( 'NONE', *, *, #59469, .F. ) ;
#95210 = EDGE_CURVE ( 'NONE', #24001, #121148, #80301, .T. ) ;
#95211 = ORIENTED_EDGE ( 'NONE', *, *, #54864, .F. ) ;
#95212 = DIRECTION ( 'NONE',  ( -0.000000000000000000, 1.000000000000000000, -0.000000000000000000 ) ) ;
#95213 = AXIS2_PLACEMENT_3D ( 'NONE', #8583, #47261, #19049 ) ;
#95214 = AXIS2_PLACEMENT_3D ( 'NONE', #31922, #120301, #111092 ) ;
#95215 = AXIS2_PLACEMENT_3D ( 'NONE', #125170, #74140, #24391 ) ;
#95216 = DIRECTION ( 'NONE',  ( 0.000000000000000000, 1.000000000000000000, 0.000000000000000000 ) ) ;
#95217 = FACE_OUTER_BOUND ( 'NONE', #18592, .T. ) ;
#95218 = FACE_OUTER_BOUND ( 'NONE', #23004, .T. ) ;
#95219 = CONICAL_SURFACE ( 'NONE', #78513, 0.1000000000000002554, 0.003490658503988666988 ) ;
#95220 = DIRECTION ( 'NONE',  ( 0.000000000000000000, 1.000000000000000000, 0.000000000000000000 ) ) ;
#95221 = ORIENTED_EDGE ( 'NONE', *, *, #52949, .F. ) ;
#95222 = CARTESIAN_POINT ( 'NONE',  ( 7.899999999999924860, 2.500000000000000000, -4.330127018922201643 ) ) ;
#95223 = CIRCLE ( 'NONE', #9449, 7.541925104783893552 ) ;
#95224 = AXIS2_PLACEMENT_3D ( 'NONE', #67622, #107568, #17885 ) ;
#95225 = VERTEX_POINT ( 'NONE', #119118 ) ;
#95226 = CARTESIAN_POINT ( 'NONE',  ( 14.59999999999989484, 12.50000000000000000, -2.276824562219559311E-15 ) ) ;
#95227 = CONICAL_SURFACE ( 'NONE', #38819, 0.09999999999999982514, 0.003490658503988666988 ) ;
#95228 = ORIENTED_EDGE ( 'NONE', *, *, #112519, .T. ) ;
#95229 = CARTESIAN_POINT ( 'NONE',  ( 12.49999999999990230, 2.500000000000000000, -0.7928203230275542301 ) ) ;
#95230 = CARTESIAN_POINT ( 'NONE',  ( -8.749999999999976907, 2.500000000000000000, -6.495190528383297135 ) ) ;
#95231 = AXIS2_PLACEMENT_3D ( 'NONE', #28930, #77375, #58393 ) ;
#95232 = ORIENTED_EDGE ( 'NONE', *, *, #68585, .T. ) ;
#95233 = LINE ( 'NONE', #4888, #29979 ) ;
#95234 = FACE_OUTER_BOUND ( 'NONE', #101577, .T. ) ;
#95235 = ORIENTED_EDGE ( 'NONE', *, *, #38255, .T. ) ;
#95236 = DIRECTION ( 'NONE',  ( 0.000000000000000000, 0.000000000000000000, 1.000000000000000000 ) ) ;
#95237 = ADVANCED_FACE ( 'NONE', ( #69356 ), #109291, .T. ) ;
#95238 = DIRECTION ( 'NONE',  ( -0.000000000000000000, 1.000000000000000000, -0.000000000000000000 ) ) ;
#95239 = ORIENTED_EDGE ( 'NONE', *, *, #66404, .F. ) ;
#95240 = ORIENTED_EDGE ( 'NONE', *, *, #38524, .F. ) ;
#95241 = VERTEX_POINT ( 'NONE', #78569 ) ;
#95242 = FACE_OUTER_BOUND ( 'NONE', #122625, .T. ) ;
#95243 = CARTESIAN_POINT ( 'NONE',  ( -9.150000000000009237, 12.50000000000000000, 1.472243186433545459 ) ) ;
#95244 = CARTESIAN_POINT ( 'NONE',  ( 184.9843750003414016, -8.734944146203032389, -1.604583208406768146E-15 ) ) ;
#95245 = AXIS2_PLACEMENT_3D ( 'NONE', #59617, #119150, #20312 ) ;
#95246 = DIRECTION ( 'NONE',  ( 0.000000000000000000, 0.000000000000000000, -1.000000000000000000 ) ) ;
#95247 = ADVANCED_FACE ( 'NONE', ( #108000 ), #57310, .T. ) ;
#95248 = CARTESIAN_POINT ( 'NONE',  ( 11.69999999999990514, 2.500000000000000000, -0.1000000000000022815 ) ) ;
#95249 = DIRECTION ( 'NONE',  ( -0.000000000000000000, 1.000000000000000000, -0.000000000000000000 ) ) ;
#95250 = EDGE_CURVE ( 'NONE', #39170, #82540, #117805, .T. ) ;
#95251 = AXIS2_PLACEMENT_3D ( 'NONE', #13209, #1462, #102260 ) ;
#95252 = EDGE_CURVE ( 'NONE', #48345, #49639, #67766, .T. ) ;
#95253 = CIRCLE ( 'NONE', #105716, 0.06509327318403745899 ) ;
#95254 = ADVANCED_FACE ( 'NONE', ( #19634 ), #92826, .T. ) ;
#95255 = ORIENTED_EDGE ( 'NONE', *, *, #87927, .T. ) ;
#95256 = CIRCLE ( 'NONE', #74321, 0.1000000000000002554 ) ;
#95257 = CARTESIAN_POINT ( 'NONE',  ( 10.39999999999991509, 2.500000000000000000, 0.7928203230275495672 ) ) ;
#95258 = EDGE_LOOP ( 'NONE', ( #49512, #113367 ) ) ;
#95259 = ADVANCED_FACE ( 'NONE', ( #90275 ), #88343, .T. ) ;
#95260 = CARTESIAN_POINT ( 'NONE',  ( -0.6500000000000398792, 2.500000000000000000, -6.841600689897078702 ) ) ;
#95261 = DIRECTION ( 'NONE',  ( -0.000000000000000000, 1.000000000000000000, -0.000000000000000000 ) ) ;
#95262 = DIRECTION ( 'NONE',  ( 0.000000000000000000, 1.000000000000000000, 0.000000000000000000 ) ) ;
#95263 = ORIENTED_EDGE ( 'NONE', *, *, #106012, .T. ) ;
#95264 = EDGE_CURVE ( 'NONE', #32613, #108881, #50374, .T. ) ;
#95265 = AXIS2_PLACEMENT_3D ( 'NONE', #112525, #113151, #42500 ) ;
#95266 = ADVANCED_FACE ( 'NONE', ( #118461 ), #53107, .T. ) ;
#95267 = VECTOR ( 'NONE', #72476, 1000.000000000000000 ) ;
#95268 = LINE ( 'NONE', #65130, #20006 ) ;
#95269 = CARTESIAN_POINT ( 'NONE',  ( -12.29999999999999538, 2.500000000000000000, 4.576537180435972019 ) ) ;
#95270 = ORIENTED_EDGE ( 'NONE', *, *, #4794, .T. ) ;
#95271 = FACE_OUTER_BOUND ( 'NONE', #100505, .T. ) ;
#95272 = CIRCLE ( 'NONE', #45105, 0.1000000000000002554 ) ;
#95273 = AXIS2_PLACEMENT_3D ( 'NONE', #83893, #84548, #75360 ) ;
#95274 = ORIENTED_EDGE ( 'NONE', *, *, #96237, .T. ) ;
#95275 = ORIENTED_EDGE ( 'NONE', *, *, #71733, .T. ) ;
#95276 = CARTESIAN_POINT ( 'NONE',  ( -9.800000000000004263, 2.500000000000000000, 3.883716857408420431 ) ) ;
#95277 = ORIENTED_EDGE ( 'NONE', *, *, #65352, .F. ) ;
#95278 = DIRECTION ( 'NONE',  ( 0.000000000000000000, -0.9999939076577903929, 0.003490651415223739937 ) ) ;
#95279 = CARTESIAN_POINT ( 'NONE',  ( -8.100000000000013856, 12.50000000000000000, 0.3464101615137736845 ) ) ;
#95280 = CARTESIAN_POINT ( 'NONE',  ( -0.8500000000000382805, 2.500000000000000000, -5.702370205355749455 ) ) ;
#95281 = ORIENTED_EDGE ( 'NONE', *, *, #21941, .F. ) ;
#95282 = FACE_BOUND ( 'NONE', #22497, .T. ) ;
#95284 = ORIENTED_EDGE ( 'NONE', *, *, #59684, .F. ) ;
#95283 = CARTESIAN_POINT ( 'NONE',  ( -6.249999999999981348, 12.50000000000000000, 2.165063509461097713 ) ) ;
#95285 = PLANE ( 'NONE',  #15161 ) ;
#95286 = DIRECTION ( 'NONE',  ( 0.000000000000000000, 0.000000000000000000, -1.000000000000000000 ) ) ;
#95287 = VERTEX_POINT ( 'NONE', #89660 ) ;
#95288 = AXIS2_PLACEMENT_3D ( 'NONE', #36261, #16585, #27704 ) ;
#95289 = ORIENTED_EDGE ( 'NONE', *, *, #71253, .T. ) ;
#95290 = VECTOR ( 'NONE', #112799, 1000.000000000000000 ) ;
#95291 = ORIENTED_EDGE ( 'NONE', *, *, #71560, .T. ) ;
#95292 = FACE_OUTER_BOUND ( 'NONE', #45448, .T. ) ;
#95293 = LINE ( 'NONE', #84816, #97986 ) ;
#95294 =( BOUNDED_CURVE ( )  B_SPLINE_CURVE ( 2, ( #89744, #109381, #50457, #110038, #119847, #712, #60310 ),
 .UNSPECIFIED., .F., .F. ) 
 B_SPLINE_CURVE_WITH_KNOTS ( ( 3, 2, 2, 3 ),
 ( 0.07142857142857149400, 0.09523809523809532995, 0.1190476190476191520, 0.1428571428571429880 ),
 .UNSPECIFIED. ) 
 CURVE ( )  GEOMETRIC_REPRESENTATION_ITEM ( )  RATIONAL_B_SPLINE_CURVE ( ( 0.9999999999999996669, 0.8660254037844390407, 1.000000000000000000, 0.8660254037844387076, 1.000000000000000000, 0.8660254037844379305, 1.000000000000000666 ) ) 
 REPRESENTATION_ITEM ( '' )  );
#95295 = DIRECTION ( 'NONE',  ( 0.000000000000000000, 0.000000000000000000, -1.000000000000000000 ) ) ;
#95296 = FACE_BOUND ( 'NONE', #50494, .T. ) ;
#95297 = ORIENTED_EDGE ( 'NONE', *, *, #115005, .F. ) ;
#95298 = CARTESIAN_POINT ( 'NONE',  ( 185.1510416670080872, 4.367472073101518859, -7.564683531249999149 ) ) ;
#95299 = CARTESIAN_POINT ( 'NONE',  ( 129.5000000000000000, -0.6250000000000000000, 7.634788798650553154 ) ) ;
#95300 = LINE ( 'NONE', #5602, #23013 ) ;
#95301 = EDGE_CURVE ( 'NONE', #73914, #67694, #111687, .T. ) ;
#95302 = CARTESIAN_POINT ( 'NONE',  ( -1.700000000000034817, 2.500000000000000000, -2.385244779468109755E-15 ) ) ;
#95303 = CARTESIAN_POINT ( 'NONE',  ( 10.44999999999991402, 2.500000000000000000, 6.495190528383297135 ) ) ;
#95304 = CIRCLE ( 'NONE', #128778, 0.09999999999999999167 ) ;
#95305 = CARTESIAN_POINT ( 'NONE',  ( 2.949999999999946887, 2.500000000000000000, -6.395190528383301931 ) ) ;
#95306 = CARTESIAN_POINT ( 'NONE',  ( -13.14999999999999147, 12.50000000000000000, -1.818653347947323917 ) ) ;
#95307 = CARTESIAN_POINT ( 'NONE',  ( -6.050000000000020250, 2.500000000000000000, -2.511473670974877948 ) ) ;
#95308 = AXIS2_PLACEMENT_3D ( 'NONE', #36098, #16416, #56364 ) ;
#95309 = FACE_OUTER_BOUND ( 'NONE', #120014, .T. ) ;
#95310 = CONICAL_SURFACE ( 'NONE', #61878, 0.1000000000000000472, 0.003490658503988666988 ) ;
#95311 = VERTEX_POINT ( 'NONE', #6329 ) ;
#95312 = ORIENTED_EDGE ( 'NONE', *, *, #92290, .F. ) ;
#95313 = VERTEX_POINT ( 'NONE', #96653 ) ;
#95314 = VERTEX_POINT ( 'NONE', #87483 ) ;
#95315 = AXIS2_PLACEMENT_3D ( 'NONE', #25364, #93488, #5724 ) ;
#95316 = ORIENTED_EDGE ( 'NONE', *, *, #35673, .F. ) ;
#95317 = FACE_OUTER_BOUND ( 'NONE', #97642, .T. ) ;
#95318 = DIRECTION ( 'NONE',  ( 0.000000000000000000, 0.000000000000000000, -1.000000000000000000 ) ) ;
#95319 = ORIENTED_EDGE ( 'NONE', *, *, #6711, .T. ) ;
#95320 = FACE_BOUND ( 'NONE', #1146, .T. ) ;
#95321 = CARTESIAN_POINT ( 'NONE',  ( 4.799999999999935874, 12.50000000000000000, 3.983716857408420964 ) ) ;
#95322 = DIRECTION ( 'NONE',  ( -1.000000000000000000, 0.000000000000000000, 0.000000000000000000 ) ) ;
#95323 = VERTEX_POINT ( 'NONE', #95390 ) ;
#95324 = DIRECTION ( 'NONE',  ( -0.000000000000000000, 1.000000000000000000, -0.000000000000000000 ) ) ;
#95325 = CARTESIAN_POINT ( 'NONE',  ( 186.7500000000000000, 9.429780353434619030E-16, -7.700000000000000178 ) ) ;
#95326 = CARTESIAN_POINT ( 'NONE',  ( -1.900000000000034994, 2.500000000000000000, -4.676537180435978769 ) ) ;
#95328 = VERTEX_POINT ( 'NONE', #77668 ) ;
#95327 = AXIS2_PLACEMENT_3D ( 'NONE', #93563, #3251, #91623 ) ;
#95329 = CARTESIAN_POINT ( 'NONE',  ( 5.799999999999933209, 2.500000000000000000, -2.385244779468109755E-15 ) ) ;
#95330 = ORIENTED_EDGE ( 'NONE', *, *, #25456, .T. ) ;
#95331 = PRODUCT ( 'Internal PCBA Controller Module', 'Internal PCBA Controller Module', '', ( #56864 ) ) ;
#95332 = ORIENTED_EDGE ( 'NONE', *, *, #15962, .F. ) ;
#95333 = VERTEX_POINT ( 'NONE', #106497 ) ;
#95334 = CARTESIAN_POINT ( 'NONE',  ( -1.850000000000033396, 2.500000000000000000, -2.611473670974877592 ) ) ;
#95335 = CARTESIAN_POINT ( 'NONE',  ( -6.249999999999984901, 2.500000000000000000, -6.495190528383302464 ) ) ;
#95336 = CIRCLE ( 'NONE', #5524, 0.1000000000000002554 ) ;
#95337 = DIRECTION ( 'NONE',  ( -0.000000000000000000, -1.000000000000000000, -0.000000000000000000 ) ) ;
#95338 = EDGE_LOOP ( 'NONE', ( #73328, #59603, #68746, #108077, #6275, #79544, #68593, #112317, #5616, #23181, #97196, #17633, #27369, #17954, #34971, #66961, #15467 ) ) ;
#95339 = CARTESIAN_POINT ( 'NONE',  ( 11.74779829703379974, 2.500000000000000000, -7.682567037525008580 ) ) ;
#95340 = CIRCLE ( 'NONE', #38935, 0.1000000000000002554 ) ;
#95341 = VECTOR ( 'NONE', #118002, 1000.000000000000000 ) ;
#95342 = EDGE_CURVE ( 'NONE', #14399, #115596, #109545, .T. ) ;
#95343 = CARTESIAN_POINT ( 'NONE',  ( 12.09999999999990550, 2.500000000000000000, -3.637306695894650055 ) ) ;
#95344 = AXIS2_PLACEMENT_3D ( 'NONE', #44433, #73252, #122366 ) ;
#95345 = DIRECTION ( 'NONE',  ( 0.000000000000000000, 0.000000000000000000, 1.000000000000000000 ) ) ;
#95346 = CARTESIAN_POINT ( 'NONE',  ( 187.3177083336747444, 4.367472073101515306, 7.564683531250000925 ) ) ;
#95347 = PLANE ( 'NONE',  #71820 ) ;
#95348 = EDGE_CURVE ( 'NONE', #80050, #20142, #71984, .T. ) ;
#95349 = CARTESIAN_POINT ( 'NONE',  ( 179.5000000000000000, -0.6250000000000028866, -7.634788798650553154 ) ) ;
#95350 = ADVANCED_FACE ( 'NONE', ( #65265 ), #56096, .T. ) ;
#95351 = EDGE_LOOP ( 'NONE', ( #15612, #104300 ) ) ;
#95352 = FACE_OUTER_BOUND ( 'NONE', #5850, .T. ) ;
#95353 = CIRCLE ( 'NONE', #128832, 0.06509327318403745899 ) ;
#95354 = ORIENTED_EDGE ( 'NONE', *, *, #12933, .F. ) ;
#95356 = AXIS2_PLACEMENT_3D ( 'NONE', #114949, #25274, #73736 ) ;
#95355 = AXIS2_PLACEMENT_3D ( 'NONE', #79894, #78630, #71348 ) ;
#95357 = ORIENTED_EDGE ( 'NONE', *, *, #60518, .T. ) ;
#95358 = CARTESIAN_POINT ( 'NONE',  ( 12.89999999999990266, 2.500000000000000000, -3.637306695894650055 ) ) ;
#95359 = CARTESIAN_POINT ( 'NONE',  ( 11.89999999999990798, 2.500000000000000000, 3.983716857408420964 ) ) ;
#95360 = EDGE_CURVE ( 'NONE', #39771, #86684, #107785, .T. ) ;
#95361 = EDGE_CURVE ( 'NONE', #101786, #91215, #65918, .T. ) ;
#95362 = LINE ( 'NONE', #43704, #109479 ) ;
#95363 = CARTESIAN_POINT ( 'NONE',  ( -7.300000000000016698, 2.500000000000000000, -0.4464101615137783252 ) ) ;
#95364 = ADVANCED_FACE ( 'NONE', ( #46950 ), #117572, .T. ) ;
#95365 = ORIENTED_EDGE ( 'NONE', *, *, #99912, .F. ) ;
#95366 = ORIENTED_EDGE ( 'NONE', *, *, #89892, .F. ) ;
#95367 = CARTESIAN_POINT ( 'NONE',  ( 2.699999999999946443, 2.500000000000000000, -4.083716857408426826 ) ) ;
#95368 = CARTESIAN_POINT ( 'NONE',  ( 11.84999999999990372, 2.500000000000000000, -6.841600689897078702 ) ) ;
#95369 = CARTESIAN_POINT ( 'NONE',  ( -12.09999999999999609, 2.500000000000000000, -5.022947341949751454 ) ) ;
#95370 = ORIENTED_EDGE ( 'NONE', *, *, #91088, .T. ) ;
#95371 = ORIENTED_EDGE ( 'NONE', *, *, #87778, .F. ) ;
#95372 = CARTESIAN_POINT ( 'NONE',  ( 11.84999999999990372, 12.50000000000000000, 1.818653347947321475 ) ) ;
#95373 = ORIENTED_EDGE ( 'NONE', *, *, #87828, .T. ) ;
#95374 = DIRECTION ( 'NONE',  ( 0.000000000000000000, 0.000000000000000000, 1.000000000000000000 ) ) ;
#95375 = CARTESIAN_POINT ( 'NONE',  ( 5.799999999999934985, 2.500000000000000000, -4.230127018922201998 ) ) ;
#95376 = ORIENTED_EDGE ( 'NONE', *, *, #88546, .F. ) ;
#95377 = CARTESIAN_POINT ( 'NONE',  ( -4.999999999999986677, 2.500000000000000000, -2.276824562219559311E-15 ) ) ;
#95378 = CARTESIAN_POINT ( 'NONE',  ( -1.250000000000037970, 12.50000000000000000, 7.253104124594885960 ) ) ;
#95379 = CARTESIAN_POINT ( 'NONE',  ( -11.44999999999999929, 2.500000000000000000, -6.148780366869522673 ) ) ;
#95380 = CARTESIAN_POINT ( 'NONE',  ( -0.2000000000000412836, 12.50000000000000000, 4.676537180435972552 ) ) ;
#95381 = ORIENTED_EDGE ( 'NONE', *, *, #12301, .F. ) ;
#95382 = DIRECTION ( 'NONE',  ( -0.000000000000000000, -1.000000000000000000, -0.000000000000000000 ) ) ;
#95383 = AXIS2_PLACEMENT_3D ( 'NONE', #10019, #42730, #121903 ) ;
#95384 = CIRCLE ( 'NONE', #112196, 0.1000000000000002554 ) ;
#95385 = FACE_OUTER_BOUND ( 'NONE', #112197, .T. ) ;
#95386 = ORIENTED_EDGE ( 'NONE', *, *, #27353, .F. ) ;
#95387 = ORIENTED_EDGE ( 'NONE', *, *, #91409, .F. ) ;
#95388 = CARTESIAN_POINT ( 'NONE',  ( 184.7552083336747444, 6.551208109652275624, -3.782341765624998686 ) ) ;
#95389 = DIRECTION ( 'NONE',  ( -0.000000000000000000, 1.000000000000000000, -0.000000000000000000 ) ) ;
#95390 = CARTESIAN_POINT ( 'NONE',  ( 10.39999999999991154, 2.500000000000000000, -3.537306695894649966 ) ) ;
#95391 = FACE_OUTER_BOUND ( 'NONE', #110548, .T. ) ;
#95392 = CARTESIAN_POINT ( 'NONE',  ( -0.6500000000000403233, 2.500000000000000000, 1.718653347947321386 ) ) ;
#95394 = DIRECTION ( 'NONE',  ( 0.000000000000000000, -0.000000000000000000, 1.000000000000000000 ) ) ;
#95393 = CONICAL_SURFACE ( 'NONE', #126791, 0.1000000000000002554, 0.003490658503988666988 ) ;
#95395 = DIRECTION ( 'NONE',  ( -0.000000000000000000, 1.000000000000000000, -0.000000000000000000 ) ) ;
#95396 = DIRECTION ( 'NONE',  ( 0.000000000000000000, 0.000000000000000000, -1.000000000000000000 ) ) ;
#95397 = CARTESIAN_POINT ( 'NONE',  ( 5.849999999999933920, 2.500000000000000000, -2.757883832488654097 ) ) ;
#95398 = DIRECTION ( 'NONE',  ( 0.000000000000000000, -0.9999939076577903929, 0.003490651415223739937 ) ) ;
#95399 = EDGE_CURVE ( 'NONE', #18200, #68464, #126788, .T. ) ;
#95400 = EDGE_CURVE ( 'NONE', #111304, #45268, #34344, .T. ) ;
#95401 = EDGE_CURVE ( 'NONE', #7829, #117308, #23870, .T. ) ;
#95402 = DIRECTION ( 'NONE',  ( 0.000000000000000000, 1.000000000000000000, 0.000000000000000000 ) ) ;
#95404 = AXIS2_PLACEMENT_3D ( 'NONE', #24301, #23653, #3999 ) ;
#95403 = VECTOR ( 'NONE', #25051, 1000.000000000000000 ) ;
#95405 = ORIENTED_EDGE ( 'NONE', *, *, #16605, .F. ) ;
#95406 = EDGE_LOOP ( 'NONE', ( #22920, #22904, #21709, #39838 ) ) ;
#95407 = EDGE_CURVE ( 'NONE', #64709, #62921, #49007, .T. ) ;
#95408 = ORIENTED_EDGE ( 'NONE', *, *, #19990, .T. ) ;
#95409 = EDGE_CURVE ( 'NONE', #96334, #4778, #75735, .T. ) ;
#95410 = DIRECTION ( 'NONE',  ( -0.000000000000000000, 1.000000000000000000, -0.000000000000000000 ) ) ;
#95411 = FACE_OUTER_BOUND ( 'NONE', #17659, .T. ) ;
#95412 = EDGE_CURVE ( 'NONE', #115890, #62546, #120007, .T. ) ;
#95413 = ORIENTED_EDGE ( 'NONE', *, *, #47287, .F. ) ;
#95414 = EDGE_CURVE ( 'NONE', #83814, #73789, #65708, .T. ) ;
#95415 = CARTESIAN_POINT ( 'NONE',  ( -14.99999999999994671, 2.500000000000000000, 0.000000000000000000 ) ) ;
#95416 = EDGE_CURVE ( 'NONE', #19273, #8444, #128076, .T. ) ;
#95417 = DIRECTION ( 'NONE',  ( -0.000000000000000000, 1.000000000000000000, -0.000000000000000000 ) ) ;
#95419 = ORIENTED_EDGE ( 'NONE', *, *, #49906, .F. ) ;
#95418 = FACE_OUTER_BOUND ( 'NONE', #85239, .T. ) ;
#95420 = AXIS2_PLACEMENT_3D ( 'NONE', #28697, #58797, #9033 ) ;
#95421 = ADVANCED_FACE ( 'NONE', ( #38423 ), #7637, .T. ) ;
#95422 = CARTESIAN_POINT ( 'NONE',  ( 9.149999999999920419, 2.500000000000000000, -7.288010851410854585 ) ) ;
#95423 = VERTEX_POINT ( 'NONE', #116299 ) ;
#95424 = AXIS2_PLACEMENT_3D ( 'NONE', #80155, #8175, #88006 ) ;
#95425 = AXIS2_PLACEMENT_3D ( 'NONE', #57888, #78170, #8119 ) ;
#95426 = ORIENTED_EDGE ( 'NONE', *, *, #61960, .F. ) ;
#95427 = VERTEX_POINT ( 'NONE', #26653 ) ;
#95428 = VERTEX_POINT ( 'NONE', #66558 ) ;
#95429 = CARTESIAN_POINT ( 'NONE',  ( -8.100000000000013856, 2.500000000000000000, -0.4464101615137782142 ) ) ;
#95430 = AXIS2_PLACEMENT_3D ( 'NONE', #94854, #112570, #55575 ) ;
#95431 = CIRCLE ( 'NONE', #107950, 0.06509327318403745899 ) ;
#95432 = DIRECTION ( 'NONE',  ( 0.000000000000000000, 0.000000000000000000, 1.000000000000000000 ) ) ;
#95433 = CARTESIAN_POINT ( 'NONE',  ( 11.24999999999991118, 12.50000000000000000, -2.857883832488653741 ) ) ;
#95434 = VECTOR ( 'NONE', #97720, 1000.000000000000000 ) ;
#95435 = DIRECTION ( 'NONE',  ( 0.000000000000000000, 0.000000000000000000, 1.000000000000000000 ) ) ;
#95436 = ORIENTED_EDGE ( 'NONE', *, *, #23968, .F. ) ;
#95437 = CONICAL_SURFACE ( 'NONE', #36861, 0.09999999999999982514, 0.003490658503988666988 ) ;
#95438 = CARTESIAN_POINT ( 'NONE',  ( -13.14999999999999147, 2.500000000000000000, 2.411473670974877415 ) ) ;
#95439 = ORIENTED_EDGE ( 'NONE', *, *, #16883, .T. ) ;
#95440 = LINE ( 'NONE', #45701, #126971 ) ;
#95441 = CARTESIAN_POINT ( 'NONE',  ( 16.04820284657690621, -2.500000000000000444, -6.585610460626504903 ) ) ;
#95442 = DIRECTION ( 'NONE',  ( 0.000000000000000000, 0.000000000000000000, -1.000000000000000000 ) ) ;
#95443 = PLANE ( 'NONE',  #111218 ) ;
#95444 = CONICAL_SURFACE ( 'NONE', #39041, 0.09999999999999982514, 0.003490658503988666988 ) ;
#95445 = ORIENTED_EDGE ( 'NONE', *, *, #77619, .F. ) ;
#95447 = CIRCLE ( 'NONE', #47330, 0.1000000000000002554 ) ;
#95446 = AXIS2_PLACEMENT_3D ( 'NONE', #12905, #24052, #72513 ) ;
#95448 = VERTEX_POINT ( 'NONE', #16795 ) ;
#95449 = ORIENTED_EDGE ( 'NONE', *, *, #76925, .T. ) ;
#95450 = DIRECTION ( 'NONE',  ( -4.274815082592931898E-19, -0.9999939076577903929, -0.003490651415223739937 ) ) ;
#95451 = FACE_OUTER_BOUND ( 'NONE', #89524, .T. ) ;
#95452 = FACE_OUTER_BOUND ( 'NONE', #67972, .T. ) ;
#95453 = FACE_BOUND ( 'NONE', #1717, .T. ) ;
#95454 = LINE ( 'NONE', #45716, #57708 ) ;
#95455 = FACE_OUTER_BOUND ( 'NONE', #87858, .T. ) ;
#95456 = CARTESIAN_POINT ( 'NONE',  ( 7.949999999999925571, 12.50000000000000000, -6.430097255199264339 ) ) ;
#95457 = CARTESIAN_POINT ( 'NONE',  ( -4.119968255444916849E-14, 2.500000000000000000, 3.637306695894644726 ) ) ;
#95458 = ADVANCED_FACE ( 'NONE', ( #56720 ), #43419, .T. ) ;
#95459 = CARTESIAN_POINT ( 'NONE',  ( 8.349999999999919709, 2.500000000000000000, 6.595190528383296780 ) ) ;
#95460 = CARTESIAN_POINT ( 'NONE',  ( 1.899999999999951283, 2.500000000000000000, 0.2464101615137736789 ) ) ;
#95461 = DIRECTION ( 'NONE',  ( 0.000000000000000000, -0.000000000000000000, 1.000000000000000000 ) ) ;
#95462 = CARTESIAN_POINT ( 'NONE',  ( -3.100000000000028955, 2.500000000000000000, 4.676537180435972552 ) ) ;
#95463 = ORIENTED_EDGE ( 'NONE', *, *, #50314, .T. ) ;
#95464 = EDGE_LOOP ( 'NONE', ( #83590, #85663, #41055, #73305 ) ) ;
#95465 = ORIENTED_EDGE ( 'NONE', *, *, #33736, .F. ) ;
#95466 = ORIENTED_EDGE ( 'NONE', *, *, #106024, .T. ) ;
#95467 = ADVANCED_FACE ( 'NONE', ( #20702 ), #49100, .T. ) ;
#95468 = DIRECTION ( 'NONE',  ( -4.274815082592931898E-19, -0.9999939076577903929, -0.003490651415223739937 ) ) ;
#95469 = FACE_BOUND ( 'NONE', #60563, .T. ) ;
#95470 = DIRECTION ( 'NONE',  ( 0.000000000000000000, 1.000000000000000000, 0.000000000000000000 ) ) ;
#95471 = AXIS2_PLACEMENT_3D ( 'NONE', #109346, #99545, #1321 ) ;
#95472 = CONICAL_SURFACE ( 'NONE', #93329, 0.09999999999999982514, 0.003490658503988666988 ) ;
#95473 = ORIENTED_EDGE ( 'NONE', *, *, #73202, .F. ) ;
#95474 = DIRECTION ( 'NONE',  ( -4.274815082592931898E-19, -0.9999939076577903929, -0.003490651415223739937 ) ) ;
#95475 = DIRECTION ( 'NONE',  ( 0.000000000000000000, 1.000000000000000000, 0.000000000000000000 ) ) ;
#95476 = VERTEX_POINT ( 'NONE', #69795 ) ;
#95477 = CARTESIAN_POINT ( 'NONE',  ( -12.09999999999999609, 2.500000000000000000, 0.5928203230275536084 ) ) ;
#95478 = FACE_OUTER_BOUND ( 'NONE', #87848, .T. ) ;
#95480 = VECTOR ( 'NONE', #121869, 1000.000000000000000 ) ;
#95479 = AXIS2_PLACEMENT_3D ( 'NONE', #37955, #95589, #47139 ) ;
#95481 = ORIENTED_EDGE ( 'NONE', *, *, #48165, .T. ) ;
#95482 = DIRECTION ( 'NONE',  ( -4.274815082592931898E-19, -0.9999939076577903929, -0.003490651415223739937 ) ) ;
#95484 = CONICAL_SURFACE ( 'NONE', #39082, 0.1000000000000002554, 0.003490658503988666988 ) ;
#95483 = LINE ( 'NONE', #5793, #9961 ) ;
#95486 = CIRCLE ( 'NONE', #105952, 0.09999999999999982514 ) ;
#95485 = CIRCLE ( 'NONE', #47383, 0.09999999999999999167 ) ;
#95487 = VERTEX_POINT ( 'NONE', #68497 ) ;
#95489 = EDGE_CURVE ( 'NONE', #122496, #43147, #99269, .T. ) ;
#95488 = AXIS2_PLACEMENT_3D ( 'NONE', #45424, #85334, #34973 ) ;
#95490 = CARTESIAN_POINT ( 'NONE',  ( 7.899999999999924860, 2.500000000000000000, -3.637306695894650055 ) ) ;
#95491 = CARTESIAN_POINT ( 'NONE',  ( -13.54999999999999005, 12.50000000000000000, 2.511473670974877503 ) ) ;
#95492 = ORIENTED_EDGE ( 'NONE', *, *, #19716, .T. ) ;
#95493 = DIRECTION ( 'NONE',  ( 0.000000000000000000, -0.9999939076577903929, 0.003490651415223739937 ) ) ;
#95494 = ORIENTED_EDGE ( 'NONE', *, *, #108528, .F. ) ;
#95495 = ORIENTED_EDGE ( 'NONE', *, *, #95361, .T. ) ;
#95496 = FACE_OUTER_BOUND ( 'NONE', #62294, .T. ) ;
#95497 = EDGE_CURVE ( 'NONE', #78788, #22205, #40351, .T. ) ;
#95498 = ORIENTED_EDGE ( 'NONE', *, *, #56789, .F. ) ;
#95499 = LINE ( 'NONE', #86306, #17734 ) ;
#95500 = DIRECTION ( 'NONE',  ( 0.000000000000000000, -0.9999939076577903929, 0.003490651415223739937 ) ) ;
#95501 = VERTEX_POINT ( 'NONE', #9588 ) ;
#95502 = DIRECTION ( 'NONE',  ( 0.000000000000000000, 0.000000000000000000, -1.000000000000000000 ) ) ;
#95503 = DIRECTION ( 'NONE',  ( 0.000000000000000000, 0.000000000000000000, 1.000000000000000000 ) ) ;
#95504 = DIRECTION ( 'NONE',  ( 0.000000000000000000, 0.000000000000000000, -1.000000000000000000 ) ) ;
#95505 = EDGE_CURVE ( 'NONE', #127904, #99888, #10821, .T. ) ;
#95506 = ADVANCED_FACE ( 'NONE', ( #119527 ), #122254, .T. ) ;
#95507 = CARTESIAN_POINT ( 'NONE',  ( -3.550000000000027800, 2.500000000000000000, 6.148780366869520009 ) ) ;
#95508 = EDGE_CURVE ( 'NONE', #81743, #82923, #95061, .T. ) ;
#95509 = DIRECTION ( 'NONE',  ( 0.000000000000000000, 0.000000000000000000, 1.000000000000000000 ) ) ;
#95510 = EDGE_CURVE ( 'NONE', #62380, #29817, #38643, .T. ) ;
#95511 = AXIS2_PLACEMENT_3D ( 'NONE', #25288, #54755, #75684 ) ;
#95512 = ADVANCED_FACE ( 'NONE', ( #70443 ), #60002, .T. ) ;
#95514 = CIRCLE ( 'NONE', #28619, 0.1000000000000002554 ) ;
#95513 = CARTESIAN_POINT ( 'NONE',  ( 8.349999999999919709, 2.500000000000000000, 5.802370205355744659 ) ) ;
#95515 = AXIS2_PLACEMENT_3D ( 'NONE', #9214, #106757, #119166 ) ;
#95516 = ORIENTED_EDGE ( 'NONE', *, *, #75847, .F. ) ;
#95517 = EDGE_LOOP ( 'NONE', ( #31228, #15639 ) ) ;
#95518 = FACE_OUTER_BOUND ( 'NONE', #16863, .T. ) ;
#95519 = AXIS2_PLACEMENT_3D ( 'NONE', #19793, #66932, #77418 ) ;
#95520 = DIRECTION ( 'NONE',  ( 0.000000000000000000, 1.000000000000000000, 0.000000000000000000 ) ) ;
#95521 = CARTESIAN_POINT ( 'NONE',  ( 11.44999999999991047, 12.50000000000000000, 6.083687093685482772 ) ) ;
#95523 = ORIENTED_EDGE ( 'NONE', *, *, #86705, .F. ) ;
#95522 = VERTEX_POINT ( 'NONE', #120830 ) ;
#95524 = ORIENTED_EDGE ( 'NONE', *, *, #45463, .T. ) ;
#95525 = ADVANCED_FACE ( 'NONE', ( #128745 ), #17674, .T. ) ;
#95526 = CARTESIAN_POINT ( 'NONE',  ( -3.100000000000028955, 2.500000000000000000, 4.676537180435972552 ) ) ;
#95527 = CONICAL_SURFACE ( 'NONE', #39112, 0.1000000000000000056, 0.003490658503988666988 ) ;
#95528 = CIRCLE ( 'NONE', #108030, 0.1000000000000002554 ) ;
#95529 = ADVANCED_FACE ( 'NONE', ( #10235 ), #18753, .T. ) ;
#95530 = CARTESIAN_POINT ( 'NONE',  ( -1.450000000000035039, 2.500000000000000000, -6.941600689897077459 ) ) ;
#95531 = EDGE_CURVE ( 'NONE', #94071, #105417, #8921, .T. ) ;
#95532 = DIRECTION ( 'NONE',  ( -4.274815082592931898E-19, -0.9999939076577903929, -0.003490651415223739937 ) ) ;
#95533 = CIRCLE ( 'NONE', #112259, 0.1000000000000002554 ) ;
#95534 = DIRECTION ( 'NONE',  ( 1.000000000000000000, 0.000000000000000000, 0.000000000000000000 ) ) ;
#95535 = CARTESIAN_POINT ( 'NONE',  ( -0.8500000000000382805, 2.500000000000000000, -7.188010851410854052 ) ) ;
#95536 = FACE_OUTER_BOUND ( 'NONE', #56186, .T. ) ;
#95537 = CARTESIAN_POINT ( 'NONE',  ( 12.29999999999990301, 2.500000000000000000, -0.3464101615137782364 ) ) ;
#95538 = DIRECTION ( 'NONE',  ( -4.274815082592931898E-19, -0.9999939076577903929, -0.003490651415223739937 ) ) ;
#95539 = DIRECTION ( 'NONE',  ( 0.000000000000000000, 0.000000000000000000, 1.000000000000000000 ) ) ;
#95540 = FACE_OUTER_BOUND ( 'NONE', #5597, .T. ) ;
#95541 = ORIENTED_EDGE ( 'NONE', *, *, #8150, .T. ) ;
#95543 = AXIS2_PLACEMENT_3D ( 'NONE', #23688, #55720, #5961 ) ;
#95542 = VECTOR ( 'NONE', #359, 1000.000000000000000 ) ;
#95544 = CARTESIAN_POINT ( 'NONE',  ( -6.250000000000015987, 2.500000000000000000, 5.802370205355744659 ) ) ;
#95545 = EDGE_LOOP ( 'NONE', ( #70782, #55328, #69973, #109231 ) ) ;
#95546 = ORIENTED_EDGE ( 'NONE', *, *, #20199, .T. ) ;
#95547 = DIRECTION ( 'NONE',  ( -0.000000000000000000, -1.000000000000000000, -0.000000000000000000 ) ) ;
#95548 = CARTESIAN_POINT ( 'NONE',  ( 9.999999999999911182, 2.500000000000000000, 4.922947341949748257 ) ) ;
#95549 = CARTESIAN_POINT ( 'NONE',  ( 13.29999999999989946, 12.50000000000000000, -2.385244779468109755E-15 ) ) ;
#95550 = LINE ( 'NONE', #85077, #127781 ) ;
#95551 = CARTESIAN_POINT ( 'NONE',  ( -2.900000000000029665, 12.50000000000000000, 4.330127018922196314 ) ) ;
#95552 = DIRECTION ( 'NONE',  ( 0.000000000000000000, -0.9999939076577903929, 0.003490651415223739937 ) ) ;
#95553 = PLANE ( 'NONE',  #109621 ) ;
#95554 = VERTEX_POINT ( 'NONE', #118247 ) ;
#95555 = CARTESIAN_POINT ( 'NONE',  ( 13.34999999999990017, 2.500000000000000000, 2.757883832488649656 ) ) ;
#95556 = AXIS2_PLACEMENT_3D ( 'NONE', #55425, #62676, #75063 ) ;
#95557 = EDGE_CURVE ( 'NONE', #66518, #110514, #29243, .T. ) ;
#95558 = LINE ( 'NONE', #106021, #58280 ) ;
#95559 = VERTEX_POINT ( 'NONE', #109048 ) ;
#95560 = EDGE_LOOP ( 'NONE', ( #51140, #48090, #105378, #128187 ) ) ;
#95561 = EDGE_CURVE ( 'NONE', #21383, #32164, #19388, .T. ) ;
#95562 = ORIENTED_EDGE ( 'NONE', *, *, #82357, .F. ) ;
#95563 = ADVANCED_FACE ( 'NONE', ( #79615 ), #29872, .T. ) ;
#95564 = ORIENTED_EDGE ( 'NONE', *, *, #105107, .T. ) ;
#95565 = CARTESIAN_POINT ( 'NONE',  ( -1.250000000000035749, 12.50000000000000000, -2.857883832488653741 ) ) ;
#95566 = DIRECTION ( 'NONE',  ( 0.000000000000000000, 1.000000000000000000, 0.000000000000000000 ) ) ;
#95567 = EDGE_CURVE ( 'NONE', #124646, #13639, #13466, .T. ) ;
#95568 = AXIS2_PLACEMENT_3D ( 'NONE', #18226, #67300, #58183 ) ;
#95569 = DIRECTION ( 'NONE',  ( 0.000000000000000000, -0.9999939076577903929, 0.003490651415223739937 ) ) ;
#95571 = CARTESIAN_POINT ( 'NONE',  ( 14.19999999999989626, 12.50000000000000000, -0.06509327318403970719 ) ) ;
#95570 = CIRCLE ( 'NONE', #28675, 0.06509327318403745899 ) ;
#95572 = EDGE_CURVE ( 'NONE', #46914, #103864, #63690, .T. ) ;
#95573 = CARTESIAN_POINT ( 'NONE',  ( 0.8499999999999527933, 12.50000000000000000, 7.188010851410848723 ) ) ;
#95574 = VERTEX_POINT ( 'NONE', #64319 ) ;
#95575 = DIRECTION ( 'NONE',  ( 0.000000000000000000, -0.000000000000000000, 1.000000000000000000 ) ) ;
#95576 = ADVANCED_FACE ( 'NONE', ( #14562 ), #99271, .T. ) ;
#95578 = AXIS2_PLACEMENT_3D ( 'NONE', #23032, #20880, #68682 ) ;
#95577 = VECTOR ( 'NONE', #58096, 1000.000000000000000 ) ;
#95579 = DIRECTION ( 'NONE',  ( -4.274815082592931898E-19, -0.9999939076577903929, -0.003490651415223739937 ) ) ;
#95580 = ORIENTED_EDGE ( 'NONE', *, *, #125098, .F. ) ;
#95581 = EDGE_LOOP ( 'NONE', ( #35971, #76150 ) ) ;
#95582 = ORIENTED_EDGE ( 'NONE', *, *, #14063, .T. ) ;
#95583 = DIRECTION ( 'NONE',  ( 0.000000000000000000, 0.000000000000000000, 1.000000000000000000 ) ) ;
#95585 = AXIS2_PLACEMENT_3D ( 'NONE', #55544, #45726, #102690 ) ;
#95584 = AXIS2_PLACEMENT_3D ( 'NONE', #82213, #31822, #80931 ) ;
#95586 = DIRECTION ( 'NONE',  ( -0.000000000000000000, -1.000000000000000000, -0.000000000000000000 ) ) ;
#95587 = PLANE ( 'NONE',  #6305 ) ;
#95588 = EDGE_LOOP ( 'NONE', ( #11953, #101759, #30481, #68455 ) ) ;
#95589 = DIRECTION ( 'NONE',  ( -0.000000000000000000, -1.000000000000000000, -0.000000000000000000 ) ) ;
#95590 = CARTESIAN_POINT ( 'NONE',  ( 6.249999999999965361, 2.500000000000000000, 2.065063509461097624 ) ) ;
#95591 = FACE_OUTER_BOUND ( 'NONE', #55593, .T. ) ;
#95592 = CARTESIAN_POINT ( 'NONE',  ( -11.64999999999999680, 2.500000000000000000, 5.802370205355744659 ) ) ;
#95593 = EDGE_CURVE ( 'NONE', #70324, #13448, #53210, .T. ) ;
#95594 = DIRECTION ( 'NONE',  ( 0.000000000000000000, 0.000000000000000000, 1.000000000000000000 ) ) ;
#95595 = ORIENTED_EDGE ( 'NONE', *, *, #14852, .T. ) ;
#95596 = CONICAL_SURFACE ( 'NONE', #106057, 0.09999999999999999167, 0.003490658503988666988 ) ;
#95597 = DIRECTION ( 'NONE',  ( 0.000000000000000000, 1.000000000000000000, 0.000000000000000000 ) ) ;
#95598 = ORIENTED_EDGE ( 'NONE', *, *, #124478, .T. ) ;
#95599 = ORIENTED_EDGE ( 'NONE', *, *, #71898, .F. ) ;
#95600 = ORIENTED_EDGE ( 'NONE', *, *, #96237, .F. ) ;
#95601 = LINE ( 'NONE', #15066, #33553 ) ;
#95602 = FACE_BOUND ( 'NONE', #97353, .T. ) ;
#95603 = CARTESIAN_POINT ( 'NONE',  ( 8.099999999999921485, 2.500000000000000000, 0.3464101615137735735 ) ) ;
#95604 = CIRCLE ( 'NONE', #62171, 0.1000000000000000472 ) ;
#95605 = DIRECTION ( 'NONE',  ( -0.000000000000000000, -1.000000000000000000, -0.000000000000000000 ) ) ;
#95606 = MECHANICAL_DESIGN_GEOMETRIC_PRESENTATION_REPRESENTATION (  '', ( #89351 ), #110273 ) ;
#95607 = EDGE_CURVE ( 'NONE', #40320, #14309, #75420, .T. ) ;
#95608 = ORIENTED_EDGE ( 'NONE', *, *, #108357, .F. ) ;
#95609 = DIRECTION ( 'NONE',  ( 0.000000000000000000, 0.000000000000000000, 1.000000000000000000 ) ) ;
#95610 = DIRECTION ( 'NONE',  ( -4.274815082592931898E-19, -0.9999939076577903929, -0.003490651415223739937 ) ) ;
#95612 = DIRECTION ( 'NONE',  ( 0.000000000000000000, -0.000000000000000000, 1.000000000000000000 ) ) ;
#95611 = VECTOR ( 'NONE', #92594, 1000.000000000000000 ) ;
#95614 = PLANE ( 'NONE',  #122080 ) ;
#95613 = AXIS2_PLACEMENT_3D ( 'NONE', #95326, #125430, #26589 ) ;
#95615 = EDGE_LOOP ( 'NONE', ( #123292, #104558, #121143, #4053 ) ) ;
#95616 = LINE ( 'NONE', #6542, #122192 ) ;
#95617 = AXIS2_PLACEMENT_3D ( 'NONE', #30368, #21164, #91203 ) ;
#95618 = VECTOR ( 'NONE', #126343, 1000.000000000000000 ) ;
#95619 = DIRECTION ( 'NONE',  ( -0.000000000000000000, 1.000000000000000000, -0.000000000000000000 ) ) ;
#95620 = ORIENTED_EDGE ( 'NONE', *, *, #6548, .F. ) ;
#95621 = DIRECTION ( 'NONE',  ( 0.000000000000000000, 1.000000000000000000, 0.000000000000000000 ) ) ;
#95622 = CIRCLE ( 'NONE', #68424, 0.06509327318403745899 ) ;
#95623 = EDGE_CURVE ( 'NONE', #100019, #113079, #90844, .T. ) ;
#95624 = FACE_BOUND ( 'NONE', #2392, .T. ) ;
#95625 = CYLINDRICAL_SURFACE ( 'NONE', #40988, 1.388921157871086942 ) ;
#95627 = CIRCLE ( 'NONE', #103948, 0.06509327318403745899 ) ;
#95626 = AXIS2_PLACEMENT_3D ( 'NONE', #57872, #29065, #29693 ) ;
#95628 = EDGE_LOOP ( 'NONE', ( #97568, #667 ) ) ;
#95629 = CARTESIAN_POINT ( 'NONE',  ( 7.099999999999928590, 12.50000000000000000, -4.395220292106239768 ) ) ;
#95630 = CARTESIAN_POINT ( 'NONE',  ( 3.749999999999975131, 2.500000000000000000, 6.395190528383296602 ) ) ;
#95631 = ORIENTED_EDGE ( 'NONE', *, *, #26797, .T. ) ;
#95632 = EDGE_LOOP ( 'NONE', ( #48049, #37653 ) ) ;
#95633 = CARTESIAN_POINT ( 'NONE',  ( 184.8802083336747444, 4.367472073101515306, 7.564683531250000925 ) ) ;
#95634 = ORIENTED_EDGE ( 'NONE', *, *, #3758, .F. ) ;
#95635 = CARTESIAN_POINT ( 'NONE',  ( 185.9635416670080588, -4.367472073101520635, 7.564683531249999149 ) ) ;
#95636 = CARTESIAN_POINT ( 'NONE',  ( -1.850000000000033396, 12.50000000000000000, -2.576566944158915184 ) ) ;
#95637 = CARTESIAN_POINT ( 'NONE',  ( -3.350000000000028511, 2.500000000000000000, 1.372243186433545370 ) ) ;
#95638 = CARTESIAN_POINT ( 'NONE',  ( -4.400000000000025224, 12.50000000000000000, -0.2813168883297409439 ) ) ;
#95639 = CARTESIAN_POINT ( 'NONE',  ( -1.250000000000037970, 12.50000000000000000, 2.792790559304612064 ) ) ;
#95640 = CONICAL_SURFACE ( 'NONE', #53777, 0.09999999999999999167, 0.003490658503988666988 ) ;
#95641 = VERTEX_POINT ( 'NONE', #104249 ) ;
#95643 = ORIENTED_EDGE ( 'NONE', *, *, #32308, .F. ) ;
#95642 = EDGE_CURVE ( 'NONE', #30305, #35899, #86639, .T. ) ;
#95644 = DIRECTION ( 'NONE',  ( 0.000000000000000000, 0.000000000000000000, 1.000000000000000000 ) ) ;
#95645 = CARTESIAN_POINT ( 'NONE',  ( 187.5000000000000000, 0.000000000000000000, 7.700000000000000178 ) ) ;
#95646 = DIRECTION ( 'NONE',  ( -0.000000000000000000, 1.000000000000000000, -0.000000000000000000 ) ) ;
#95647 = CARTESIAN_POINT ( 'NONE',  ( 10.39999999999991331, 2.500000000000000000, -2.385244779468109755E-15 ) ) ;
#95649 = ORIENTED_EDGE ( 'NONE', *, *, #109226, .F. ) ;
#95648 = EDGE_LOOP ( 'NONE', ( #124982, #103276, #92973, #60616 ) ) ;
#95650 = DIRECTION ( 'NONE',  ( 0.000000000000000000, 0.000000000000000000, 1.000000000000000000 ) ) ;
#95651 = ORIENTED_EDGE ( 'NONE', *, *, #20867, .F. ) ;
#95652 = PLANE ( 'NONE',  #124502 ) ;
#95653 = CARTESIAN_POINT ( 'NONE',  ( -10.00000000000000533, 12.50000000000000000, 0.6277270498435120194 ) ) ;
#95654 = ORIENTED_EDGE ( 'NONE', *, *, #92568, .T. ) ;
#95656 = EDGE_CURVE ( 'NONE', #42231, #18847, #114071, .T. ) ;
#95655 = DIRECTION ( 'NONE',  ( 0.000000000000000000, -0.000000000000000000, 1.000000000000000000 ) ) ;
#95657 = DIRECTION ( 'NONE',  ( 0.000000000000000000, 0.000000000000000000, 1.000000000000000000 ) ) ;
#95658 = AXIS2_PLACEMENT_3D ( 'NONE', #48681, #68303, #87297 ) ;
#95659 = DIRECTION ( 'NONE',  ( 0.000000000000000000, 1.000000000000000000, 0.000000000000000000 ) ) ;
#95660 = FACE_OUTER_BOUND ( 'NONE', #89325, .T. ) ;
#95661 = CARTESIAN_POINT ( 'NONE',  ( 11.04999999999990656, 2.500000000000000000, 2.511473670974873507 ) ) ;
#95662 = DIRECTION ( 'NONE',  ( -4.274815082592931898E-19, -0.9999939076577903929, -0.003490651415223739937 ) ) ;
#95663 = EDGE_CURVE ( 'NONE', #97017, #40454, #76184, .T. ) ;
#95664 = EDGE_CURVE ( 'NONE', #76810, #66380, #35521, .T. ) ;
#95665 = DIRECTION ( 'NONE',  ( 0.000000000000000000, 0.000000000000000000, 1.000000000000000000 ) ) ;
#95666 = CYLINDRICAL_SURFACE ( 'NONE', #127982, 5.000000000000004441 ) ;
#95667 = ADVANCED_FACE ( 'NONE', ( #103614 ), #85252, .T. ) ;
#95668 = EDGE_CURVE ( 'NONE', #54565, #81006, #104872, .T. ) ;
#95669 = CARTESIAN_POINT ( 'NONE',  ( 3.099999999999945466, 2.500000000000000000, -3.983716857408426293 ) ) ;
#95670 = AXIS2_PLACEMENT_3D ( 'NONE', #69176, #60681, #98002 ) ;
#95671 = ORIENTED_EDGE ( 'NONE', *, *, #71147, .F. ) ;
#95672 = AXIS2_PLACEMENT_3D ( 'NONE', #34852, #25642, #123837 ) ;
#95674 = ORIENTED_EDGE ( 'NONE', *, *, #37165, .F. ) ;
#95673 = CIRCLE ( 'NONE', #39266, 0.06509327318403745899 ) ;
#95675 = CARTESIAN_POINT ( 'NONE',  ( 2.049999999999950084, 12.50000000000000000, 2.230156782645134950 ) ) ;
#95676 = VERTEX_POINT ( 'NONE', #115323 ) ;
#95677 = ADVANCED_FACE ( 'NONE', ( #36163 ), #46952, .T. ) ;
#95678 = CARTESIAN_POINT ( 'NONE',  ( 4.599999999999937472, 2.500000000000000000, 0.6928203230275494784 ) ) ;
#95681 = VERTEX_POINT ( 'NONE', #4732 ) ;
#95680 = EDGE_LOOP ( 'NONE', ( #123920, #41813 ) ) ;
#95679 = EDGE_CURVE ( 'NONE', #42325, #89946, #25679, .T. ) ;
#95682 = ORIENTED_EDGE ( 'NONE', *, *, #51381, .T. ) ;
#95683 = EDGE_CURVE ( 'NONE', #52044, #95641, #88792, .T. ) ;
#95684 = DIRECTION ( 'NONE',  ( -0.000000000000000000, -1.000000000000000000, -0.000000000000000000 ) ) ;
#95685 = EDGE_CURVE ( 'NONE', #23954, #95574, #26342, .T. ) ;
#95686 = AXIS2_PLACEMENT_3D ( 'NONE', #15121, #53153, #55077 ) ;
#95687 = ADVANCED_FACE ( 'NONE', ( #74796 ), #114702, .T. ) ;
#95688 = CARTESIAN_POINT ( 'NONE',  ( 12.29999999999990656, 12.50000000000000000, 3.918623584224383727 ) ) ;
#95689 =( NAMED_UNIT ( * ) SI_UNIT ( $, .STERADIAN. ) SOLID_ANGLE_UNIT ( ) );
#95690 = CARTESIAN_POINT ( 'NONE',  ( 2.899999999999946620, 12.50000000000000000, -0.6928203230275542523 ) ) ;
#95691 = CARTESIAN_POINT ( 'NONE',  ( 6.449999999999930012, 12.50000000000000000, 1.753560074763284016 ) ) ;
#95692 = LINE ( 'NONE', #84576, #114439 ) ;
#95693 = CIRCLE ( 'NONE', #83262, 0.1000000000000002554 ) ;
#95694 = ORIENTED_EDGE ( 'NONE', *, *, #77988, .T. ) ;
#95695 = EDGE_CURVE ( 'NONE', #98508, #6453, #63672, .T. ) ;
#95696 = CARTESIAN_POINT ( 'NONE',  ( 8.749999999999923617, 2.500000000000000000, -7.088010851410853519 ) ) ;
#95697 = ORIENTED_EDGE ( 'NONE', *, *, #92894, .T. ) ;
#95698 = VERTEX_POINT ( 'NONE', #96427 ) ;
#95699 = ORIENTED_EDGE ( 'NONE', *, *, #61518, .T. ) ;
#95700 = ORIENTED_EDGE ( 'NONE', *, *, #68764, .F. ) ;
#95701 = DIRECTION ( 'NONE',  ( 0.000000000000000000, -0.000000000000000000, 1.000000000000000000 ) ) ;
#95702 = ORIENTED_EDGE ( 'NONE', *, *, #78736, .T. ) ;
#95703 = ORIENTED_EDGE ( 'NONE', *, *, #60247, .T. ) ;
#95704 = CIRCLE ( 'NONE', #122790, 0.1000000000000000472 ) ;
#95706 = CARTESIAN_POINT ( 'NONE',  ( -6.650000000000014566, 2.500000000000000000, 5.702370205355745014 ) ) ;
#95705 = CONICAL_SURFACE ( 'NONE', #39299, 0.09999999999999982514, 0.003490658503988666988 ) ;
#95707 = FACE_OUTER_BOUND ( 'NONE', #74659, .T. ) ;
#95709 = AXIS2_PLACEMENT_3D ( 'NONE', #55187, #95112, #113456 ) ;
#95708 = CARTESIAN_POINT ( 'NONE',  ( 0.3999999999999628852, 12.50000000000000000, -0.6928203230275520319 ) ) ;
#95710 = DIRECTION ( 'NONE',  ( 0.000000000000000000, -0.000000000000000000, 1.000000000000000000 ) ) ;
#95711 = DIRECTION ( 'NONE',  ( 0.000000000000000000, -0.000000000000000000, 1.000000000000000000 ) ) ;
#95712 = CARTESIAN_POINT ( 'NONE',  ( 2.299999999999948752, 2.500000000000000000, 0.3464101615137735735 ) ) ;
#95713 = ORIENTED_EDGE ( 'NONE', *, *, #66214, .F. ) ;
#95715 = AXIS2_PLACEMENT_3D ( 'NONE', #48161, #18038, #28523 ) ;
#95714 = DIRECTION ( 'NONE',  ( 0.000000000000000000, 1.000000000000000000, 0.000000000000000000 ) ) ;
#95716 = ORIENTED_EDGE ( 'NONE', *, *, #115899, .F. ) ;
#95717 = DIRECTION ( 'NONE',  ( 0.000000000000000000, 0.000000000000000000, 1.000000000000000000 ) ) ;
#95718 = ORIENTED_EDGE ( 'NONE', *, *, #12039, .F. ) ;
#95719 = DIRECTION ( 'NONE',  ( -4.274815082592931898E-19, -0.9999939076577903929, -0.003490651415223739937 ) ) ;
#95720 = ORIENTED_EDGE ( 'NONE', *, *, #88836, .T. ) ;
#95721 = AXIS2_PLACEMENT_3D ( 'NONE', #29217, #129361, #118866 ) ;
#95722 = EDGE_LOOP ( 'NONE', ( #126556, #43020, #100678, #19594 ) ) ;
#95723 = CARTESIAN_POINT ( 'NONE',  ( 3.749999999999944045, 2.500000000000000000, -2.957883832488653830 ) ) ;
#95724 = CARTESIAN_POINT ( 'NONE',  ( -13.09999999999999254, 2.500000000000000000, -3.983716857408423628 ) ) ;
#95725 = EDGE_CURVE ( 'NONE', #58662, #53518, #48003, .T. ) ;
#95727 = AXIS2_PLACEMENT_3D ( 'NONE', #67564, #78046, #57112 ) ;
#95726 = CIRCLE ( 'NONE', #51816, 0.06509327318403745899 ) ;
#95728 = FACE_OUTER_BOUND ( 'NONE', #35044, .T. ) ;
#95729 = DIRECTION ( 'NONE',  ( 0.000000000000000000, 0.000000000000000000, -1.000000000000000000 ) ) ;
#95730 = EDGE_CURVE ( 'NONE', #53628, #53022, #26103, .T. ) ;
#95731 = DIRECTION ( 'NONE',  ( 0.000000000000000000, 0.000000000000000000, 1.000000000000000000 ) ) ;
#95732 = ORIENTED_EDGE ( 'NONE', *, *, #59205, .T. ) ;
#95733 = DIRECTION ( 'NONE',  ( 0.000000000000000000, 0.000000000000000000, 1.000000000000000000 ) ) ;
#95734 = LINE ( 'NONE', #97654, #20095 ) ;
#95735 = CARTESIAN_POINT ( 'NONE',  ( 0.8499999999999553468, 12.50000000000000000, -2.857883832488653741 ) ) ;
#95736 = DIRECTION ( 'NONE',  ( -4.274815082592931898E-19, -0.9999939076577903929, -0.003490651415223739937 ) ) ;
#95737 = ADVANCED_FACE ( 'NONE', ( #17202 ), #99171, .T. ) ;
#95738 = FACE_OUTER_BOUND ( 'NONE', #36220, .T. ) ;
#95739 = EDGE_LOOP ( 'NONE', ( #9024, #12866, #91143, #87298 ) ) ;
#95740 = VERTEX_POINT ( 'NONE', #6738 ) ;
#95741 = ORIENTED_EDGE ( 'NONE', *, *, #75159, .F. ) ;
#95742 = FACE_OUTER_BOUND ( 'NONE', #119032, .T. ) ;
#95743 = CARTESIAN_POINT ( 'NONE',  ( -9.550000000000006040, 12.50000000000000000, -2.165063509461101710 ) ) ;
#95744 = CIRCLE ( 'NONE', #76964, 0.1000000000000000056 ) ;
#95745 = CARTESIAN_POINT ( 'NONE',  ( 186.6250000000000284, -8.891194145520236347, -1.633285867636356693E-15 ) ) ;
#95746 = CARTESIAN_POINT ( 'NONE',  ( -8.950000000000009948, 2.500000000000000000, 2.611473670974873151 ) ) ;
#95747 = LINE ( 'NONE', #104900, #13101 ) ;
#95748 = DIRECTION ( 'NONE',  ( -0.000000000000000000, -1.000000000000000000, -0.000000000000000000 ) ) ;
#95749 = DIRECTION ( 'NONE',  ( 0.000000000000000000, 0.000000000000000000, 1.000000000000000000 ) ) ;
#95750 = ORIENTED_EDGE ( 'NONE', *, *, #46331, .T. ) ;
#95751 = AXIS2_PLACEMENT_3D ( 'NONE', #49191, #107438, #108720 ) ;
#95752 = VECTOR ( 'NONE', #122484, 1000.000000000000000 ) ;
#95753 = CARTESIAN_POINT ( 'NONE',  ( -14.99999999999998401, 2.500000000000000000, 0.5928203230275517210 ) ) ;
#95754 = CARTESIAN_POINT ( 'NONE',  ( -8.950000000000009948, 12.50000000000000000, 2.511473670974873507 ) ) ;
#95755 = ORIENTED_EDGE ( 'NONE', *, *, #122695, .T. ) ;
#95756 = DIRECTION ( 'NONE',  ( 0.000000000000000000, 1.000000000000000000, 0.000000000000000000 ) ) ;
#95757 = FACE_OUTER_BOUND ( 'NONE', #70490, .T. ) ;
#95758 = CIRCLE ( 'NONE', #18387, 0.06509327318403745899 ) ;
#95759 = CARTESIAN_POINT ( 'NONE',  ( -10.00000000000000355, 2.500000000000000000, -0.7928203230275542301 ) ) ;
#95760 = AXIS2_PLACEMENT_3D ( 'NONE', #117789, #99480, #48430 ) ;
#95761 = ORIENTED_EDGE ( 'NONE', *, *, #87938, .F. ) ;
#95762 = DIRECTION ( 'NONE',  ( -0.000000000000000000, 1.000000000000000000, -0.000000000000000000 ) ) ;
#95763 = ORIENTED_EDGE ( 'NONE', *, *, #34707, .F. ) ;
#95764 = LINE ( 'NONE', #105593, #2030 ) ;
#95765 = CARTESIAN_POINT ( 'NONE',  ( -13.14999999999999147, 12.50000000000000000, 1.753560074763288013 ) ) ;
#95766 = EDGE_LOOP ( 'NONE', ( #33785, #9911, #83217, #14994 ) ) ;
#95767 = DIRECTION ( 'NONE',  ( -0.000000000000000000, -1.000000000000000000, -0.000000000000000000 ) ) ;
#95768 = DIRECTION ( 'NONE',  ( 0.000000000000000000, -0.000000000000000000, 1.000000000000000000 ) ) ;
#95769 = EDGE_CURVE ( 'NONE', #100605, #93533, #42853, .T. ) ;
#95770 = AXIS2_PLACEMENT_3D ( 'NONE', #91216, #82701, #1533 ) ;
#95771 = ORIENTED_EDGE ( 'NONE', *, *, #70567, .T. ) ;
#95772 = EDGE_CURVE ( 'NONE', #129184, #83779, #42764, .T. ) ;
#95773 = ORIENTED_EDGE ( 'NONE', *, *, #94034, .T. ) ;
#95774 = CARTESIAN_POINT ( 'NONE',  ( 5.599999999999934808, 2.500000000000000000, -3.983716857408426293 ) ) ;
#95775 = AXIS2_PLACEMENT_3D ( 'NONE', #74471, #84928, #105210 ) ;
#95776 = ORIENTED_EDGE ( 'NONE', *, *, #49902, .F. ) ;
#95777 = AXIS2_PLACEMENT_3D ( 'NONE', #69591, #47386, #49338 ) ;
#95778 = DIRECTION ( 'NONE',  ( 0.000000000000000000, 0.000000000000000000, 1.000000000000000000 ) ) ;
#95779 = DIRECTION ( 'NONE',  ( 0.000000000000000000, 0.000000000000000000, -1.000000000000000000 ) ) ;
#95780 = EDGE_CURVE ( 'NONE', #6261, #39515, #115882, .T. ) ;
#95781 = ORIENTED_EDGE ( 'NONE', *, *, #2863, .F. ) ;
#95782 = CONICAL_SURFACE ( 'NONE', #26737, 0.09999999999999982514, 0.003490658503988666988 ) ;
#95783 = FACE_OUTER_BOUND ( 'NONE', #52698, .T. ) ;
#95784 = DIRECTION ( 'NONE',  ( 0.000000000000000000, -0.000000000000000000, 1.000000000000000000 ) ) ;
#95785 = VECTOR ( 'NONE', #10815, 1000.000000000000000 ) ;
#95786 = VERTEX_POINT ( 'NONE', #87892 ) ;
#95787 = FACE_OUTER_BOUND ( 'NONE', #116657, .T. ) ;
#95788 = CARTESIAN_POINT ( 'NONE',  ( -4.400000000000025224, 2.500000000000000000, 4.676537180435972552 ) ) ;
#95789 = AXIS2_PLACEMENT_3D ( 'NONE', #68859, #108777, #29582 ) ;
#95790 = DIRECTION ( 'NONE',  ( -0.000000000000000000, 1.000000000000000000, -0.000000000000000000 ) ) ;
#95791 = PLANE ( 'NONE',  #13193 ) ;
#95792 = DIRECTION ( 'NONE',  ( 0.000000000000000000, -0.000000000000000000, 1.000000000000000000 ) ) ;
#95793 = AXIS2_PLACEMENT_3D ( 'NONE', #96939, #84552, #27541 ) ;
#95794 = DIRECTION ( 'NONE',  ( 0.000000000000000000, 0.000000000000000000, 1.000000000000000000 ) ) ;
#95795 = EDGE_LOOP ( 'NONE', ( #100040, #54941 ) ) ;
#95796 = ORIENTED_EDGE ( 'NONE', *, *, #96084, .T. ) ;
#95797 = ORIENTED_EDGE ( 'NONE', *, *, #30403, .T. ) ;
#95798 = ORIENTED_EDGE ( 'NONE', *, *, #82567, .F. ) ;
#95799 = CARTESIAN_POINT ( 'NONE',  ( 32.25969448929755856, 3.190781364619325267, 3.146220011503479075 ) ) ;
#95800 = DIRECTION ( 'NONE',  ( 0.000000000000000000, 0.000000000000000000, 1.000000000000000000 ) ) ;
#95801 = CARTESIAN_POINT ( 'NONE',  ( 8.349999999999923261, 2.500000000000000000, 2.165063509461097713 ) ) ;
#95802 = VERTEX_POINT ( 'NONE', #127836 ) ;
#95803 = FACE_BOUND ( 'NONE', #12012, .T. ) ;
#95804 = FACE_OUTER_BOUND ( 'NONE', #103431, .T. ) ;
#95805 = DIRECTION ( 'NONE',  ( 0.000000000000000000, 0.000000000000000000, 1.000000000000000000 ) ) ;
#95807 = EDGE_CURVE ( 'NONE', #40951, #34456, #19846, .T. ) ;
#95806 = CARTESIAN_POINT ( 'NONE',  ( 10.19999999999991402, 12.50000000000000000, 0.3464101615137735735 ) ) ;
#95809 = CIRCLE ( 'NONE', #72834, 0.06509327318403745899 ) ;
#95808 = CIRCLE ( 'NONE', #39404, 0.09999999999999982514 ) ;
#95810 = DIRECTION ( 'NONE',  ( 0.000000000000000000, 0.000000000000000000, -1.000000000000000000 ) ) ;
#95811 = DIRECTION ( 'NONE',  ( 0.000000000000000000, 0.000000000000000000, -1.000000000000000000 ) ) ;
#95812 = DIRECTION ( 'NONE',  ( 0.000000000000000000, -0.9999939076577903929, 0.003490651415223739937 ) ) ;
#95813 = DIRECTION ( 'NONE',  ( -0.000000000000000000, 1.000000000000000000, -0.000000000000000000 ) ) ;
#95814 = DIRECTION ( 'NONE',  ( 0.000000000000000000, 0.000000000000000000, 1.000000000000000000 ) ) ;
#95815 = EDGE_CURVE ( 'NONE', #55120, #99646, #9463, .T. ) ;
#95816 = EDGE_CURVE ( 'NONE', #4150, #46427, #105614, .T. ) ;
#95817 = DIRECTION ( 'NONE',  ( -0.000000000000000000, 1.000000000000000000, -0.000000000000000000 ) ) ;
#95818 = EDGE_CURVE ( 'NONE', #117477, #96527, #82637, .T. ) ;
#95819 = ADVANCED_FACE ( 'NONE', ( #116718 ), #30322, .T. ) ;
#95820 = DIRECTION ( 'NONE',  ( -0.000000000000000000, -1.000000000000000000, -0.000000000000000000 ) ) ;
#95821 = ORIENTED_EDGE ( 'NONE', *, *, #120822, .F. ) ;
#95822 = VERTEX_POINT ( 'NONE', #55868 ) ;
#95823 = EDGE_LOOP ( 'NONE', ( #18025, #25098 ) ) ;
#95824 = VERTEX_POINT ( 'NONE', #85960 ) ;
#95825 = DIRECTION ( 'NONE',  ( 0.000000000000000000, 0.000000000000000000, 1.000000000000000000 ) ) ;
#95826 = ADVANCED_FACE ( 'NONE', ( #7403 ), #78442, .T. ) ;
#95827 = VERTEX_POINT ( 'NONE', #46704 ) ;
#95828 = AXIS2_PLACEMENT_3D ( 'NONE', #20449, #99660, #11907 ) ;
#95829 = CARTESIAN_POINT ( 'NONE',  ( 16.56576425165006583, 1.500000000000000888, -6.084390597445814564 ) ) ;
#95831 = VERTEX_POINT ( 'NONE', #86618 ) ;
#95830 = EDGE_CURVE ( 'NONE', #112983, #6303, #45425, .T. ) ;
#95832 = ORIENTED_EDGE ( 'NONE', *, *, #5116, .F. ) ;
#95833 = DIRECTION ( 'NONE',  ( 0.000000000000000000, 0.000000000000000000, 1.000000000000000000 ) ) ;
#95834 = CIRCLE ( 'NONE', #79404, 0.06509327318403745899 ) ;
#95835 = EDGE_CURVE ( 'NONE', #49008, #99284, #47036, .T. ) ;
#95836 = CONICAL_SURFACE ( 'NONE', #91909, 0.09999999999999982514, 0.003490658503988666988 ) ;
#95837 = CARTESIAN_POINT ( 'NONE',  ( 10.89704209861766770, -2.500000000000253131, 8.980393935570946340 ) ) ;
#95839 = CARTESIAN_POINT ( 'NONE',  ( 4.349999999999937472, 12.50000000000000000, 6.906693963081109722 ) ) ;
#95838 = CIRCLE ( 'NONE', #127241, 0.06509327318403745899 ) ;
#95840 = DIRECTION ( 'NONE',  ( 0.000000000000000000, -0.000000000000000000, 1.000000000000000000 ) ) ;
#95841 = DIRECTION ( 'NONE',  ( -0.000000000000000000, 1.000000000000000000, -0.000000000000000000 ) ) ;
#95842 = EDGE_CURVE ( 'NONE', #2195, #51573, #125887, .T. ) ;
#95843 = ORIENTED_EDGE ( 'NONE', *, *, #76457, .T. ) ;
#95844 = ADVANCED_FACE ( 'NONE', ( #18525 ), #95162, .T. ) ;
#95845 = AXIS2_PLACEMENT_3D ( 'NONE', #25627, #6604, #127078 ) ;
#95846 = AXIS2_PLACEMENT_3D ( 'NONE', #30836, #91664, #92302 ) ;
#95847 = ORIENTED_EDGE ( 'NONE', *, *, #5892, .F. ) ;
#95848 = VECTOR ( 'NONE', #31317, 1000.000000000000000 ) ;
#95849 = ORIENTED_EDGE ( 'NONE', *, *, #11406, .T. ) ;
#95850 = ORIENTED_EDGE ( 'NONE', *, *, #71143, .F. ) ;
#95851 = PLANE ( 'NONE',  #63002 ) ;
#95852 = ORIENTED_EDGE ( 'NONE', *, *, #26333, .T. ) ;
#95853 = EDGE_LOOP ( 'NONE', ( #67027, #37582 ) ) ;
#95854 = AXIS2_PLACEMENT_3D ( 'NONE', #48937, #48282, #107188 ) ;
#95855 = FACE_OUTER_BOUND ( 'NONE', #84113, .T. ) ;
#95856 = CIRCLE ( 'NONE', #56127, 0.1000000000000002554 ) ;
#95857 = CARTESIAN_POINT ( 'NONE',  ( -3.100000000000028511, 2.500000000000000000, -0.2464101615137782308 ) ) ;
#95858 = DIRECTION ( 'NONE',  ( 0.000000000000000000, -0.9999939076577903929, 0.003490651415223739937 ) ) ;
#95859 = DIRECTION ( 'NONE',  ( 0.000000000000000000, -1.000000000000000000, 0.000000000000000000 ) ) ;
#95860 = FACE_OUTER_BOUND ( 'NONE', #72767, .T. ) ;
#95861 = CARTESIAN_POINT ( 'NONE',  ( 0.8499999999999553468, 2.500000000000000000, 2.265063509461097357 ) ) ;
#95862 = ORIENTED_EDGE ( 'NONE', *, *, #88459, .T. ) ;
#95863 = DIRECTION ( 'NONE',  ( 0.000000000000000000, 1.000000000000000000, 0.000000000000000000 ) ) ;
#95864 = AXIS2_PLACEMENT_3D ( 'NONE', #55892, #95185, #55264 ) ;
#95865 = ORIENTED_EDGE ( 'NONE', *, *, #8946, .T. ) ;
#95866 = DIRECTION ( 'NONE',  ( 0.000000000000000000, 0.000000000000000000, 1.000000000000000000 ) ) ;
#95867 = ORIENTED_EDGE ( 'NONE', *, *, #19772, .T. ) ;
#95868 = CARTESIAN_POINT ( 'NONE',  ( 10.19999999999991047, 2.500000000000000000, -3.983716857408426293 ) ) ;
#95869 = DIRECTION ( 'NONE',  ( 0.000000000000000000, 0.000000000000000000, 1.000000000000000000 ) ) ;
#95870 = CONICAL_SURFACE ( 'NONE', #28976, 0.1000000000000002554, 0.003490658503988666988 ) ;
#95871 = AXIS2_PLACEMENT_3D ( 'NONE', #79944, #40035, #22335 ) ;
#95872 = EDGE_LOOP ( 'NONE', ( #127769, #40947 ) ) ;
#95873 = CARTESIAN_POINT ( 'NONE',  ( -10.85000000000000142, 12.50000000000000000, -1.472243186433546125 ) ) ;
#95874 = CARTESIAN_POINT ( 'NONE',  ( 1.049999999999952971, 12.50000000000000000, 6.083687093685483660 ) ) ;
#95875 = EDGE_LOOP ( 'NONE', ( #112682, #94023 ) ) ;
#95876 = FILL_AREA_STYLE ('',( #34397 ) ) ;
#95877 = EDGE_CURVE ( 'NONE', #29719, #10941, #53299, .T. ) ;
#95878 = MECHANICAL_DESIGN_GEOMETRIC_PRESENTATION_REPRESENTATION (  '', ( #91668 ), #123068 ) ;
#95879 = CARTESIAN_POINT ( 'NONE',  ( 4.549999999999939426, 2.500000000000000000, -2.165063509461101710 ) ) ;
#95880 = EDGE_CURVE ( 'NONE', #64833, #124839, #26192, .T. ) ;
#95881 = ORIENTED_EDGE ( 'NONE', *, *, #54810, .F. ) ;
#95882 = ORIENTED_EDGE ( 'NONE', *, *, #48531, .F. ) ;
#95883 = DIRECTION ( 'NONE',  ( -1.000000000000000000, -0.000000000000000000, -0.000000000000000000 ) ) ;
#95884 = CARTESIAN_POINT ( 'NONE',  ( 97.50000000000000000, 0.000000000000000000, 0.000000000000000000 ) ) ;
#95885 = CARTESIAN_POINT ( 'NONE',  ( 186.7552083336747444, 6.551208109652275624, -3.782341765624998686 ) ) ;
#95887 = AXIS2_PLACEMENT_3D ( 'NONE', #39697, #31155, #111631 ) ;
#95886 = DIRECTION ( 'NONE',  ( -0.000000000000000000, -1.000000000000000000, -0.000000000000000000 ) ) ;
#95888 = VECTOR ( 'NONE', #59572, 1000.000000000000000 ) ;
#95889 = DIRECTION ( 'NONE',  ( -0.000000000000000000, -1.000000000000000000, -0.000000000000000000 ) ) ;
#95890 = DIRECTION ( 'NONE',  ( 0.000000000000000000, 0.000000000000000000, 1.000000000000000000 ) ) ;
#95891 = CIRCLE ( 'NONE', #37321, 2.250000000000001776 ) ;
#95892 = ORIENTED_EDGE ( 'NONE', *, *, #122340, .T. ) ;
#95893 = LINE ( 'NONE', #115507, #31830 ) ;
#95894 = ORIENTED_EDGE ( 'NONE', *, *, #24897, .F. ) ;
#95895 = AXIS2_PLACEMENT_3D ( 'NONE', #124423, #95605, #43298 ) ;
#95896 = AXIS2_PLACEMENT_3D ( 'NONE', #42362, #71163, #80989 ) ;
#95897 = CARTESIAN_POINT ( 'NONE',  ( -10.45000000000000462, 2.500000000000000000, -2.165063509461097713 ) ) ;
#95898 = CARTESIAN_POINT ( 'NONE',  ( -0.6500000000000403233, 2.500000000000000000, 6.248780366869520542 ) ) ;
#95899 = DIRECTION ( 'NONE',  ( 0.000000000000000000, 1.000000000000000000, 0.000000000000000000 ) ) ;
#95900 = ORIENTED_EDGE ( 'NONE', *, *, #1792, .T. ) ;
#95901 = AXIS2_PLACEMENT_3D ( 'NONE', #54570, #4824, #84689 ) ;
#95902 = CARTESIAN_POINT ( 'NONE',  ( 3.099999999999945466, 2.500000000000000000, 0.3464101615137735735 ) ) ;
#95903 = DIRECTION ( 'NONE',  ( -0.000000000000000000, -1.000000000000000000, -0.000000000000000000 ) ) ;
#95904 = ORIENTED_EDGE ( 'NONE', *, *, #29468, .T. ) ;
#95905 = CARTESIAN_POINT ( 'NONE',  ( -11.24999999999999822, 12.50000000000000000, 1.537336459617582918 ) ) ;
#95906 = EDGE_CURVE ( 'NONE', #87583, #23954, #95145, .T. ) ;
#95907 = VERTEX_POINT ( 'NONE', #61026 ) ;
#95908 = ORIENTED_EDGE ( 'NONE', *, *, #21344, .T. ) ;
#95909 = CARTESIAN_POINT ( 'NONE',  ( 184.5000000000000000, 0.000000000000000000, 0.000000000000000000 ) ) ;
#95910 = AXIS2_PLACEMENT_3D ( 'NONE', #84366, #35285, #63443 ) ;
#95911 = ORIENTED_EDGE ( 'NONE', *, *, #115264, .F. ) ;
#95912 = DIRECTION ( 'NONE',  ( 0.000000000000000000, 1.000000000000000000, 0.000000000000000000 ) ) ;
#95913 = CARTESIAN_POINT ( 'NONE',  ( 179.5000000000000000, -0.6250000000000028866, -7.634788798650553154 ) ) ;
#95914 = DIRECTION ( 'NONE',  ( 0.000000000000000000, -0.000000000000000000, 1.000000000000000000 ) ) ;
#95915 = EDGE_CURVE ( 'NONE', #29584, #32403, #86727, .T. ) ;
#95916 = ORIENTED_EDGE ( 'NONE', *, *, #77026, .F. ) ;
#95917 = CONICAL_SURFACE ( 'NONE', #64516, 0.1000000000000002554, 0.003490658503988666988 ) ;
#95918 = FACE_BOUND ( 'NONE', #31571, .T. ) ;
#95919 = AXIS2_PLACEMENT_3D ( 'NONE', #31026, #108892, #30372 ) ;
#95921 = ORIENTED_EDGE ( 'NONE', *, *, #54881, .T. ) ;
#95920 = FACE_OUTER_BOUND ( 'NONE', #54223, .T. ) ;
#95922 = EDGE_CURVE ( 'NONE', #112250, #84669, #103464, .T. ) ;
#95923 = CARTESIAN_POINT ( 'NONE',  ( 3.949999999999942446, 12.50000000000000000, -6.841600689897078702 ) ) ;
#95924 = FACE_OUTER_BOUND ( 'NONE', #101821, .T. ) ;
#95925 = EDGE_CURVE ( 'NONE', #29739, #118702, #124396, .T. ) ;
#95926 = AXIS2_PLACEMENT_3D ( 'NONE', #35683, #106348, #48084 ) ;
#95927 = VERTEX_POINT ( 'NONE', #49949 ) ;
#95928 = AXIS2_PLACEMENT_3D ( 'NONE', #46422, #48363, #7132 ) ;
#95929 = AXIS2_PLACEMENT_3D ( 'NONE', #18738, #58675, #8904 ) ;
#95930 = ORIENTED_EDGE ( 'NONE', *, *, #50141, .F. ) ;
#95931 = VERTEX_POINT ( 'NONE', #39489 ) ;
#95932 = DIRECTION ( 'NONE',  ( 0.000000000000000000, 1.000000000000000000, 0.000000000000000000 ) ) ;
#95933 = DIRECTION ( 'NONE',  ( 0.000000000000000000, -0.000000000000000000, 1.000000000000000000 ) ) ;
#95934 = DIRECTION ( 'NONE',  ( 0.000000000000000000, 1.000000000000000000, 0.000000000000000000 ) ) ;
#95935 = EDGE_CURVE ( 'NONE', #117161, #98934, #22008, .T. ) ;
#95936 = FACE_BOUND ( 'NONE', #59741, .T. ) ;
#95937 = VERTEX_POINT ( 'NONE', #118654 ) ;
#95938 = CARTESIAN_POINT ( 'NONE',  ( 186.1927083336747160, 6.551208109652275624, -3.782341765624998686 ) ) ;
#95939 = CONICAL_SURFACE ( 'NONE', #8105, 0.1000000000000002554, 0.003490658503988666988 ) ;
#95940 = DIRECTION ( 'NONE',  ( 0.000000000000000000, 0.000000000000000000, 1.000000000000000000 ) ) ;
#95941 = FACE_OUTER_BOUND ( 'NONE', #10934, .T. ) ;
#95942 = CARTESIAN_POINT ( 'NONE',  ( 12.49999999999990585, 12.50000000000000000, -5.022947341949754119 ) ) ;
#95943 = CARTESIAN_POINT ( 'NONE',  ( -0.8500000000000395017, 12.50000000000000000, 2.230156782645134950 ) ) ;
#95944 = DIRECTION ( 'NONE',  ( 0.000000000000000000, -0.000000000000000000, 1.000000000000000000 ) ) ;
#95945 = CARTESIAN_POINT ( 'NONE',  ( -6.250000000000015987, 2.500000000000000000, 1.472243186433545459 ) ) ;
#95946 = DIRECTION ( 'NONE',  ( -0.000000000000000000, 1.000000000000000000, -0.000000000000000000 ) ) ;
#95947 = VECTOR ( 'NONE', #845, 1000.000000000000000 ) ;
#95948 = FACE_OUTER_BOUND ( 'NONE', #119958, .T. ) ;
#95949 = EDGE_LOOP ( 'NONE', ( #65199, #112918 ) ) ;
#95950 = ORIENTED_EDGE ( 'NONE', *, *, #35766, .T. ) ;
#95951 = ORIENTED_EDGE ( 'NONE', *, *, #48756, .T. ) ;
#95952 = ORIENTED_EDGE ( 'NONE', *, *, #8188, .F. ) ;
#95953 = ORIENTED_EDGE ( 'NONE', *, *, #78265, .F. ) ;
#95954 = CONICAL_SURFACE ( 'NONE', #72881, 0.1000000000000000472, 0.003490658503988666988 ) ;
#95955 = CARTESIAN_POINT ( 'NONE',  ( -11.64999999999999680, 12.50000000000000000, -2.165063509461097713 ) ) ;
#95956 = DIRECTION ( 'NONE',  ( -0.000000000000000000, -1.000000000000000000, -0.000000000000000000 ) ) ;
#95957 = EDGE_LOOP ( 'NONE', ( #85243, #15101 ) ) ;
#95958 = FACE_BOUND ( 'NONE', #115533, .T. ) ;
#95959 = CARTESIAN_POINT ( 'NONE',  ( 0.3999999999999563904, 2.500000000000000000, 5.022947341949748790 ) ) ;
#95960 = EDGE_CURVE ( 'NONE', #86833, #106745, #91138, .T. ) ;
#95961 = AXIS2_PLACEMENT_3D ( 'NONE', #70441, #17449, #10233 ) ;
#95962 = DIRECTION ( 'NONE',  ( -0.000000000000000000, -1.000000000000000000, -0.000000000000000000 ) ) ;
#95963 = LINE ( 'NONE', #16730, #126821 ) ;
#95964 = DIRECTION ( 'NONE',  ( 0.000000000000000000, 0.000000000000000000, -1.000000000000000000 ) ) ;
#95965 = EDGE_CURVE ( 'NONE', #91963, #101677, #120195, .T. ) ;
#95966 = DIRECTION ( 'NONE',  ( -0.000000000000000000, -1.000000000000000000, -0.000000000000000000 ) ) ;
#95967 = ORIENTED_EDGE ( 'NONE', *, *, #17145, .F. ) ;
#95968 = VECTOR ( 'NONE', #117394, 1000.000000000000000 ) ;
#95969 = CARTESIAN_POINT ( 'NONE',  ( 184.5000000000000000, 0.000000000000000000, -7.699999999999999289 ) ) ;
#95970 = EDGE_CURVE ( 'NONE', #110892, #120440, #41411, .T. ) ;
#95972 = ORIENTED_EDGE ( 'NONE', *, *, #96119, .F. ) ;
#95971 = CONICAL_SURFACE ( 'NONE', #39574, 0.1000000000000002554, 0.003490658503988666988 ) ;
#95973 = ORIENTED_EDGE ( 'NONE', *, *, #17769, .T. ) ;
#95974 = EDGE_LOOP ( 'NONE', ( #128915, #6232 ) ) ;
#95975 = EDGE_CURVE ( 'NONE', #24259, #69008, #17770, .T. ) ;
#95976 = LINE ( 'NONE', #62351, #109087 ) ;
#95978 = ADVANCED_FACE ( 'NONE', ( #99681 ), #100319, .T. ) ;
#95977 = CARTESIAN_POINT ( 'NONE',  ( 3.149999999999944400, 2.500000000000000000, 2.611473670974873151 ) ) ;
#95979 = FACE_OUTER_BOUND ( 'NONE', #54055, .T. ) ;
#95980 = AXIS2_PLACEMENT_3D ( 'NONE', #101798, #80869, #122083 ) ;
#95982 = EDGE_LOOP ( 'NONE', ( #85118, #92758 ) ) ;
#95981 = ADVANCED_FACE ( 'NONE', ( #21100 ), #111875, .T. ) ;
#95983 = CARTESIAN_POINT ( 'NONE',  ( 13.80955901367088146, 1.499999999999681366, -7.955427458311461031 ) ) ;
#95984 = ADVANCED_FACE ( 'NONE', ( #80028 ), #819, .T. ) ;
#95985 = CARTESIAN_POINT ( 'NONE',  ( 3.299999999999944755, 2.500000000000000000, -0.1000000000000023925 ) ) ;
#95989 = EDGE_CURVE ( 'NONE', #11815, #109349, #128622, .T. ) ;
#95988 = VECTOR ( 'NONE', #4459, 1000.000000000000000 ) ;
#95987 = CARTESIAN_POINT ( 'NONE',  ( -6.450000000000016165, 12.50000000000000000, 6.841600689897072485 ) ) ;
#95986 = CIRCLE ( 'NONE', #87561, 0.06509327318403745899 ) ;
#95990 = CARTESIAN_POINT ( 'NONE',  ( 186.7760416670080588, 6.551208109652274736, 3.782341765625001351 ) ) ;
#95991 = CARTESIAN_POINT ( 'NONE',  ( -5.650000000000019895, 12.50000000000000000, 6.148780366869520009 ) ) ;
#95992 = AXIS2_PLACEMENT_3D ( 'NONE', #60572, #41577, #101768 ) ;
#95993 = DIRECTION ( 'NONE',  ( 0.000000000000000000, 0.000000000000000000, 1.000000000000000000 ) ) ;
#95994 = EDGE_LOOP ( 'NONE', ( #125140, #49722, #120362, #35748 ) ) ;
#95995 = DIRECTION ( 'NONE',  ( -0.000000000000000000, -1.000000000000000000, -0.000000000000000000 ) ) ;
#95996 = EDGE_CURVE ( 'NONE', #102123, #56648, #122348, .T. ) ;
#95998 = CONICAL_SURFACE ( 'NONE', #100206, 0.1000000000000000472, 0.003490658503988666988 ) ;
#95997 = CONICAL_SURFACE ( 'NONE', #16547, 0.1000000000000000472, 0.003490658503988666988 ) ;
#95999 = ORIENTED_EDGE ( 'NONE', *, *, #5613, .T. ) ;
#96000 = ORIENTED_EDGE ( 'NONE', *, *, #65350, .F. ) ;
#96001 = LINE ( 'NONE', #25299, #63451 ) ;
#96002 = DIRECTION ( 'NONE',  ( 0.000000000000000000, 1.000000000000000000, 0.000000000000000000 ) ) ;
#96003 = DIRECTION ( 'NONE',  ( 0.000000000000000000, 0.000000000000000000, -1.000000000000000000 ) ) ;
#96004 = ORIENTED_EDGE ( 'NONE', *, *, #16163, .T. ) ;
#96005 = ORIENTED_EDGE ( 'NONE', *, *, #109585, .T. ) ;
#96006 = CARTESIAN_POINT ( 'NONE',  ( -10.84999999999999964, 2.500000000000000000, 1.472243186433545459 ) ) ;
#96007 = LINE ( 'NONE', #7613, #122637 ) ;
#96008 = LINE ( 'NONE', #114985, #69057 ) ;
#96010 = ORIENTED_EDGE ( 'NONE', *, *, #102587, .F. ) ;
#96009 = VECTOR ( 'NONE', #115412, 1000.000000000000000 ) ;
#96011 = ORIENTED_EDGE ( 'NONE', *, *, #105846, .F. ) ;
#96012 = LINE ( 'NONE', #84898, #33150 ) ;
#96013 = ORIENTED_EDGE ( 'NONE', *, *, #50915, .F. ) ;
#96014 = CARTESIAN_POINT ( 'NONE',  ( 11.04999999999991189, 2.500000000000000000, 6.148780366869520897 ) ) ;
#96015 = CONICAL_SURFACE ( 'NONE', #81364, 0.09999999999999982514, 0.003490658503988666988 ) ;
#96016 = CARTESIAN_POINT ( 'NONE',  ( -13.34999999999999076, 12.50000000000000000, -1.537336459617585360 ) ) ;
#96017 = VERTEX_POINT ( 'NONE', #129158 ) ;
#96018 = CARTESIAN_POINT ( 'NONE',  ( -10.20000000000000462, 12.50000000000000000, 0.2813168883297361700 ) ) ;
#96019 = CARTESIAN_POINT ( 'NONE',  ( 13.09999999999990195, 2.500000000000000000, 4.676537180435972552 ) ) ;
#96020 = DIRECTION ( 'NONE',  ( 0.000000000000000000, -0.9999939076577903929, 0.003490651415223739937 ) ) ;
#96021 = FACE_OUTER_BOUND ( 'NONE', #32751, .T. ) ;
#96022 = ORIENTED_EDGE ( 'NONE', *, *, #32603, .F. ) ;
#96023 = CONICAL_SURFACE ( 'NONE', #20810, 0.1000000000000000472, 0.003490658503988666988 ) ;
#96024 = FACE_OUTER_BOUND ( 'NONE', #14166, .T. ) ;
#96025 = EDGE_CURVE ( 'NONE', #97422, #108453, #44982, .T. ) ;
#96026 = CARTESIAN_POINT ( 'NONE',  ( 1.049999999999954525, 2.500000000000000000, -2.511473670974877948 ) ) ;
#96027 = ORIENTED_EDGE ( 'NONE', *, *, #91953, .T. ) ;
#96028 = ORIENTED_EDGE ( 'NONE', *, *, #122922, .F. ) ;
#96029 = DIRECTION ( 'NONE',  ( 0.000000000000000000, 0.000000000000000000, 1.000000000000000000 ) ) ;
#96030 = CARTESIAN_POINT ( 'NONE',  ( -14.79999999999998295, 12.50000000000000000, -0.2813168883297386680 ) ) ;
#96031 = DIRECTION ( 'NONE',  ( 0.000000000000000000, 1.000000000000000000, 0.000000000000000000 ) ) ;
#96032 = CARTESIAN_POINT ( 'NONE',  ( 5.849999999999933031, 2.500000000000000000, 7.188010851410848723 ) ) ;
#96033 = DIRECTION ( 'NONE',  ( 0.000000000000000000, 0.000000000000000000, -1.000000000000000000 ) ) ;
#96034 = DIRECTION ( 'NONE',  ( 0.000000000000000000, 1.000000000000000000, 0.000000000000000000 ) ) ;
#96035 = EDGE_CURVE ( 'NONE', #89842, #44383, #113930, .T. ) ;
#96036 = AXIS2_PLACEMENT_3D ( 'NONE', #79488, #90575, #100408 ) ;
#96037 = AXIS2_PLACEMENT_3D ( 'NONE', #98323, #129116, #8644 ) ;
#96038 = CARTESIAN_POINT ( 'NONE',  ( -2.700000000000030820, 12.50000000000000000, 0.4115034346978109769 ) ) ;
#96039 = FACE_OUTER_BOUND ( 'NONE', #96101, .T. ) ;
#96040 = CARTESIAN_POINT ( 'NONE',  ( -1.650000000000035216, 2.500000000000000000, -5.802370205355749988 ) ) ;
#96041 = CARTESIAN_POINT ( 'NONE',  ( 13.34999999999989662, 2.500000000000000000, -2.165063509461101710 ) ) ;
#96042 = ORIENTED_EDGE ( 'NONE', *, *, #24860, .F. ) ;
#96043 = ORIENTED_EDGE ( 'NONE', *, *, #84283, .F. ) ;
#96044 = CARTESIAN_POINT ( 'NONE',  ( -15.39999999999997904, 2.500000000000000000, -0.5928203230275518321 ) ) ;
#96045 = EDGE_LOOP ( 'NONE', ( #35770, #120380, #61798, #43468 ) ) ;
#96046 = CARTESIAN_POINT ( 'NONE',  ( 10.39999999999991154, 12.50000000000000000, 5.088040615133786027 ) ) ;
#96047 = DIRECTION ( 'NONE',  ( 0.000000000000000000, 0.000000000000000000, 1.000000000000000000 ) ) ;
#96048 = DIRECTION ( 'NONE',  ( -0.000000000000000000, -1.000000000000000000, -0.000000000000000000 ) ) ;
#96049 = VERTEX_POINT ( 'NONE', #59773 ) ;
#96050 = CARTESIAN_POINT ( 'NONE',  ( 17.79089025268834590, -2.511997385349132195, -2.795007471442499725 ) ) ;
#96051 = CARTESIAN_POINT ( 'NONE',  ( 6.049999999999932321, 2.500000000000000000, 1.918653347947321564 ) ) ;
#96053 = VERTEX_POINT ( 'NONE', #74073 ) ;
#96052 = CARTESIAN_POINT ( 'NONE',  ( 12.04999999999990834, 2.500000000000000000, -2.065063509461102065 ) ) ;
#96054 =( BOUNDED_CURVE ( )  B_SPLINE_CURVE ( 2, ( #110203, #72854, #13270, #53224, #3467, #123246, #35516 ),
 .UNSPECIFIED., .F., .F. ) 
 B_SPLINE_CURVE_WITH_KNOTS ( ( 3, 2, 2, 3 ),
 ( 0.7142857142857148567, 0.7380952380952386926, 0.7619047619047624176, 0.7857142857142862535 ),
 .UNSPECIFIED. ) 
 CURVE ( )  GEOMETRIC_REPRESENTATION_ITEM ( )  RATIONAL_B_SPLINE_CURVE ( ( 0.9999999999999968914, 0.8660254037844418162, 1.000000000000000000, 0.8660254037844387076, 1.000000000000000000, 0.8660254037844355990, 1.000000000000003109 ) ) 
 REPRESENTATION_ITEM ( '' )  );
#96055 = VECTOR ( 'NONE', #66871, 1000.000000000000000 ) ;
#96056 = CARTESIAN_POINT ( 'NONE',  ( -1.450000000000036371, 12.50000000000000000, 6.906693963081109722 ) ) ;
#96057 = EDGE_LOOP ( 'NONE', ( #74567, #127396 ) ) ;
#96058 = EDGE_CURVE ( 'NONE', #61588, #45891, #84535, .T. ) ;
#96059 = EDGE_LOOP ( 'NONE', ( #123876, #60392, #13644, #110006 ) ) ;
#96060 = VERTEX_POINT ( 'NONE', #42044 ) ;
#96061 = EDGE_LOOP ( 'NONE', ( #52851, #60053, #14135, #11925 ) ) ;
#96062 = CARTESIAN_POINT ( 'NONE',  ( -11.24999999999996447, 2.500000000000000000, -6.595190528383298556 ) ) ;
#96063 = CIRCLE ( 'NONE', #110645, 0.06509327318403745899 ) ;
#96064 = DIRECTION ( 'NONE',  ( -0.000000000000000000, 1.000000000000000000, -0.000000000000000000 ) ) ;
#96065 = CARTESIAN_POINT ( 'NONE',  ( 130.5000000000000000, -0.5000000000000000000, -7.500000000000001776 ) ) ;
#96066 = CARTESIAN_POINT ( 'NONE',  ( -9.350000000000004974, 12.50000000000000000, 6.841600689897072485 ) ) ;
#96067 = ADVANCED_FACE ( 'NONE', ( #62333 ), #123184, .T. ) ;
#96068 = EDGE_LOOP ( 'NONE', ( #36567, #100322 ) ) ;
#96070 = VECTOR ( 'NONE', #449, 1000.000000000000000 ) ;
#96069 = CIRCLE ( 'NONE', #27033, 0.1000000000000002554 ) ;
#96071 = CARTESIAN_POINT ( 'NONE',  ( -6.650000000000018119, 12.50000000000000000, -6.495190528383302464 ) ) ;
#96072 = VERTEX_POINT ( 'NONE', #33520 ) ;
#96073 = DIRECTION ( 'NONE',  ( 0.000000000000000000, 0.000000000000000000, -1.000000000000000000 ) ) ;
#96075 = VECTOR ( 'NONE', #78110, 1000.000000000000000 ) ;
#96074 = DIRECTION ( 'NONE',  ( 0.000000000000000000, 0.000000000000000000, -1.000000000000000000 ) ) ;
#96076 = EDGE_CURVE ( 'NONE', #124065, #68389, #118118, .T. ) ;
#96077 = CARTESIAN_POINT ( 'NONE',  ( -10.20000000000000462, 2.500000000000000000, 4.576537180435972019 ) ) ;
#96078 = CARTESIAN_POINT ( 'NONE',  ( 18.37149739119674052, -2.540880845002044808, 2.596776292461127067 ) ) ;
#96079 = EDGE_CURVE ( 'NONE', #9068, #29188, #65887, .T. ) ;
#96080 = ORIENTED_EDGE ( 'NONE', *, *, #112266, .F. ) ;
#96082 = VECTOR ( 'NONE', #97207, 1000.000000000000000 ) ;
#96081 = PRESENTATION_LAYER_ASSIGNMENT (  '', '', ( #91884 ) ) ;
#96083 = ORIENTED_EDGE ( 'NONE', *, *, #117350, .F. ) ;
#96084 = EDGE_CURVE ( 'NONE', #111361, #105503, #88879, .T. ) ;
#96085 = ORIENTED_EDGE ( 'NONE', *, *, #107250, .T. ) ;
#96086 = DIRECTION ( 'NONE',  ( 0.000000000000000000, 0.000000000000000000, 1.000000000000000000 ) ) ;
#96087 = CARTESIAN_POINT ( 'NONE',  ( -8.750000000000010658, 2.500000000000000000, -1.572243186433550211 ) ) ;
#96088 = CARTESIAN_POINT ( 'NONE',  ( 7.099999999999925926, 12.50000000000000000, 0.7579135962115869374 ) ) ;
#96089 = ADVANCED_FACE ( 'NONE', ( #22419 ), #3118, .T. ) ;
#96090 = FACE_BOUND ( 'NONE', #87454, .T. ) ;
#96091 = CARTESIAN_POINT ( 'NONE',  ( 5.199999999999933564, 2.500000000000000000, 3.983716857408420076 ) ) ;
#96092 = DIRECTION ( 'NONE',  ( -0.000000000000000000, 1.000000000000000000, -0.000000000000000000 ) ) ;
#96093 = CARTESIAN_POINT ( 'NONE',  ( -3.470671598752761919E-14, 2.500000000000000000, -0.7928203230275518987 ) ) ;
#96094 = FACE_OUTER_BOUND ( 'NONE', #76415, .T. ) ;
#96095 = CARTESIAN_POINT ( 'NONE',  ( 184.8802083336747444, 4.367472073101515306, 7.564683531250000925 ) ) ;
#96096 = CARTESIAN_POINT ( 'NONE',  ( -11.44999999999999751, 2.500000000000000000, 1.818653347947321475 ) ) ;
#96097 = CARTESIAN_POINT ( 'NONE',  ( -12.89999999999999147, 12.50000000000000000, 4.395220292106234439 ) ) ;
#96098 = VECTOR ( 'NONE', #111275, 1000.000000000000000 ) ;
#96099 = AXIS2_PLACEMENT_3D ( 'NONE', #5712, #115670, #115022 ) ;
#96100 = FACE_OUTER_BOUND ( 'NONE', #8485, .T. ) ;
#96101 = EDGE_LOOP ( 'NONE', ( #70438, #118126 ) ) ;
#96102 = ORIENTED_EDGE ( 'NONE', *, *, #89631, .T. ) ;
#96103 = ORIENTED_EDGE ( 'NONE', *, *, #92242, .F. ) ;
#96104 = VERTEX_POINT ( 'NONE', #104175 ) ;
#96105 = LINE ( 'NONE', #94822, #21473 ) ;
#96106 = FACE_BOUND ( 'NONE', #74147, .T. ) ;
#96107 = DIRECTION ( 'NONE',  ( 0.000000000000000000, 0.000000000000000000, 1.000000000000000000 ) ) ;
#96109 = VECTOR ( 'NONE', #87777, 1000.000000000000000 ) ;
#96108 = VECTOR ( 'NONE', #87322, 1000.000000000000000 ) ;
#96110 = DIRECTION ( 'NONE',  ( 0.000000000000000000, 0.000000000000000000, 1.000000000000000000 ) ) ;
#96111 = EDGE_LOOP ( 'NONE', ( #45771, #122710 ) ) ;
#96112 = CARTESIAN_POINT ( 'NONE',  ( -12.29999999999999538, 2.500000000000000000, -0.4464101615137742174 ) ) ;
#96113 = CARTESIAN_POINT ( 'NONE',  ( 14.14999999999989733, 12.50000000000000000, 2.922977105672686982 ) ) ;
#96114 = ORIENTED_EDGE ( 'NONE', *, *, #65929, .F. ) ;
#96115 = DIRECTION ( 'NONE',  ( 0.000000000000000000, 0.000000000000000000, 1.000000000000000000 ) ) ;
#96116 = FACE_OUTER_BOUND ( 'NONE', #117357, .T. ) ;
#96117 = AXIS2_PLACEMENT_3D ( 'NONE', #37480, #64973, #65625 ) ;
#96118 = CONICAL_SURFACE ( 'NONE', #104534, 0.09999999999999999167, 0.003490658503988666988 ) ;
#96119 = EDGE_CURVE ( 'NONE', #9837, #66463, #59579, .T. ) ;
#96120 = ORIENTED_EDGE ( 'NONE', *, *, #79669, .F. ) ;
#96121 = EDGE_CURVE ( 'NONE', #104198, #25500, #128720, .T. ) ;
#96122 = FACE_OUTER_BOUND ( 'NONE', #122958, .T. ) ;
#96123 = DIRECTION ( 'NONE',  ( 0.000000000000000000, -0.000000000000000000, 1.000000000000000000 ) ) ;
#96124 = EDGE_CURVE ( 'NONE', #79633, #66106, #101504, .T. ) ;
#96126 = EDGE_CURVE ( 'NONE', #32665, #120157, #76461, .T. ) ;
#96125 = VECTOR ( 'NONE', #106063, 1000.000000000000000 ) ;
#96127 = VERTEX_POINT ( 'NONE', #81950 ) ;
#96128 = LINE ( 'NONE', #116404, #82324 ) ;
#96129 = CARTESIAN_POINT ( 'NONE',  ( -5.800000000000022027, 2.500000000000000000, -4.330127018922201643 ) ) ;
#96130 = EDGE_LOOP ( 'NONE', ( #122956, #55945 ) ) ;
#96132 = ADVANCED_FACE ( 'NONE', ( #21761 ), #38832, .T. ) ;
#96131 = LINE ( 'NONE', #96764, #72356 ) ;
#96133 = ORIENTED_EDGE ( 'NONE', *, *, #93035, .T. ) ;
#96134 = ORIENTED_EDGE ( 'NONE', *, *, #77824, .F. ) ;
#96135 = CARTESIAN_POINT ( 'NONE',  ( -2.950000000000033484, 12.50000000000000000, -6.495190528383302464 ) ) ;
#96136 = VERTEX_POINT ( 'NONE', #44615 ) ;
#96137 = DIRECTION ( 'NONE',  ( 0.000000000000000000, 1.000000000000000000, 0.000000000000000000 ) ) ;
#96138 = FACE_BOUND ( 'NONE', #91117, .T. ) ;
#96139 = EDGE_CURVE ( 'NONE', #26496, #60288, #126543, .T. ) ;
#96140 = EDGE_CURVE ( 'NONE', #1757, #72027, #34818, .T. ) ;
#96141 = EDGE_LOOP ( 'NONE', ( #70186, #65641 ) ) ;
#96142 = CARTESIAN_POINT ( 'NONE',  ( -10.40000000000000213, 2.500000000000000000, -0.6928203230275541413 ) ) ;
#96143 = CARTESIAN_POINT ( 'NONE',  ( -9.600000000000008527, 12.50000000000000000, -4.265033745738159965 ) ) ;
#96144 = DIRECTION ( 'NONE',  ( 0.000000000000000000, 0.000000000000000000, 1.000000000000000000 ) ) ;
#96145 = FACE_OUTER_BOUND ( 'NONE', #125563, .T. ) ;
#96146 = CARTESIAN_POINT ( 'NONE',  ( -2.100000000000033396, 12.50000000000000000, -0.6928203230275542523 ) ) ;
#96147 = DIRECTION ( 'NONE',  ( 0.000000000000000000, 0.000000000000000000, 1.000000000000000000 ) ) ;
#96148 = ORIENTED_EDGE ( 'NONE', *, *, #64793, .T. ) ;
#96149 = ORIENTED_EDGE ( 'NONE', *, *, #91412, .T. ) ;
#96150 = CARTESIAN_POINT ( 'NONE',  ( -1.850000000000033396, 2.500000000000000000, -2.511473670974877948 ) ) ;
#96151 = CARTESIAN_POINT ( 'NONE',  ( -6.050000000000017586, 2.500000000000000000, 1.818653347947321475 ) ) ;
#96152 = CARTESIAN_POINT ( 'NONE',  ( -1.650000000000034772, 2.500000000000000000, 2.265063509461097357 ) ) ;
#96154 = EDGE_LOOP ( 'NONE', ( #120841, #106250, #60405, #43309 ) ) ;
#96153 = ORIENTED_EDGE ( 'NONE', *, *, #122852, .F. ) ;
#96155 = ORIENTED_EDGE ( 'NONE', *, *, #119006, .T. ) ;
#96156 = CONICAL_SURFACE ( 'NONE', #108675, 0.1000000000000000472, 0.003490658503988666988 ) ;
#96157 = CARTESIAN_POINT ( 'NONE',  ( -14.34999999999998543, 2.500000000000000000, -2.411473670974875638 ) ) ;
#96158 = CARTESIAN_POINT ( 'NONE',  ( -4.350000000000023626, 2.500000000000000000, 6.148780366869520897 ) ) ;
#96159 = DIRECTION ( 'NONE',  ( 0.000000000000000000, -0.9999939076577903929, 0.003490651415223739937 ) ) ;
#96160 = AXIS2_PLACEMENT_3D ( 'NONE', #118756, #6206, #58565 ) ;
#96161 = PLANE ( 'NONE',  #64094 ) ;
#96162 = CARTESIAN_POINT ( 'NONE',  ( -6.850000000000017408, 2.500000000000000000, -6.941600689897077459 ) ) ;
#96163 = CARTESIAN_POINT ( 'NONE',  ( -14.79999999999998472, 2.500000000000000000, 0.2464101615137758439 ) ) ;
#96164 = CARTESIAN_POINT ( 'NONE',  ( -10.80000000000000071, 2.500000000000000000, -2.276824562219559311E-15 ) ) ;
#96165 = DIRECTION ( 'NONE',  ( 0.000000000000000000, 0.000000000000000000, 1.000000000000000000 ) ) ;
#96166 = LINE ( 'NONE', #29385, #18568 ) ;
#96167 = AXIS2_PLACEMENT_3D ( 'NONE', #39300, #87705, #18959 ) ;
#96168 = ORIENTED_EDGE ( 'NONE', *, *, #121294, .T. ) ;
#96169 = CARTESIAN_POINT ( 'NONE',  ( 8.149999999999920419, 12.50000000000000000, -2.576566944158915184 ) ) ;
#96170 = VERTEX_POINT ( 'NONE', #23044 ) ;
#96171 = ORIENTED_EDGE ( 'NONE', *, *, #98641, .T. ) ;
#96172 = CARTESIAN_POINT ( 'NONE',  ( -6.250000000000019540, 12.50000000000000000, -2.857883832488653741 ) ) ;
#96173 = CARTESIAN_POINT ( 'NONE',  ( 9.149999999999918643, 2.500000000000000000, 2.165063509461097713 ) ) ;
#96174 = CARTESIAN_POINT ( 'NONE',  ( -6.650000000000014566, 2.500000000000000000, 5.902370205355745192 ) ) ;
#96175 = LINE ( 'NONE', #45809, #117381 ) ;
#96176 = EDGE_CURVE ( 'NONE', #87768, #54395, #9560, .T. ) ;
#96177 = DIRECTION ( 'NONE',  ( 0.000000000000000000, 1.000000000000000000, 0.000000000000000000 ) ) ;
#96178 = DIRECTION ( 'NONE',  ( -0.000000000000000000, -1.000000000000000000, -0.000000000000000000 ) ) ;
#96179 = CARTESIAN_POINT ( 'NONE',  ( -12.89999999999999325, 2.500000000000000000, 0.5928203230275536084 ) ) ;
#96180 = VERTEX_POINT ( 'NONE', #83881 ) ;
#96181 = DIRECTION ( 'NONE',  ( 1.000000000000000000, 0.000000000000000000, 0.000000000000000000 ) ) ;
#96182 = DIRECTION ( 'NONE',  ( 0.000000000000000000, -0.9999939076577903929, 0.003490651415223739937 ) ) ;
#96183 = ORIENTED_EDGE ( 'NONE', *, *, #85309, .F. ) ;
#96184 = AXIS2_PLACEMENT_3D ( 'NONE', #5196, #64769, #54316 ) ;
#96186 = ORIENTED_EDGE ( 'NONE', *, *, #77795, .F. ) ;
#96185 = AXIS2_PLACEMENT_3D ( 'NONE', #106912, #68930, #18542 ) ;
#96187 = EDGE_LOOP ( 'NONE', ( #105871, #897, #71665, #17878 ) ) ;
#96188 = ORIENTED_EDGE ( 'NONE', *, *, #55455, .F. ) ;
#96189 = DIRECTION ( 'NONE',  ( 0.000000000000000000, 0.000000000000000000, -1.000000000000000000 ) ) ;
#96190 = CARTESIAN_POINT ( 'NONE',  ( -4.294665249841745289E-14, 2.500000000000000000, 4.922947341949748257 ) ) ;
#96191 = CIRCLE ( 'NONE', #39795, 0.06509327318403745899 ) ;
#96192 = VERTEX_POINT ( 'NONE', #2745 ) ;
#96193 = CARTESIAN_POINT ( 'NONE',  ( 14.34999999999989662, 2.500000000000000000, 1.818653347947321475 ) ) ;
#96194 = CARTESIAN_POINT ( 'NONE',  ( 17.50000000000000000, -0.9166666666666695162, -3.432456362931489036 ) ) ;
#96195 = CARTESIAN_POINT ( 'NONE',  ( 5.399999999999935518, 2.500000000000000000, -4.330127018922201643 ) ) ;
#96196 = ORIENTED_EDGE ( 'NONE', *, *, #70517, .T. ) ;
#96197 = DIRECTION ( 'NONE',  ( 0.000000000000000000, 0.000000000000000000, 1.000000000000000000 ) ) ;
#96198 = AXIS2_PLACEMENT_3D ( 'NONE', #118970, #36065, #128828 ) ;
#96199 = CARTESIAN_POINT ( 'NONE',  ( 12.89999999999989910, 2.500000000000000000, 0.6928203230275494784 ) ) ;
#96200 = CIRCLE ( 'NONE', #41948, 0.06509327318403745899 ) ;
#96201 = ORIENTED_EDGE ( 'NONE', *, *, #17149, .T. ) ;
#96202 = CONICAL_SURFACE ( 'NONE', #10526, 0.1000000000000002554, 0.003490658503988666988 ) ;
#96203 = EDGE_LOOP ( 'NONE', ( #45879, #98788, #117034, #98381 ) ) ;
#96204 = VERTEX_POINT ( 'NONE', #42711 ) ;
#96205 = FACE_OUTER_BOUND ( 'NONE', #119294, .T. ) ;
#96206 = AXIS2_PLACEMENT_3D ( 'NONE', #90268, #128952, #50364 ) ;
#96207 = PLANE ( 'NONE',  #108811 ) ;
#96208 = ADVANCED_FACE ( 'NONE', ( #13852 ), #82620, .T. ) ;
#96209 = CONICAL_SURFACE ( 'NONE', #108743, 0.1000000000000002554, 0.003490658503988666988 ) ;
#96210 = ORIENTED_EDGE ( 'NONE', *, *, #67722, .F. ) ;
#96211 = DIRECTION ( 'NONE',  ( 0.000000000000000000, 0.000000000000000000, 1.000000000000000000 ) ) ;
#96212 = DIRECTION ( 'NONE',  ( 0.000000000000000000, -0.000000000000000000, 1.000000000000000000 ) ) ;
#96213 = EDGE_CURVE ( 'NONE', #105627, #1738, #88977, .T. ) ;
#96214 = CARTESIAN_POINT ( 'NONE',  ( -7.100000000000014744, 2.500000000000000000, 4.330127018922196314 ) ) ;
#96215 = FACE_OUTER_BOUND ( 'NONE', #125248, .T. ) ;
#96216 = EDGE_CURVE ( 'NONE', #119760, #8618, #13652, .T. ) ;
#96217 = ORIENTED_EDGE ( 'NONE', *, *, #121865, .F. ) ;
#96218 = DIRECTION ( 'NONE',  ( 0.000000000000000000, 0.000000000000000000, 1.000000000000000000 ) ) ;
#96219 = ORIENTED_EDGE ( 'NONE', *, *, #71905, .F. ) ;
#96220 = ADVANCED_FACE ( 'NONE', ( #114629 ), #55715, .T. ) ;
#96222 = EDGE_LOOP ( 'NONE', ( #118522, #63154 ) ) ;
#96221 = ADVANCED_FACE ( 'NONE', ( #7242 ), #19934, .T. ) ;
#96223 = VERTEX_POINT ( 'NONE', #87742 ) ;
#96224 = EDGE_CURVE ( 'NONE', #89145, #3186, #17041, .T. ) ;
#96226 = EDGE_CURVE ( 'NONE', #44658, #21383, #70112, .T. ) ;
#96225 = CARTESIAN_POINT ( 'NONE',  ( 10.64999999999990976, 2.500000000000000000, 2.411473670974873862 ) ) ;
#96227 = ADVANCED_FACE ( 'NONE', ( #46530 ), #51345, .T. ) ;
#96228 = FACE_BOUND ( 'NONE', #8075, .T. ) ;
#96229 = CARTESIAN_POINT ( 'NONE',  ( -7.500000000000011546, 12.50000000000000000, 3.572213422710607489 ) ) ;
#96230 = CARTESIAN_POINT ( 'NONE',  ( 2.899999999999945732, 12.50000000000000000, -2.385244779468109755E-15 ) ) ;
#96231 = CARTESIAN_POINT ( 'NONE',  ( 7.499999999999925393, 12.50000000000000000, 4.957854068765711553 ) ) ;
#96232 = AXIS2_PLACEMENT_3D ( 'NONE', #42255, #42921, #31158 ) ;
#96233 = ORIENTED_EDGE ( 'NONE', *, *, #99926, .T. ) ;
#96235 = CONICAL_SURFACE ( 'NONE', #115020, 0.1000000000000000472, 0.003490658503988666988 ) ;
#96234 = CYLINDRICAL_SURFACE ( 'NONE', #8378, 2.318304356886073059 ) ;
#96236 = DIRECTION ( 'NONE',  ( -1.000000000000000000, 0.000000000000000000, 0.000000000000000000 ) ) ;
#96237 = EDGE_CURVE ( 'NONE', #117173, #19230, #93101, .T. ) ;
#96238 = DIRECTION ( 'NONE',  ( 0.000000000000000000, 1.000000000000000000, 0.000000000000000000 ) ) ;
#96239 = LINE ( 'NONE', #77262, #57319 ) ;
#96240 = ORIENTED_EDGE ( 'NONE', *, *, #104277, .T. ) ;
#96241 = CARTESIAN_POINT ( 'NONE',  ( -3.350000000000028511, 12.50000000000000000, -1.472243186433550122 ) ) ;
#96242 = CONICAL_SURFACE ( 'NONE', #27201, 0.1000000000000002554, 0.003490658503988666988 ) ;
#96243 = DIRECTION ( 'NONE',  ( 0.000000000000000000, 0.000000000000000000, 1.000000000000000000 ) ) ;
#96244 = EDGE_LOOP ( 'NONE', ( #112866, #61347, #19194, #87832 ) ) ;
#96245 = CARTESIAN_POINT ( 'NONE',  ( 2.099999999999947686, 2.500000000000000000, 5.022947341949748790 ) ) ;
#96246 = CARTESIAN_POINT ( 'NONE',  ( -1.850000000000033396, 12.50000000000000000, -6.906693963081115051 ) ) ;
#96247 = FACE_BOUND ( 'NONE', #88740, .T. ) ;
#96248 = DIRECTION ( 'NONE',  ( 0.000000000000000000, -1.846105847067148515E-16, -1.000000000000000000 ) ) ;
#96249 = ORIENTED_EDGE ( 'NONE', *, *, #74995, .T. ) ;
#96250 = CARTESIAN_POINT ( 'NONE',  ( 4.149999999999936406, 12.50000000000000000, 6.430097255199259010 ) ) ;
#96251 = CARTESIAN_POINT ( 'NONE',  ( -3.950000000000025491, 2.500000000000000000, 6.248780366869521430 ) ) ;
#96252 = VERTEX_POINT ( 'NONE', #36743 ) ;
#96253 = ORIENTED_EDGE ( 'NONE', *, *, #120084, .F. ) ;
#96254 = CARTESIAN_POINT ( 'NONE',  ( 183.9635416670080872, -4.367472073101519747, 7.564683531249999149 ) ) ;
#96255 = ORIENTED_EDGE ( 'NONE', *, *, #78669, .F. ) ;
#96256 = CARTESIAN_POINT ( 'NONE',  ( 184.5026531346524905, -6.417290985200525100, 4.014293029178955585 ) ) ;
#96257 = DIRECTION ( 'NONE',  ( 0.000000000000000000, 0.000000000000000000, -1.000000000000000000 ) ) ;
#96258 = CARTESIAN_POINT ( 'NONE',  ( 5.599999999999931255, 12.50000000000000000, 4.676537180435972552 ) ) ;
#96259 = DIRECTION ( 'NONE',  ( 0.000000000000000000, 0.000000000000000000, -1.000000000000000000 ) ) ;
#96260 = EDGE_CURVE ( 'NONE', #92915, #86749, #3216, .T. ) ;
#96261 = EDGE_CURVE ( 'NONE', #49329, #2409, #68038, .T. ) ;
#96262 = CARTESIAN_POINT ( 'NONE',  ( -9.550000000000006040, 12.50000000000000000, -2.165063509461101710 ) ) ;
#96263 = ADVANCED_FACE ( 'NONE', ( #115926 ), #37383, .T. ) ;
#96264 = CONICAL_SURFACE ( 'NONE', #75343, 0.1000000000000002554, 0.003490658503988666988 ) ;
#96265 = AXIS2_PLACEMENT_3D ( 'NONE', #9076, #30677, #11654 ) ;
#96266 = EDGE_LOOP ( 'NONE', ( #26532, #105914, #91804, #38753 ) ) ;
#96267 = EDGE_CURVE ( 'NONE', #120717, #114882, #26906, .T. ) ;
#96268 = DIRECTION ( 'NONE',  ( 0.000000000000000000, 0.000000000000000000, 1.000000000000000000 ) ) ;
#96269 = CARTESIAN_POINT ( 'NONE',  ( 2.500000000000002220, -2.500000000000000000, -8.999999999999998224 ) ) ;
#96270 = LINE ( 'NONE', #6579, #61799 ) ;
#96271 = LINE ( 'NONE', #96924, #13505 ) ;
#96273 = VERTEX_POINT ( 'NONE', #117182 ) ;
#96272 = ORIENTED_EDGE ( 'NONE', *, *, #43511, .T. ) ;
#96274 = FACE_BOUND ( 'NONE', #124881, .T. ) ;
#96275 = ORIENTED_EDGE ( 'NONE', *, *, #28438, .F. ) ;
#96276 = EDGE_CURVE ( 'NONE', #585, #48425, #11605, .T. ) ;
#96277 = DIRECTION ( 'NONE',  ( 0.000000000000000000, 0.000000000000000000, 1.000000000000000000 ) ) ;
#96278 = DIRECTION ( 'NONE',  ( 0.000000000000000000, 1.000000000000000000, 0.000000000000000000 ) ) ;
#96279 = VECTOR ( 'NONE', #47625, 1000.000000000000000 ) ;
#96281 = VERTEX_POINT ( 'NONE', #24970 ) ;
#96280 = EDGE_CURVE ( 'NONE', #30789, #81006, #26290, .T. ) ;
#96282 = LINE ( 'NONE', #67451, #5129 ) ;
#96283 = CARTESIAN_POINT ( 'NONE',  ( 87.50000000000001421, -3.974992050023848922, -6.359987280038160051 ) ) ;
#96284 = EDGE_CURVE ( 'NONE', #113131, #110912, #24140, .T. ) ;
#96285 = CARTESIAN_POINT ( 'NONE',  ( -6.450000000000016165, 2.500000000000000000, 6.841600689897072485 ) ) ;
#96286 = ADVANCED_FACE ( 'NONE', ( #96923 ), #45911, .T. ) ;
#96287 = CARTESIAN_POINT ( 'NONE',  ( -10.84999999999999964, 12.50000000000000000, 2.857883832488649301 ) ) ;
#96288 = ORIENTED_EDGE ( 'NONE', *, *, #30866, .T. ) ;
#96289 = DIRECTION ( 'NONE',  ( 0.000000000000000000, -0.9999939076577903929, 0.003490651415223739937 ) ) ;
#96290 = CARTESIAN_POINT ( 'NONE',  ( 13.54999999999989591, 2.500000000000000000, -1.918653347947326004 ) ) ;
#96291 = CARTESIAN_POINT ( 'NONE',  ( -12.29999999999999538, 12.50000000000000000, 4.676537180435972552 ) ) ;
#96292 = DIRECTION ( 'NONE',  ( 0.000000000000000000, 0.000000000000000000, 1.000000000000000000 ) ) ;
#96294 = EDGE_CURVE ( 'NONE', #29207, #60583, #36084, .T. ) ;
#96293 = DIRECTION ( 'NONE',  ( -4.274815082592931898E-19, -0.9999939076577903929, -0.003490651415223739937 ) ) ;
#96295 = VECTOR ( 'NONE', #3196, 1000.000000000000000 ) ;
#96296 = ORIENTED_EDGE ( 'NONE', *, *, #39128, .F. ) ;
#96297 = AXIS2_PLACEMENT_3D ( 'NONE', #58110, #7042, #96718 ) ;
#96298 = ORIENTED_EDGE ( 'NONE', *, *, #93601, .T. ) ;
#96299 = DIRECTION ( 'NONE',  ( 0.000000000000000000, 0.000000000000000000, 1.000000000000000000 ) ) ;
#96300 = ORIENTED_EDGE ( 'NONE', *, *, #90389, .T. ) ;
#96301 = CARTESIAN_POINT ( 'NONE',  ( -10.40000000000000213, 2.500000000000000000, 4.230127018922196669 ) ) ;
#96303 = ORIENTED_EDGE ( 'NONE', *, *, #68874, .T. ) ;
#96302 = ORIENTED_EDGE ( 'NONE', *, *, #35542, .F. ) ;
#96304 = ORIENTED_EDGE ( 'NONE', *, *, #52989, .T. ) ;
#96305 = CARTESIAN_POINT ( 'NONE',  ( -14.34999999999998543, 12.50000000000000000, -1.883746621131361154 ) ) ;
#96306 = AXIS2_PLACEMENT_3D ( 'NONE', #22220, #62136, #42498 ) ;
#96307 = DIRECTION ( 'NONE',  ( 0.000000000000000000, 1.000000000000000000, 0.000000000000000000 ) ) ;
#96308 = CYLINDRICAL_SURFACE ( 'NONE', #82347, 2.249999999999996891 ) ;
#96309 = DIRECTION ( 'NONE',  ( -0.000000000000000000, -1.000000000000000000, -0.000000000000000000 ) ) ;
#96310 = CIRCLE ( 'NONE', #18939, 0.09999999999999982514 ) ;
#96311 = LINE ( 'NONE', #87139, #71075 ) ;
#96312 = DIRECTION ( 'NONE',  ( -0.000000000000000000, -1.000000000000000000, -0.000000000000000000 ) ) ;
#96313 = EDGE_CURVE ( 'NONE', #108949, #112141, #96270, .T. ) ;
#96314 = ORIENTED_EDGE ( 'NONE', *, *, #42513, .F. ) ;
#96315 = DIRECTION ( 'NONE',  ( 0.000000000000000000, 1.000000000000000000, 0.000000000000000000 ) ) ;
#96316 = ORIENTED_EDGE ( 'NONE', *, *, #54347, .T. ) ;
#96317 = ORIENTED_EDGE ( 'NONE', *, *, #45862, .T. ) ;
#96318 = ORIENTED_EDGE ( 'NONE', *, *, #10403, .T. ) ;
#96319 = ORIENTED_EDGE ( 'NONE', *, *, #29787, .F. ) ;
#96320 = DIRECTION ( 'NONE',  ( -4.274815082592931898E-19, -0.9999939076577903929, -0.003490651415223739937 ) ) ;
#96321 = ORIENTED_EDGE ( 'NONE', *, *, #47711, .T. ) ;
#96322 = VERTEX_POINT ( 'NONE', #87104 ) ;
#96323 = DIRECTION ( 'NONE',  ( 0.000000000000000000, 0.000000000000000000, -1.000000000000000000 ) ) ;
#96324 = DIRECTION ( 'NONE',  ( -0.000000000000000000, 1.000000000000000000, -0.000000000000000000 ) ) ;
#96325 = EDGE_CURVE ( 'NONE', #63506, #104598, #76369, .T. ) ;
#96326 = PLANE ( 'NONE',  #92320 ) ;
#96327 = CARTESIAN_POINT ( 'NONE',  ( 0.7999999999999553024, 2.500000000000000000, -4.330127018922201643 ) ) ;
#96328 = AXIS2_PLACEMENT_3D ( 'NONE', #83476, #53364, #93280 ) ;
#96329 = LINE ( 'NONE', #8585, #126153 ) ;
#96330 = EDGE_LOOP ( 'NONE', ( #73072, #42798, #86437, #40285 ) ) ;
#96331 = AXIS2_PLACEMENT_3D ( 'NONE', #47421, #118076, #69625 ) ;
#96332 = AXIS2_PLACEMENT_3D ( 'NONE', #82171, #102457, #92632 ) ;
#96333 = LINE ( 'NONE', #60781, #53359 ) ;
#96334 = VERTEX_POINT ( 'NONE', #49787 ) ;
#96335 = CARTESIAN_POINT ( 'NONE',  ( -0.6500000000000403233, 2.500000000000000000, 6.048780366869520364 ) ) ;
#96336 = MECHANICAL_DESIGN_GEOMETRIC_PRESENTATION_REPRESENTATION (  '', ( #85869 ), #75414 ) ;
#96337 = ORIENTED_EDGE ( 'NONE', *, *, #91890, .T. ) ;
#96338 = DIRECTION ( 'NONE',  ( 0.000000000000000000, 0.000000000000000000, -1.000000000000000000 ) ) ;
#96339 = EDGE_LOOP ( 'NONE', ( #100609, #81496, #86110, #22883 ) ) ;
#96340 = AXIS2_PLACEMENT_3D ( 'NONE', #127400, #9559, #47554 ) ;
#96341 = EDGE_CURVE ( 'NONE', #85026, #12477, #77932, .T. ) ;
#96342 = ORIENTED_EDGE ( 'NONE', *, *, #101381, .F. ) ;
#96343 = DIRECTION ( 'NONE',  ( 0.000000000000000000, 1.000000000000000000, 0.000000000000000000 ) ) ;
#96344 = FACE_OUTER_BOUND ( 'NONE', #14903, .T. ) ;
#96345 = CARTESIAN_POINT ( 'NONE',  ( -4.293440603042597559E-14, 2.500000000000000000, 5.022947341949748790 ) ) ;
#96346 = DIRECTION ( 'NONE',  ( -0.000000000000000000, 1.000000000000000000, -0.000000000000000000 ) ) ;
#96347 = DIRECTION ( 'NONE',  ( 0.000000000000000000, 0.000000000000000000, -1.000000000000000000 ) ) ;
#96348 = ORIENTED_EDGE ( 'NONE', *, *, #84984, .F. ) ;
#96349 = DIRECTION ( 'NONE',  ( 0.000000000000000000, 1.000000000000000000, 0.000000000000000000 ) ) ;
#96350 = DIRECTION ( 'NONE',  ( -4.274815082592931898E-19, -0.9999939076577903929, -0.003490651415223739937 ) ) ;
#96351 = DIRECTION ( 'NONE',  ( 0.000000000000000000, 0.000000000000000000, -1.000000000000000000 ) ) ;
#96352 = DIRECTION ( 'NONE',  ( 0.000000000000000000, 0.000000000000000000, 1.000000000000000000 ) ) ;
#96353 = CARTESIAN_POINT ( 'NONE',  ( -0.8500000000000386136, 2.500000000000000000, 2.757883832488649656 ) ) ;
#96354 = EDGE_LOOP ( 'NONE', ( #67484, #116185, #122656, #88133 ) ) ;
#96355 = AXIS2_PLACEMENT_3D ( 'NONE', #6439, #127546, #97431 ) ;
#96356 = ORIENTED_EDGE ( 'NONE', *, *, #90143, .F. ) ;
#96357 = CARTESIAN_POINT ( 'NONE',  ( -3.150000000000030109, 2.500000000000000000, 1.718653347947321386 ) ) ;
#96358 = ORIENTED_EDGE ( 'NONE', *, *, #47660, .T. ) ;
#96359 = DIRECTION ( 'NONE',  ( 0.000000000000000000, 0.000000000000000000, -1.000000000000000000 ) ) ;
#96360 = AXIS2_PLACEMENT_3D ( 'NONE', #117110, #77214, #127602 ) ;
#96361 = DIRECTION ( 'NONE',  ( -0.000000000000000000, -1.000000000000000000, -0.000000000000000000 ) ) ;
#96362 = AXIS2_PLACEMENT_3D ( 'NONE', #48205, #6960, #46263 ) ;
#96363 = EDGE_CURVE ( 'NONE', #118657, #27686, #78536, .T. ) ;
#96364 = ORIENTED_EDGE ( 'NONE', *, *, #14507, .T. ) ;
#96365 = CARTESIAN_POINT ( 'NONE',  ( 186.0833333333333144, -6.668395609140180369, 3.849999999999994760 ) ) ;
#96366 = FACE_OUTER_BOUND ( 'NONE', #81061, .T. ) ;
#96367 = FACE_OUTER_BOUND ( 'NONE', #31508, .T. ) ;
#96368 = CARTESIAN_POINT ( 'NONE',  ( -11.44999999999999751, 2.500000000000000000, -2.611473670974873595 ) ) ;
#96369 = CARTESIAN_POINT ( 'NONE',  ( 1.899999999999951283, 12.50000000000000000, -3.983716857408426293 ) ) ;
#96370 = ORIENTED_EDGE ( 'NONE', *, *, #98979, .F. ) ;
#96371 = EDGE_CURVE ( 'NONE', #52515, #32613, #28343, .T. ) ;
#96372 = AXIS2_PLACEMENT_3D ( 'NONE', #129052, #9255, #28904 ) ;
#96373 = DIRECTION ( 'NONE',  ( 0.000000000000000000, 1.000000000000000000, 0.000000000000000000 ) ) ;
#96374 = CARTESIAN_POINT ( 'NONE',  ( -2.300000000000033129, 12.50000000000000000, 3.983716857408420076 ) ) ;
#96375 = ORIENTED_EDGE ( 'NONE', *, *, #14381, .T. ) ;
#96376 = EDGE_CURVE ( 'NONE', #40814, #32532, #43034, .T. ) ;
#96377 = ADVANCED_FACE ( 'NONE', ( #20953 ), #128352, .T. ) ;
#96378 = EDGE_CURVE ( 'NONE', #7910, #110892, #59754, .T. ) ;
#96380 = EDGE_CURVE ( 'NONE', #125657, #102321, #22095, .T. ) ;
#96379 = PLANE ( 'NONE',  #48505 ) ;
#96381 = DIRECTION ( 'NONE',  ( -0.000000000000000000, -1.000000000000000000, -0.000000000000000000 ) ) ;
#96382 = CARTESIAN_POINT ( 'NONE',  ( 2.899999999999944844, 12.50000000000000000, 4.957854068765711553 ) ) ;
#96383 = CONICAL_SURFACE ( 'NONE', #111044, 0.09999999999999982514, 0.003490658503988666988 ) ;
#96384 = CONICAL_SURFACE ( 'NONE', #86005, 0.1000000000000000472, 0.003490658503988666988 ) ;
#96385 = VERTEX_POINT ( 'NONE', #79240 ) ;
#96386 = DIRECTION ( 'NONE',  ( 0.000000000000000000, 1.000000000000000000, 0.000000000000000000 ) ) ;
#96387 = ORIENTED_EDGE ( 'NONE', *, *, #104305, .T. ) ;
#96388 = CARTESIAN_POINT ( 'NONE',  ( -8.300000000000011369, 2.500000000000000000, -4.230127018922201998 ) ) ;
#96389 = DIRECTION ( 'NONE',  ( 0.000000000000000000, 1.000000000000000000, 0.000000000000000000 ) ) ;
#96390 = EDGE_CURVE ( 'NONE', #83631, #49637, #58952, .T. ) ;
#96391 = CIRCLE ( 'NONE', #75471, 0.1000000000000000472 ) ;
#96392 = DIRECTION ( 'NONE',  ( 0.000000000000000000, 0.000000000000000000, 1.000000000000000000 ) ) ;
#96393 = EDGE_LOOP ( 'NONE', ( #42926, #9817, #57971, #11249 ) ) ;
#96394 = EDGE_CURVE ( 'NONE', #82278, #49864, #38685, .T. ) ;
#96396 = EDGE_CURVE ( 'NONE', #48604, #28288, #9647, .T. ) ;
#96395 = DIRECTION ( 'NONE',  ( -0.000000000000000000, -1.000000000000000000, -0.000000000000000000 ) ) ;
#96397 = DIRECTION ( 'NONE',  ( 0.000000000000000000, 0.000000000000000000, -1.000000000000000000 ) ) ;
#96398 = VECTOR ( 'NONE', #114149, 1000.000000000000000 ) ;
#96399 = AXIS2_PLACEMENT_3D ( 'NONE', #26635, #66546, #129376 ) ;
#96400 = ORIENTED_EDGE ( 'NONE', *, *, #127851, .T. ) ;
#96401 = VERTEX_POINT ( 'NONE', #18364 ) ;
#96402 = FACE_OUTER_BOUND ( 'NONE', #74722, .T. ) ;
#96403 = EDGE_LOOP ( 'NONE', ( #113854, #40812 ) ) ;
#96404 = DIRECTION ( 'NONE',  ( 0.000000000000000000, 0.000000000000000000, 1.000000000000000000 ) ) ;
#96405 = CARTESIAN_POINT ( 'NONE',  ( -3.950000000000026379, 2.500000000000000000, 2.611473670974873151 ) ) ;
#96406 = EDGE_LOOP ( 'NONE', ( #101153, #34998 ) ) ;
#96407 = VERTEX_POINT ( 'NONE', #60874 ) ;
#96408 = CARTESIAN_POINT ( 'NONE',  ( -8.100000000000010303, 2.500000000000000000, 4.576537180435972019 ) ) ;
#96409 = FACE_OUTER_BOUND ( 'NONE', #107286, .T. ) ;
#96410 = ORIENTED_EDGE ( 'NONE', *, *, #109397, .T. ) ;
#96411 = DIRECTION ( 'NONE',  ( 0.000000000000000000, -0.000000000000000000, 1.000000000000000000 ) ) ;
#96412 = CARTESIAN_POINT ( 'NONE',  ( 14.54999999999989235, 2.500000000000000000, -2.265063509461101798 ) ) ;
#96413 = AXIS2_PLACEMENT_3D ( 'NONE', #34713, #6472, #87639 ) ;
#96414 = CARTESIAN_POINT ( 'NONE',  ( -11.44999999999999929, 12.50000000000000000, -6.083687093685485436 ) ) ;
#96415 = DIRECTION ( 'NONE',  ( 1.000000000000000000, -0.000000000000000000, -1.084202172485504434E-16 ) ) ;
#96416 = AXIS2_PLACEMENT_3D ( 'NONE', #119859, #84281, #34568 ) ;
#96417 = AXIS2_PLACEMENT_3D ( 'NONE', #89258, #27747, #69611 ) ;
#96418 = DIRECTION ( 'NONE',  ( 0.000000000000000000, 0.000000000000000000, 1.000000000000000000 ) ) ;
#96419 = CARTESIAN_POINT ( 'NONE',  ( 185.1145833340161175, 6.668395609140177704, -3.849999999999998312 ) ) ;
#96420 = CIRCLE ( 'NONE', #40022, 0.09999999999999982514 ) ;
#96421 = ORIENTED_EDGE ( 'NONE', *, *, #37870, .F. ) ;
#96423 = ORIENTED_EDGE ( 'NONE', *, *, #119114, .T. ) ;
#96422 = CONICAL_SURFACE ( 'NONE', #40024, 0.1000000000000000056, 0.003490658503988666988 ) ;
#96424 = ORIENTED_EDGE ( 'NONE', *, *, #25300, .F. ) ;
#96425 = VERTEX_POINT ( 'NONE', #98213 ) ;
#96426 = FACE_OUTER_BOUND ( 'NONE', #89076, .T. ) ;
#96427 = CARTESIAN_POINT ( 'NONE',  ( 2.499999999999983569, 12.50000000000000000, -4.265033745738164406 ) ) ;
#96428 = AXIS2_PLACEMENT_3D ( 'NONE', #89247, #39537, #79444 ) ;
#96429 = DIRECTION ( 'NONE',  ( 0.000000000000000000, -0.9999939076577903929, 0.003490651415223739937 ) ) ;
#96430 = EDGE_LOOP ( 'NONE', ( #9131, #65056 ) ) ;
#96431 = FACE_BOUND ( 'NONE', #66356, .T. ) ;
#96432 = ADVANCED_FACE ( 'NONE', ( #120444 ), #659, .T. ) ;
#96433 = DIRECTION ( 'NONE',  ( -0.000000000000000000, -1.000000000000000000, -0.000000000000000000 ) ) ;
#96434 = LINE ( 'NONE', #37544, #16640 ) ;
#96435 = EDGE_CURVE ( 'NONE', #85963, #110378, #92, .T. ) ;
#96436 = DIRECTION ( 'NONE',  ( -4.274815082592931898E-19, -0.9999939076577903929, -0.003490651415223739937 ) ) ;
#96437 = DIRECTION ( 'NONE',  ( 0.000000000000000000, 0.000000000000000000, 1.000000000000000000 ) ) ;
#96438 = EDGE_CURVE ( 'NONE', #115346, #41126, #78605, .T. ) ;
#96439 = PLANE ( 'NONE',  #24189 ) ;
#96440 = DIRECTION ( 'NONE',  ( -0.000000000000000000, -1.000000000000000000, -0.000000000000000000 ) ) ;
#96441 = DIRECTION ( 'NONE',  ( 0.000000000000000000, 0.000000000000000000, 1.000000000000000000 ) ) ;
#96442 = FACE_OUTER_BOUND ( 'NONE', #117769, .T. ) ;
#96443 = FACE_OUTER_BOUND ( 'NONE', #31674, .T. ) ;
#96445 = EDGE_CURVE ( 'NONE', #22282, #128788, #5428, .T. ) ;
#96444 = CARTESIAN_POINT ( 'NONE',  ( 9.349999999999919709, 12.50000000000000000, -6.213873640053564351 ) ) ;
#96446 = EDGE_LOOP ( 'NONE', ( #12271, #42372, #101404, #126333 ) ) ;
#96447 = ORIENTED_EDGE ( 'NONE', *, *, #129283, .F. ) ;
#96448 = ORIENTED_EDGE ( 'NONE', *, *, #95877, .F. ) ;
#96449 = ORIENTED_EDGE ( 'NONE', *, *, #97197, .F. ) ;
#96450 = DIRECTION ( 'NONE',  ( 0.000000000000000000, 0.000000000000000000, 1.000000000000000000 ) ) ;
#96451 = DIRECTION ( 'NONE',  ( -0.000000000000000000, 1.000000000000000000, -0.000000000000000000 ) ) ;
#96453 = EDGE_LOOP ( 'NONE', ( #76210, #119984 ) ) ;
#96452 = ORIENTED_EDGE ( 'NONE', *, *, #7725, .F. ) ;
#96454 = ORIENTED_EDGE ( 'NONE', *, *, #56126, .T. ) ;
#96455 = FACE_OUTER_BOUND ( 'NONE', #94198, .T. ) ;
#96456 = CIRCLE ( 'NONE', #65142, 0.06509327318403745899 ) ;
#96457 = CIRCLE ( 'NONE', #121493, 0.1000000000000002554 ) ;
#96458 = CARTESIAN_POINT ( 'NONE',  ( 4.913542845177470753, -1.500000000000381473, 9.942462991075531775 ) ) ;
#96459 = DIRECTION ( 'NONE',  ( -0.000000000000000000, 1.000000000000000000, -0.000000000000000000 ) ) ;
#96460 = DIRECTION ( 'NONE',  ( -0.000000000000000000, 1.000000000000000000, -0.000000000000000000 ) ) ;
#96461 = DIRECTION ( 'NONE',  ( 0.000000000000000000, -0.000000000000000000, 1.000000000000000000 ) ) ;
#96462 = EDGE_LOOP ( 'NONE', ( #1364, #31192, #113105, #64425 ) ) ;
#96463 = CONICAL_SURFACE ( 'NONE', #42112, 0.1000000000000000056, 0.003490658503988666988 ) ;
#96464 = ORIENTED_EDGE ( 'NONE', *, *, #38869, .F. ) ;
#96465 = EDGE_LOOP ( 'NONE', ( #76342, #54284 ) ) ;
#96466 = AXIS2_PLACEMENT_3D ( 'NONE', #41019, #21347, #51470 ) ;
#96467 = ORIENTED_EDGE ( 'NONE', *, *, #92572, .T. ) ;
#96468 = DIRECTION ( 'NONE',  ( -4.274815082592931898E-19, -0.9999939076577903929, -0.003490651415223739937 ) ) ;
#96469 = ORIENTED_EDGE ( 'NONE', *, *, #127682, .F. ) ;
#96470 = ORIENTED_EDGE ( 'NONE', *, *, #16942, .F. ) ;
#96471 = VECTOR ( 'NONE', #32513, 1000.000000000000000 ) ;
#96472 = CARTESIAN_POINT ( 'NONE',  ( -9.999999999999969802, 2.500000000000000000, 0.09999999999999772959 ) ) ;
#96473 = CIRCLE ( 'NONE', #40063, 0.06509327318403745899 ) ;
#96474 = CARTESIAN_POINT ( 'NONE',  ( 8.349999999999919709, 2.500000000000000000, -1.472243186433550122 ) ) ;
#96475 = CARTESIAN_POINT ( 'NONE',  ( -12.89999999999999147, 2.500000000000000000, 5.022947341949748790 ) ) ;
#96476 = EDGE_CURVE ( 'NONE', #71888, #22161, #9196, .T. ) ;
#96477 = FACE_OUTER_BOUND ( 'NONE', #1331, .T. ) ;
#96478 = AXIS2_PLACEMENT_3D ( 'NONE', #73042, #72409, #60659 ) ;
#96479 = CARTESIAN_POINT ( 'NONE',  ( 9.799999999999918998, 12.50000000000000000, -0.2813168883297408329 ) ) ;
#96480 = ORIENTED_EDGE ( 'NONE', *, *, #40688, .T. ) ;
#96481 = DIRECTION ( 'NONE',  ( 0.000000000000000000, 0.000000000000000000, 1.000000000000000000 ) ) ;
#96482 = VERTEX_POINT ( 'NONE', #69396 ) ;
#96483 = DIRECTION ( 'NONE',  ( -0.000000000000000000, 1.000000000000000000, -0.000000000000000000 ) ) ;
#96484 = ORIENTED_EDGE ( 'NONE', *, *, #42626, .F. ) ;
#96485 = DIRECTION ( 'NONE',  ( 0.000000000000000000, 0.000000000000000000, -1.000000000000000000 ) ) ;
#96486 = VECTOR ( 'NONE', #77440, 1000.000000000000000 ) ;
#96487 = AXIS2_PLACEMENT_3D ( 'NONE', #110346, #21991, #79602 ) ;
#96488 = FACE_OUTER_BOUND ( 'NONE', #47311, .T. ) ;
#96489 = VERTEX_POINT ( 'NONE', #119794 ) ;
#96490 = DIRECTION ( 'NONE',  ( 0.000000000000000000, 0.000000000000000000, 1.000000000000000000 ) ) ;
#96491 = ADVANCED_FACE ( 'NONE', ( #94203 ), #45166, .T. ) ;
#96492 = CARTESIAN_POINT ( 'NONE',  ( -11.25000000000000178, 12.50000000000000000, -1.472243186433546125 ) ) ;
#96493 = ORIENTED_EDGE ( 'NONE', *, *, #87411, .F. ) ;
#96494 = DIRECTION ( 'NONE',  ( 0.000000000000000000, 0.000000000000000000, -1.000000000000000000 ) ) ;
#96495 = ORIENTED_EDGE ( 'NONE', *, *, #2203, .F. ) ;
#96497 = VERTEX_POINT ( 'NONE', #41256 ) ;
#96496 = EDGE_CURVE ( 'NONE', #123090, #126709, #52995, .T. ) ;
#96498 = DIRECTION ( 'NONE',  ( 0.000000000000000000, 0.000000000000000000, -1.000000000000000000 ) ) ;
#96499 = DIRECTION ( 'NONE',  ( 0.000000000000000000, 0.000000000000000000, 1.000000000000000000 ) ) ;
#96500 = CARTESIAN_POINT ( 'NONE',  ( 185.5885416670080872, -6.551208109652273848, -3.782341765625003571 ) ) ;
#96501 = DIRECTION ( 'NONE',  ( 0.000000000000000000, 0.000000000000000000, 1.000000000000000000 ) ) ;
#96502 = CARTESIAN_POINT ( 'NONE',  ( 4.599999999999939249, 12.50000000000000000, -3.702399969078687292 ) ) ;
#96503 = CARTESIAN_POINT ( 'NONE',  ( 14.54999999999989235, 2.500000000000000000, -2.265063509461101798 ) ) ;
#96504 = AXIS2_PLACEMENT_3D ( 'NONE', #31396, #71966, #81756 ) ;
#96505 = VECTOR ( 'NONE', #123239, 1000.000000000000000 ) ;
#96506 = ORIENTED_EDGE ( 'NONE', *, *, #11407, .F. ) ;
#96507 = FACE_OUTER_BOUND ( 'NONE', #131, .T. ) ;
#96508 = AXIS2_PLACEMENT_3D ( 'NONE', #40563, #79813, #60827 ) ;
#96510 = ADVANCED_FACE ( 'NONE', ( #54279 ), #103652, .T. ) ;
#96509 = AXIS2_PLACEMENT_3D ( 'NONE', #106772, #103080, #13399 ) ;
#96511 = VERTEX_POINT ( 'NONE', #104029 ) ;
#96512 = CIRCLE ( 'NONE', #54759, 0.06509327318403745899 ) ;
#96513 = CONICAL_SURFACE ( 'NONE', #63088, 0.1000000000000000472, 0.003490658503988666988 ) ;
#96514 = DIRECTION ( 'NONE',  ( 0.000000000000000000, 0.000000000000000000, 1.000000000000000000 ) ) ;
#96515 = FACE_OUTER_BOUND ( 'NONE', #51848, .T. ) ;
#96516 = LINE ( 'NONE', #77535, #69452 ) ;
#96517 = DIRECTION ( 'NONE',  ( 0.000000000000000000, 0.000000000000000000, 1.000000000000000000 ) ) ;
#96518 = DIRECTION ( 'NONE',  ( 0.000000000000000000, 1.000000000000000000, 0.000000000000000000 ) ) ;
#96519 = ORIENTED_EDGE ( 'NONE', *, *, #25895, .F. ) ;
#96520 = EDGE_CURVE ( 'NONE', #63624, #119823, #1238, .T. ) ;
#96521 = DIRECTION ( 'NONE',  ( 0.000000000000000000, 1.000000000000000000, 0.000000000000000000 ) ) ;
#96522 = DIRECTION ( 'NONE',  ( 0.000000000000000000, 0.000000000000000000, -1.000000000000000000 ) ) ;
#96523 = ADVANCED_FACE ( 'NONE', ( #63462 ), #103384, .T. ) ;
#96524 = EDGE_CURVE ( 'NONE', #20444, #3575, #33372, .T. ) ;
#96525 = EDGE_CURVE ( 'NONE', #20333, #10004, #7490, .T. ) ;
#96526 = EDGE_CURVE ( 'NONE', #114323, #101653, #22264, .T. ) ;
#96527 = VERTEX_POINT ( 'NONE', #121722 ) ;
#96528 = DIRECTION ( 'NONE',  ( -0.000000000000000000, 1.000000000000000000, -0.000000000000000000 ) ) ;
#96529 = ORIENTED_EDGE ( 'NONE', *, *, #41220, .F. ) ;
#96530 = ORIENTED_EDGE ( 'NONE', *, *, #50270, .F. ) ;
#96531 = CARTESIAN_POINT ( 'NONE',  ( 9.149999999999916866, 2.500000000000000000, 7.088010851410848190 ) ) ;
#96532 = EDGE_CURVE ( 'NONE', #69316, #51138, #22189, .T. ) ;
#96533 = EDGE_CURVE ( 'NONE', #1764, #5270, #114106, .T. ) ;
#96534 = VERTEX_POINT ( 'NONE', #23522 ) ;
#96535 = CARTESIAN_POINT ( 'NONE',  ( -6.700000000000016165, 2.500000000000000000, 4.330127018922196314 ) ) ;
#96536 = FACE_OUTER_BOUND ( 'NONE', #123683, .T. ) ;
#96537 = FACE_OUTER_BOUND ( 'NONE', #45942, .T. ) ;
#96538 = CONICAL_SURFACE ( 'NONE', #107005, 0.09999999999999982514, 0.003490658503988666988 ) ;
#96539 = ORIENTED_EDGE ( 'NONE', *, *, #107130, .T. ) ;
#96541 = EDGE_CURVE ( 'NONE', #62955, #67958, #102715, .T. ) ;
#96540 = VECTOR ( 'NONE', #65601, 1000.000000000000000 ) ;
#96543 = EDGE_CURVE ( 'NONE', #86820, #63617, #93191, .T. ) ;
#96542 = FACE_BOUND ( 'NONE', #95581, .T. ) ;
#96545 = ORIENTED_EDGE ( 'NONE', *, *, #30411, .T. ) ;
#96544 = DIRECTION ( 'NONE',  ( -0.000000000000000000, 1.000000000000000000, -0.000000000000000000 ) ) ;
#96546 = CARTESIAN_POINT ( 'NONE',  ( 4.999999999999936939, 2.500000000000000000, -0.6928203230275541413 ) ) ;
#96547 = DIRECTION ( 'NONE',  ( 0.000000000000000000, 1.000000000000000000, 0.000000000000000000 ) ) ;
#96549 = ADVANCED_FACE ( 'NONE', ( #111240 ), #13741, .T. ) ;
#96548 = AXIS2_PLACEMENT_3D ( 'NONE', #48268, #97368, #77712 ) ;
#96550 = ADVANCED_FACE ( 'NONE', ( #24177 ), #30510, .T. ) ;
#96551 = ORIENTED_EDGE ( 'NONE', *, *, #69446, .F. ) ;
#96552 = AXIS2_PLACEMENT_3D ( 'NONE', #60612, #62539, #40322 ) ;
#96553 = CIRCLE ( 'NONE', #17117, 0.06509327318403745899 ) ;
#96554 = EDGE_LOOP ( 'NONE', ( #101295, #31553, #114951, #118471 ) ) ;
#96555 = ORIENTED_EDGE ( 'NONE', *, *, #25797, .F. ) ;
#96556 = DIRECTION ( 'NONE',  ( 0.000000000000000000, 0.000000000000000000, -1.000000000000000000 ) ) ;
#96557 = LINE ( 'NONE', #58597, #60367 ) ;
#96558 = DIRECTION ( 'NONE',  ( 0.000000000000000000, 0.000000000000000000, -1.000000000000000000 ) ) ;
#96559 = FACE_BOUND ( 'NONE', #82922, .T. ) ;
#96560 = ORIENTED_EDGE ( 'NONE', *, *, #18074, .F. ) ;
#96561 = DIRECTION ( 'NONE',  ( 0.000000000000000000, 0.000000000000000000, 1.000000000000000000 ) ) ;
#96562 = CARTESIAN_POINT ( 'NONE',  ( -11.89999999999999680, 12.50000000000000000, -4.676537180435976104 ) ) ;
#96563 = CIRCLE ( 'NONE', #33891, 0.09999999999999982514 ) ;
#96564 = CONICAL_SURFACE ( 'NONE', #77787, 0.1000000000000002554, 0.003490658503988666988 ) ;
#96565 = FACE_OUTER_BOUND ( 'NONE', #125471, .T. ) ;
#96566 = CIRCLE ( 'NONE', #54811, 0.1000000000000000472 ) ;
#96567 = VECTOR ( 'NONE', #96320, 1000.000000000000000 ) ;
#96568 = CONICAL_SURFACE ( 'NONE', #31844, 0.09999999999999982514, 0.003490658503988666988 ) ;
#96569 = DIRECTION ( 'NONE',  ( 0.000000000000000000, 0.000000000000000000, 1.000000000000000000 ) ) ;
#96570 = DIRECTION ( 'NONE',  ( 0.000000000000000000, 1.000000000000000000, 0.000000000000000000 ) ) ;
#96571 = CARTESIAN_POINT ( 'NONE',  ( -8.350000000000012079, 12.50000000000000000, 2.922977105672686982 ) ) ;
#96572 = CIRCLE ( 'NONE', #104986, 0.1000000000000002554 ) ;
#96573 = DIRECTION ( 'NONE',  ( 0.000000000000000000, -0.9999939076577903929, 0.003490651415223739937 ) ) ;
#96574 = ORIENTED_EDGE ( 'NONE', *, *, #20183, .F. ) ;
#96575 = CIRCLE ( 'NONE', #27526, 0.06509327318403745899 ) ;
#96576 = ORIENTED_EDGE ( 'NONE', *, *, #9099, .F. ) ;
#96577 = ORIENTED_EDGE ( 'NONE', *, *, #115973, .F. ) ;
#96578 = ORIENTED_EDGE ( 'NONE', *, *, #79518, .T. ) ;
#96579 = EDGE_LOOP ( 'NONE', ( #74792, #45596 ) ) ;
#96580 = DIRECTION ( 'NONE',  ( -0.000000000000000000, -1.000000000000000000, -0.000000000000000000 ) ) ;
#96581 = PLANE ( 'NONE',  #96857 ) ;
#96582 = EDGE_LOOP ( 'NONE', ( #5822, #112205 ) ) ;
#96583 = FACE_BOUND ( 'NONE', #841, .T. ) ;
#96584 = CARTESIAN_POINT ( 'NONE',  ( 11.64999999999990798, 2.500000000000000000, -1.372243186433550033 ) ) ;
#96585 = ADVANCED_FACE ( 'NONE', ( #51712 ), #41899, .T. ) ;
#96586 = CARTESIAN_POINT ( 'NONE',  ( 3.349999999999941913, 2.500000000000000000, 5.702370205355745014 ) ) ;
#96587 = EDGE_CURVE ( 'NONE', #86863, #21611, #26380, .T. ) ;
#96588 = DIRECTION ( 'NONE',  ( 0.000000000000000000, -0.000000000000000000, 1.000000000000000000 ) ) ;
#96589 = FACE_OUTER_BOUND ( 'NONE', #67080, .T. ) ;
#96590 = DIRECTION ( 'NONE',  ( 0.000000000000000000, 0.000000000000000000, 1.000000000000000000 ) ) ;
#96591 = EDGE_LOOP ( 'NONE', ( #111916, #48403, #111101, #96825 ) ) ;
#96592 = DIRECTION ( 'NONE',  ( 0.000000000000000000, 0.000000000000000000, 1.000000000000000000 ) ) ;
#96593 = ORIENTED_EDGE ( 'NONE', *, *, #82404, .F. ) ;
#96594 = VERTEX_POINT ( 'NONE', #2578 ) ;
#96595 = VERTEX_POINT ( 'NONE', #82468 ) ;
#96596 = AXIS2_PLACEMENT_3D ( 'NONE', #46023, #15234, #76115 ) ;
#96597 = CARTESIAN_POINT ( 'NONE',  ( 129.5000000000000000, -1.375000000000000000, 7.634788798650553154 ) ) ;
#96598 = CIRCLE ( 'NONE', #123788, 0.09999999999999982514 ) ;
#96599 = CARTESIAN_POINT ( 'NONE',  ( 4.849235612580145016, 2.499999999999999556, 8.943930330244967308 ) ) ;
#96600 = DIRECTION ( 'NONE',  ( 0.000000000000000000, -0.000000000000000000, 1.000000000000000000 ) ) ;
#96601 = ORIENTED_EDGE ( 'NONE', *, *, #18703, .T. ) ;
#96602 = CARTESIAN_POINT ( 'NONE',  ( 7.306656945318586338, 1.500000000000379918, -9.704971168320692954 ) ) ;
#96603 = CARTESIAN_POINT ( 'NONE',  ( 12.09999999999990195, 2.500000000000000000, -0.6928203230275541413 ) ) ;
#96604 = AXIS2_PLACEMENT_3D ( 'NONE', #35244, #54852, #56771 ) ;
#96605 = CIRCLE ( 'NONE', #109127, 0.06509327318403745899 ) ;
#96606 = DIRECTION ( 'NONE',  ( 0.000000000000000000, 1.000000000000000000, 0.000000000000000000 ) ) ;
#96607 = CARTESIAN_POINT ( 'NONE',  ( 186.8177083336747160, 4.367472073101515306, 7.564683531250000925 ) ) ;
#96608 = DIRECTION ( 'NONE',  ( -0.000000000000000000, -1.000000000000000000, -0.000000000000000000 ) ) ;
#96609 = DIRECTION ( 'NONE',  ( -0.000000000000000000, -1.000000000000000000, -0.000000000000000000 ) ) ;
#96610 = CONICAL_SURFACE ( 'NONE', #100820, 0.1000000000000000472, 0.003490658503988666988 ) ;
#96611 = AXIS2_PLACEMENT_3D ( 'NONE', #54944, #56232, #86986 ) ;
#96612 = CARTESIAN_POINT ( 'NONE',  ( -10.84999999999999964, 2.500000000000000000, 1.572243186433545548 ) ) ;
#96613 = VERTEX_POINT ( 'NONE', #112567 ) ;
#96614 = DIRECTION ( 'NONE',  ( -0.000000000000000000, 1.000000000000000000, -0.000000000000000000 ) ) ;
#96615 = AXIS2_PLACEMENT_3D ( 'NONE', #46282, #6981, #95394 ) ;
#96616 = ORIENTED_EDGE ( 'NONE', *, *, #78766, .F. ) ;
#96617 = ORIENTED_EDGE ( 'NONE', *, *, #71054, .F. ) ;
#96618 = DIRECTION ( 'NONE',  ( -0.000000000000000000, -1.000000000000000000, -0.000000000000000000 ) ) ;
#96619 = DIRECTION ( 'NONE',  ( -4.274815082592931898E-19, -0.9999939076577903929, -0.003490651415223739937 ) ) ;
#96620 = FACE_OUTER_BOUND ( 'NONE', #123745, .T. ) ;
#96621 = EDGE_LOOP ( 'NONE', ( #118682, #5345 ) ) ;
#96622 = VERTEX_POINT ( 'NONE', #22899 ) ;
#96623 = ADVANCED_FACE ( 'NONE', ( #37232 ), #17959, .T. ) ;
#96624 = DIRECTION ( 'NONE',  ( 0.000000000000000000, 0.000000000000000000, -1.000000000000000000 ) ) ;
#96625 = CARTESIAN_POINT ( 'NONE',  ( -7.500000000000011546, 2.500000000000000000, 3.637306695894644726 ) ) ;
#96626 = CARTESIAN_POINT ( 'NONE',  ( 8.749999999999957367, 12.50000000000000000, -6.495190528383302464 ) ) ;
#96627 = ORIENTED_EDGE ( 'NONE', *, *, #122287, .F. ) ;
#96628 = ORIENTED_EDGE ( 'NONE', *, *, #113346, .F. ) ;
#96629 = DIRECTION ( 'NONE',  ( -4.274815082592931898E-19, -0.9999939076577903929, -0.003490651415223739937 ) ) ;
#96631 = ORIENTED_EDGE ( 'NONE', *, *, #72780, .F. ) ;
#96630 = VECTOR ( 'NONE', #258, 1000.000000000000000 ) ;
#96632 = DIRECTION ( 'NONE',  ( -0.000000000000000000, 1.000000000000000000, -0.000000000000000000 ) ) ;
#96633 = FACE_OUTER_BOUND ( 'NONE', #43336, .T. ) ;
#96634 = VERTEX_POINT ( 'NONE', #16261 ) ;
#96635 = CARTESIAN_POINT ( 'NONE',  ( 8.149999999999923972, 12.50000000000000000, 1.753560074763284016 ) ) ;
#96636 = CARTESIAN_POINT ( 'NONE',  ( 11.04999999999991012, 2.500000000000000000, 6.941600689897073018 ) ) ;
#96637 = DIRECTION ( 'NONE',  ( 0.000000000000000000, 0.000000000000000000, 1.000000000000000000 ) ) ;
#96638 = ADVANCED_FACE ( 'NONE', ( #75840 ), #99544, .T. ) ;
#96639 = EDGE_CURVE ( 'NONE', #11311, #37370, #116242, .T. ) ;
#96641 = CIRCLE ( 'NONE', #105055, 0.06509327318403745899 ) ;
#96640 = CARTESIAN_POINT ( 'NONE',  ( 8.749999999999957367, 2.500000000000000000, 2.165063509461097713 ) ) ;
#96642 = ORIENTED_EDGE ( 'NONE', *, *, #117601, .F. ) ;
#96643 = VECTOR ( 'NONE', #68966, 1000.000000000000000 ) ;
#96644 = CONICAL_SURFACE ( 'NONE', #105058, 0.1000000000000002554, 0.003490658503988666988 ) ;
#96645 = CARTESIAN_POINT ( 'NONE',  ( -11.64999999999999680, 2.500000000000000000, 1.572243186433545548 ) ) ;
#96646 = CIRCLE ( 'NONE', #63217, 0.06509327318403745899 ) ;
#96647 = LINE ( 'NONE', #85558, #49959 ) ;
#96648 = ORIENTED_EDGE ( 'NONE', *, *, #113973, .T. ) ;
#96649 = VERTEX_POINT ( 'NONE', #47048 ) ;
#96650 = EDGE_CURVE ( 'NONE', #78527, #68389, #74563, .T. ) ;
#96651 = CARTESIAN_POINT ( 'NONE',  ( 185.5885416670080872, -6.551208109652273848, -3.782341765625003571 ) ) ;
#96652 = CARTESIAN_POINT ( 'NONE',  ( -10.40000000000000213, 2.500000000000000000, 3.537306695894645081 ) ) ;
#96653 = CARTESIAN_POINT ( 'NONE',  ( -7.950000000000009059, 2.500000000000000000, 6.595190528383296780 ) ) ;
#96654 = DIRECTION ( 'NONE',  ( 0.000000000000000000, 0.000000000000000000, 1.000000000000000000 ) ) ;
#96655 = VECTOR ( 'NONE', #75310, 1000.000000000000000 ) ;
#96656 = DIRECTION ( 'NONE',  ( 0.000000000000000000, -0.9999939076577903929, 0.003490651415223739937 ) ) ;
#96657 = DIRECTION ( 'NONE',  ( 0.000000000000000000, 1.000000000000000000, 0.000000000000000000 ) ) ;
#96658 = CIRCLE ( 'NONE', #123854, 0.09999999999999982514 ) ;
#96659 = CARTESIAN_POINT ( 'NONE',  ( 16.88398418147296809, 2.500000000000000000, -4.430584152985972857 ) ) ;
#96660 = CONICAL_SURFACE ( 'NONE', #98721, 0.09999999999999999167, 0.003490658503988666988 ) ;
#96661 = CARTESIAN_POINT ( 'NONE',  ( 1.649999999999951505, 2.500000000000000000, 2.857883832488649301 ) ) ;
#96662 = CIRCLE ( 'NONE', #36047, 0.06509327318403741736 ) ;
#96663 = VECTOR ( 'NONE', #114494, 1000.000000000000000 ) ;
#96664 = PLANE ( 'NONE',  #104826 ) ;
#96665 = AXIS2_PLACEMENT_3D ( 'NONE', #64074, #33350, #104003 ) ;
#96666 = CARTESIAN_POINT ( 'NONE',  ( 3.949999999999941558, 12.50000000000000000, -1.753560074763288679 ) ) ;
#96667 = CONICAL_SURFACE ( 'NONE', #79963, 0.1000000000000000056, 0.003490658503988666988 ) ;
#96668 = ORIENTED_EDGE ( 'NONE', *, *, #81354, .T. ) ;
#96669 = DIRECTION ( 'NONE',  ( 0.000000000000000000, 0.000000000000000000, 1.000000000000000000 ) ) ;
#96670 = EDGE_LOOP ( 'NONE', ( #77129, #9859 ) ) ;
#96671 = DIRECTION ( 'NONE',  ( -0.000000000000000000, -1.000000000000000000, -0.000000000000000000 ) ) ;
#96672 = FACE_OUTER_BOUND ( 'NONE', #56202, .T. ) ;
#96673 = CARTESIAN_POINT ( 'NONE',  ( -10.60000000000000142, 2.500000000000000000, 4.676537180435972552 ) ) ;
#96674 = ORIENTED_EDGE ( 'NONE', *, *, #116340, .F. ) ;
#96675 = CARTESIAN_POINT ( 'NONE',  ( -12.29999999999999538, 12.50000000000000000, -0.2813168883297367806 ) ) ;
#96676 = ADVANCED_FACE ( 'NONE', ( #85667 ), #77143, .T. ) ;
#96677 = DIRECTION ( 'NONE',  ( -0.000000000000000000, 1.000000000000000000, -0.000000000000000000 ) ) ;
#96679 = ORIENTED_EDGE ( 'NONE', *, *, #68461, .F. ) ;
#96678 = CARTESIAN_POINT ( 'NONE',  ( -6.650000000000015454, 2.500000000000000000, 2.957883832488649389 ) ) ;
#96680 = AXIS2_PLACEMENT_3D ( 'NONE', #70769, #2652, #42619 ) ;
#96681 = EDGE_CURVE ( 'NONE', #8138, #79642, #40973, .T. ) ;
#96682 = EDGE_CURVE ( 'NONE', #63281, #8031, #112056, .T. ) ;
#96683 = LINE ( 'NONE', #14267, #45843 ) ;
#96684 = ORIENTED_EDGE ( 'NONE', *, *, #14699, .T. ) ;
#96685 = ORIENTED_EDGE ( 'NONE', *, *, #9125, .F. ) ;
#96686 = ORIENTED_EDGE ( 'NONE', *, *, #117217, .F. ) ;
#96687 = VECTOR ( 'NONE', #119435, 1000.000000000000000 ) ;
#96688 = ORIENTED_EDGE ( 'NONE', *, *, #12449, .F. ) ;
#96689 = DIRECTION ( 'NONE',  ( 0.000000000000000000, 1.000000000000000000, 0.000000000000000000 ) ) ;
#96690 = VECTOR ( 'NONE', #83122, 1000.000000000000000 ) ;
#96691 = ADVANCED_FACE ( 'NONE', ( #115102 ), #84856, .T. ) ;
#96692 = CIRCLE ( 'NONE', #42341, 0.06509327318403741736 ) ;
#96693 = EDGE_CURVE ( 'NONE', #126609, #128794, #105317, .T. ) ;
#96694 = EDGE_CURVE ( 'NONE', #110810, #125867, #55571, .T. ) ;
#96695 = DIRECTION ( 'NONE',  ( 0.9974916312695814025, 0.05217691604167131597, 0.04783319955355550684 ) ) ;
#96696 = DIRECTION ( 'NONE',  ( 0.000000000000000000, 1.000000000000000000, 0.000000000000000000 ) ) ;
#96697 = CARTESIAN_POINT ( 'NONE',  ( -14.99999999999998401, 2.500000000000000000, 0.7928203230275517877 ) ) ;
#96699 = ORIENTED_EDGE ( 'NONE', *, *, #66247, .T. ) ;
#96698 = AXIS2_PLACEMENT_3D ( 'NONE', #3299, #43243, #119845 ) ;
#96700 = AXIS2_PLACEMENT_3D ( 'NONE', #71923, #111836, #102645 ) ;
#96701 = AXIS2_PLACEMENT_3D ( 'NONE', #122140, #72397, #13447 ) ;
#96702 = EDGE_CURVE ( 'NONE', #97511, #109623, #28441, .T. ) ;
#96703 = CARTESIAN_POINT ( 'NONE',  ( -6.450000000000014388, 12.50000000000000000, 6.213873640053559022 ) ) ;
#96705 = VERTEX_POINT ( 'NONE', #26754 ) ;
#96704 = CIRCLE ( 'NONE', #90438, 0.1000000000000000472 ) ;
#96706 = CARTESIAN_POINT ( 'NONE',  ( 59.88499455115334769, -2.860410828890750157, -5.641292085239668630 ) ) ;
#96707 = DIRECTION ( 'NONE',  ( 0.000000000000000000, 0.000000000000000000, 1.000000000000000000 ) ) ;
#96708 = VECTOR ( 'NONE', #118155, 1000.000000000000000 ) ;
#96710 = CIRCLE ( 'NONE', #61227, 0.1000000000000002554 ) ;
#96709 = LINE ( 'NONE', #124900, #92322 ) ;
#96711 = FACE_OUTER_BOUND ( 'NONE', #104850, .T. ) ;
#96712 = EDGE_CURVE ( 'NONE', #27192, #17818, #96131, .T. ) ;
#96713 = AXIS2_PLACEMENT_3D ( 'NONE', #99273, #48887, #60006 ) ;
#96714 = ORIENTED_EDGE ( 'NONE', *, *, #65356, .F. ) ;
#96715 = EDGE_LOOP ( 'NONE', ( #26177, #53974, #54134, #78124 ) ) ;
#96716 = ORIENTED_EDGE ( 'NONE', *, *, #52377, .F. ) ;
#96717 = ORIENTED_EDGE ( 'NONE', *, *, #35258, .F. ) ;
#96718 = DIRECTION ( 'NONE',  ( 0.000000000000000000, 0.000000000000000000, 1.000000000000000000 ) ) ;
#96719 = CARTESIAN_POINT ( 'NONE',  ( 87.50000000000001421, 3.975350567648425759, 6.360562287258741065 ) ) ;
#96720 = DIRECTION ( 'NONE',  ( -4.274815082592931898E-19, -0.9999939076577903929, -0.003490651415223739937 ) ) ;
#96721 = FACE_BOUND ( 'NONE', #60859, .T. ) ;
#96722 = CARTESIAN_POINT ( 'NONE',  ( 142.3152275665817115, 0.5000000000000000000, 1.374601720185641973 ) ) ;
#96723 = PLANE ( 'NONE',  #100969 ) ;
#96724 = FACE_OUTER_BOUND ( 'NONE', #55831, .T. ) ;
#96725 = CARTESIAN_POINT ( 'NONE',  ( -3.950000000000024603, 12.50000000000000000, -2.576566944158915184 ) ) ;
#96726 = CARTESIAN_POINT ( 'NONE',  ( 184.2968750003414300, 8.734944146203032389, 5.348610694689227483E-16 ) ) ;
#96727 = DIRECTION ( 'NONE',  ( 0.000000000000000000, 0.000000000000000000, 1.000000000000000000 ) ) ;
#96728 = DIRECTION ( 'NONE',  ( 0.000000000000000000, 1.000000000000000000, 0.000000000000000000 ) ) ;
#96729 = AXIS2_PLACEMENT_3D ( 'NONE', #109258, #55818, #116021 ) ;
#96730 = AXIS2_PLACEMENT_3D ( 'NONE', #51380, #10754, #120740 ) ;
#96731 = AXIS2_PLACEMENT_3D ( 'NONE', #36082, #84533, #36740 ) ;
#96732 = DIRECTION ( 'NONE',  ( 0.000000000000000000, 0.000000000000000000, 1.000000000000000000 ) ) ;
#96733 = EDGE_LOOP ( 'NONE', ( #60809, #67217 ) ) ;
#96734 = VERTEX_POINT ( 'NONE', #14961 ) ;
#96735 = ORIENTED_EDGE ( 'NONE', *, *, #86370, .T. ) ;
#96736 = ORIENTED_EDGE ( 'NONE', *, *, #76289, .F. ) ;
#96737 = DIRECTION ( 'NONE',  ( 0.000000000000000000, 1.000000000000000000, 0.000000000000000000 ) ) ;
#96738 = FACE_BOUND ( 'NONE', #127095, .T. ) ;
#96739 = CONICAL_SURFACE ( 'NONE', #34070, 0.1000000000000002554, 0.003490658503988666988 ) ;
#96740 = DIRECTION ( 'NONE',  ( 0.000000000000000000, 0.000000000000000000, -1.000000000000000000 ) ) ;
#96741 = CARTESIAN_POINT ( 'NONE',  ( 7.949999999999922018, 2.500000000000000000, -2.265063509461101798 ) ) ;
#96742 = CONICAL_SURFACE ( 'NONE', #86276, 0.09999999999999982514, 0.003490658503988666988 ) ;
#96743 = ADVANCED_FACE ( 'NONE', ( #26115 ), #105790, .T. ) ;
#96744 = ORIENTED_EDGE ( 'NONE', *, *, #112240, .T. ) ;
#96745 = CARTESIAN_POINT ( 'NONE',  ( -3.950000000000026379, 12.50000000000000000, -1.753560074763288679 ) ) ;
#96746 = DIRECTION ( 'NONE',  ( 0.000000000000000000, 0.000000000000000000, -1.000000000000000000 ) ) ;
#96747 = EDGE_LOOP ( 'NONE', ( #126656, #5401 ) ) ;
#96748 = CARTESIAN_POINT ( 'NONE',  ( 0.000000000000000000, 0.000000000000000000, -5.000000000000004441 ) ) ;
#96749 = CARTESIAN_POINT ( 'NONE',  ( 19.95908882845296617, 2.629614671951221005, -2.273431397254392916 ) ) ;
#96750 = AXIS2_PLACEMENT_3D ( 'NONE', #635, #100761, #58929 ) ;
#96751 = EDGE_CURVE ( 'NONE', #9756, #54565, #32663, .T. ) ;
#96752 = CIRCLE ( 'NONE', #4809, 0.09999999999999999167 ) ;
#96753 = VECTOR ( 'NONE', #106642, 1000.000000000000000 ) ;
#96754 = VECTOR ( 'NONE', #86312, 1000.000000000000000 ) ;
#96755 = ORIENTED_EDGE ( 'NONE', *, *, #48588, .F. ) ;
#96756 = CARTESIAN_POINT ( 'NONE',  ( 0.7999999999999548583, 2.500000000000000000, 4.430127018922196847 ) ) ;
#96757 = FACE_OUTER_BOUND ( 'NONE', #93355, .T. ) ;
#96758 = CONICAL_SURFACE ( 'NONE', #100983, 0.09999999999999982514, 0.003490658503988666988 ) ;
#96759 = VERTEX_POINT ( 'NONE', #66027 ) ;
#96760 = DIRECTION ( 'NONE',  ( -0.000000000000000000, -1.000000000000000000, -0.000000000000000000 ) ) ;
#96761 = AXIS2_PLACEMENT_3D ( 'NONE', #109818, #60725, #91461 ) ;
#96762 = CARTESIAN_POINT ( 'NONE',  ( 4.149999999999939959, 12.50000000000000000, 2.857883832488649301 ) ) ;
#96763 = VERTEX_POINT ( 'NONE', #75207 ) ;
#96764 = CARTESIAN_POINT ( 'NONE',  ( 4.399999999999940847, 2.500000000000000000, -4.576537180435977348 ) ) ;
#96765 = EDGE_LOOP ( 'NONE', ( #104328, #81191, #84265, #70547 ) ) ;
#96766 = EDGE_LOOP ( 'NONE', ( #69830, #28558, #126984, #23249 ) ) ;
#96767 = DIRECTION ( 'NONE',  ( -1.000000000000000000, 0.000000000000000000, 0.000000000000000000 ) ) ;
#96768 = ORIENTED_EDGE ( 'NONE', *, *, #103004, .T. ) ;
#96769 = FACE_OUTER_BOUND ( 'NONE', #85200, .T. ) ;
#96770 = DIRECTION ( 'NONE',  ( -0.000000000000000000, 1.000000000000000000, -0.000000000000000000 ) ) ;
#96771 = EDGE_LOOP ( 'NONE', ( #119677, #12354 ) ) ;
#96772 = DIRECTION ( 'NONE',  ( -0.000000000000000000, 1.000000000000000000, -0.000000000000000000 ) ) ;
#96773 = VERTEX_POINT ( 'NONE', #6428 ) ;
#96774 = CARTESIAN_POINT ( 'NONE',  ( 1.449999999999951772, 2.500000000000000000, -6.248780366869526759 ) ) ;
#96775 = DIRECTION ( 'NONE',  ( 0.000000000000000000, 0.000000000000000000, 1.000000000000000000 ) ) ;
#96776 = FACE_OUTER_BOUND ( 'NONE', #35358, .T. ) ;
#96777 = CONICAL_SURFACE ( 'NONE', #15202, 0.1000000000000002554, 0.003490658503988666988 ) ;
#96778 = CARTESIAN_POINT ( 'NONE',  ( -8.950000000000008171, 2.500000000000000000, -2.511473670974877948 ) ) ;
#96779 = DIRECTION ( 'NONE',  ( -4.274815082592931898E-19, -0.9999939076577903929, -0.003490651415223739937 ) ) ;
#96780 = VERTEX_POINT ( 'NONE', #106594 ) ;
#96782 = VERTEX_POINT ( 'NONE', #86957 ) ;
#96781 = EDGE_CURVE ( 'NONE', #95522, #76489, #3478, .T. ) ;
#96783 = CARTESIAN_POINT ( 'NONE',  ( -14.14999999999998614, 12.50000000000000000, -2.922977105672689202 ) ) ;
#96784 = AXIS2_PLACEMENT_3D ( 'NONE', #74497, #114411, #24756 ) ;
#96785 = CIRCLE ( 'NONE', #86321, 0.1000000000000000472 ) ;
#96786 = FACE_OUTER_BOUND ( 'NONE', #3448, .T. ) ;
#96788 = DIRECTION ( 'NONE',  ( 0.000000000000000000, 1.000000000000000000, 0.000000000000000000 ) ) ;
#96787 = VECTOR ( 'NONE', #103768, 1000.000000000000000 ) ;
#96790 = ORIENTED_EDGE ( 'NONE', *, *, #116162, .F. ) ;
#96789 = ORIENTED_EDGE ( 'NONE', *, *, #99642, .F. ) ;
#96791 = ORIENTED_EDGE ( 'NONE', *, *, #19780, .F. ) ;
#96792 = DIRECTION ( 'NONE',  ( 0.000000000000000000, 0.000000000000000000, 1.000000000000000000 ) ) ;
#96794 = ADVANCED_FACE ( 'NONE', ( #126894 ), #43208, .T. ) ;
#96793 = CARTESIAN_POINT ( 'NONE',  ( 9.349999999999916156, 2.500000000000000000, -2.511473670974877948 ) ) ;
#96795 = AXIS2_PLACEMENT_3D ( 'NONE', #87642, #8434, #18902 ) ;
#96797 = DIRECTION ( 'NONE',  ( 0.000000000000000000, 0.000000000000000000, 1.000000000000000000 ) ) ;
#96796 = VECTOR ( 'NONE', #45678, 1000.000000000000000 ) ;
#96798 = CONICAL_SURFACE ( 'NONE', #59273, 0.1000000000000002554, 0.003490658503988666988 ) ;
#96799 = SHAPE_DEFINITION_REPRESENTATION ( #12669, #1094 ) ;
#96800 = DIRECTION ( 'NONE',  ( 0.000000000000000000, -0.000000000000000000, 1.000000000000000000 ) ) ;
#96801 = CARTESIAN_POINT ( 'NONE',  ( 187.0416666666666572, -4.445597072760107515, 7.700000000000023270 ) ) ;
#96802 = CARTESIAN_POINT ( 'NONE',  ( -11.84999999999999609, 12.50000000000000000, 2.446380397790835826 ) ) ;
#96803 = CIRCLE ( 'NONE', #86337, 0.06509327318403745899 ) ;
#96804 = CARTESIAN_POINT ( 'NONE',  ( -3.150000000000029221, 12.50000000000000000, 2.446380397790835826 ) ) ;
#96805 = CARTESIAN_POINT ( 'NONE',  ( 11.04999999999990834, 2.500000000000000000, 1.918653347947321564 ) ) ;
#96806 = CIRCLE ( 'NONE', #119797, 0.06509327318403745899 ) ;
#96807 = EDGE_CURVE ( 'NONE', #40175, #25430, #114202, .T. ) ;
#96808 = ADVANCED_FACE ( 'NONE', ( #118998 ), #109160, .T. ) ;
#96809 = CARTESIAN_POINT ( 'NONE',  ( 3.349999999999945466, 2.500000000000000000, -6.495190528383302464 ) ) ;
#96810 = AXIS2_PLACEMENT_3D ( 'NONE', #7972, #25681, #18445 ) ;
#96811 = EDGE_LOOP ( 'NONE', ( #106161, #13619 ) ) ;
#96812 = EDGE_CURVE ( 'NONE', #106895, #82230, #105880, .T. ) ;
#96813 = CARTESIAN_POINT ( 'NONE',  ( 2.299999999999949640, 2.500000000000000000, -0.2464101615137782308 ) ) ;
#96814 = ORIENTED_EDGE ( 'NONE', *, *, #67428, .F. ) ;
#96815 = VERTEX_POINT ( 'NONE', #100011 ) ;
#96816 = EDGE_CURVE ( 'NONE', #58787, #2492, #122617, .T. ) ;
#96817 = DIRECTION ( 'NONE',  ( 0.000000000000000000, 1.000000000000000000, 0.000000000000000000 ) ) ;
#96818 = LINE ( 'NONE', #69284, #80375 ) ;
#96819 = CARTESIAN_POINT ( 'NONE',  ( 3.349999999999945466, 2.500000000000000000, -2.265063509461101798 ) ) ;
#96820 = CIRCLE ( 'NONE', #111494, 0.06509327318403745899 ) ;
#96821 = FACE_OUTER_BOUND ( 'NONE', #83210, .T. ) ;
#96822 = DIRECTION ( 'NONE',  ( 0.000000000000000000, 0.000000000000000000, 1.000000000000000000 ) ) ;
#96823 = FACE_OUTER_BOUND ( 'NONE', #41109, .T. ) ;
#96824 = CARTESIAN_POINT ( 'NONE',  ( 12.89999999999989733, 12.50000000000000000, -2.385244779468109755E-15 ) ) ;
#96825 = ORIENTED_EDGE ( 'NONE', *, *, #60815, .F. ) ;
#96826 = CARTESIAN_POINT ( 'NONE',  ( 14.79999999999989413, 2.500000000000000000, -0.3464101615137782364 ) ) ;
#96828 = VECTOR ( 'NONE', #32396, 1000.000000000000000 ) ;
#96827 = DIRECTION ( 'NONE',  ( 0.000000000000000000, 0.000000000000000000, -1.000000000000000000 ) ) ;
#96829 = EDGE_LOOP ( 'NONE', ( #31521, #81436, #29408, #58043 ) ) ;
#96830 = AXIS2_PLACEMENT_3D ( 'NONE', #71783, #1095, #32520 ) ;
#96831 = ORIENTED_EDGE ( 'NONE', *, *, #88885, .T. ) ;
#96832 = VERTEX_POINT ( 'NONE', #59466 ) ;
#96833 = EDGE_LOOP ( 'NONE', ( #108401, #74700 ) ) ;
#96834 = EDGE_LOOP ( 'NONE', ( #41919, #8958 ) ) ;
#96835 = CONICAL_SURFACE ( 'NONE', #78175, 0.09999999999999999167, 0.003490658503988666988 ) ;
#96836 = CARTESIAN_POINT ( 'NONE',  ( 8.299999999999922551, 2.500000000000000000, -4.230127018922201998 ) ) ;
#96837 = PLANE ( 'NONE',  #45685 ) ;
#96838 = AXIS2_PLACEMENT_3D ( 'NONE', #63987, #6967, #84912 ) ;
#96839 = CIRCLE ( 'NONE', #126086, 0.1000000000000000472 ) ;
#96840 = ORIENTED_EDGE ( 'NONE', *, *, #30723, .F. ) ;
#96841 = CARTESIAN_POINT ( 'NONE',  ( 5.849999999999934808, 2.500000000000000000, -5.902370205355750521 ) ) ;
#96842 = CIRCLE ( 'NONE', #119840, 0.09999999999999982514 ) ;
#96843 = CARTESIAN_POINT ( 'NONE',  ( -7.900000000000014566, 12.50000000000000000, -4.395220292106239768 ) ) ;
#96844 = DIRECTION ( 'NONE',  ( 1.000000000000000000, -0.000000000000000000, -0.000000000000000000 ) ) ;
#96845 = ORIENTED_EDGE ( 'NONE', *, *, #110020, .F. ) ;
#96846 = DIRECTION ( 'NONE',  ( 0.000000000000000000, 0.000000000000000000, -1.000000000000000000 ) ) ;
#96847 = EDGE_CURVE ( 'NONE', #13639, #124646, #20209, .T. ) ;
#96848 = DIRECTION ( 'NONE',  ( 0.000000000000000000, 1.000000000000000000, 0.000000000000000000 ) ) ;
#96849 = ORIENTED_EDGE ( 'NONE', *, *, #118708, .F. ) ;
#96850 = CONICAL_SURFACE ( 'NONE', #40450, 0.1000000000000000472, 0.003490658503988666988 ) ;
#96851 = AXIS2_PLACEMENT_3D ( 'NONE', #29708, #69628, #50016 ) ;
#96852 = AXIS2_PLACEMENT_3D ( 'NONE', #69918, #119014, #37248 ) ;
#96853 = ORIENTED_EDGE ( 'NONE', *, *, #33068, .F. ) ;
#96854 = EDGE_LOOP ( 'NONE', ( #44928, #86106, #28158, #38776 ) ) ;
#96855 = CARTESIAN_POINT ( 'NONE',  ( 8.949999999999921130, 2.500000000000000000, -6.841600689897078702 ) ) ;
#96856 = EDGE_CURVE ( 'NONE', #96782, #100782, #116330, .T. ) ;
#96857 = AXIS2_PLACEMENT_3D ( 'NONE', #27210, #35752, #75657 ) ;
#96858 = EDGE_CURVE ( 'NONE', #9937, #79720, #110003, .T. ) ;
#96859 = ADVANCED_FACE ( 'NONE', ( #97418 ), #40461, .T. ) ;
#96860 = DIRECTION ( 'NONE',  ( 0.000000000000000000, 1.000000000000000000, 0.000000000000000000 ) ) ;
#96861 = EDGE_CURVE ( 'NONE', #95073, #16529, #32745, .T. ) ;
#96862 = VERTEX_POINT ( 'NONE', #118349 ) ;
#96863 = CARTESIAN_POINT ( 'NONE',  ( -3.950000000000028155, 2.500000000000000000, -6.841600689897077814 ) ) ;
#96864 = DIRECTION ( 'NONE',  ( -4.274815082592931898E-19, -0.9999939076577903929, -0.003490651415223739937 ) ) ;
#96865 = DIRECTION ( 'NONE',  ( 0.000000000000000000, 0.000000000000000000, -1.000000000000000000 ) ) ;
#96866 = DIRECTION ( 'NONE',  ( -0.000000000000000000, -1.000000000000000000, -0.000000000000000000 ) ) ;
#96867 = EDGE_CURVE ( 'NONE', #98786, #46014, #49471, .T. ) ;
#96868 = ORIENTED_EDGE ( 'NONE', *, *, #126017, .T. ) ;
#96869 = ADVANCED_FACE ( 'NONE', ( #29990 ), #87004, .T. ) ;
#96870 = DIRECTION ( 'NONE',  ( 0.000000000000000000, 0.000000000000000000, -1.000000000000000000 ) ) ;
#96871 = EDGE_LOOP ( 'NONE', ( #86167, #48507 ) ) ;
#96872 = EDGE_LOOP ( 'NONE', ( #24637, #128405, #121358, #51453 ) ) ;
#96873 = CONICAL_SURFACE ( 'NONE', #113610, 0.09999999999999982514, 0.003490658503988666988 ) ;
#96874 = VERTEX_POINT ( 'NONE', #79090 ) ;
#96875 = AXIS2_PLACEMENT_3D ( 'NONE', #656, #52993, #101447 ) ;
#96876 = FACE_OUTER_BOUND ( 'NONE', #104093, .T. ) ;
#96877 = FACE_BOUND ( 'NONE', #100809, .T. ) ;
#96878 = DIRECTION ( 'NONE',  ( 0.000000000000000000, 0.000000000000000000, 1.000000000000000000 ) ) ;
#96879 = LINE ( 'NONE', #117798, #96655 ) ;
#96880 = DIRECTION ( 'NONE',  ( -0.000000000000000000, 1.000000000000000000, -0.000000000000000000 ) ) ;
#96881 = VECTOR ( 'NONE', #28472, 1000.000000000000000 ) ;
#96882 = AXIS2_PLACEMENT_3D ( 'NONE', #98274, #87804, #127745 ) ;
#96883 = CONICAL_SURFACE ( 'NONE', #52983, 0.1000000000000002554, 0.003490658503988666988 ) ;
#96884 = AXIS2_PLACEMENT_3D ( 'NONE', #45624, #94700, #36454 ) ;
#96885 = AXIS2_PLACEMENT_3D ( 'NONE', #20544, #120677, #31649 ) ;
#96886 = ORIENTED_EDGE ( 'NONE', *, *, #11487, .T. ) ;
#96887 = DIRECTION ( 'NONE',  ( 0.000000000000000000, 1.000000000000000000, 0.000000000000000000 ) ) ;
#96888 = DIRECTION ( 'NONE',  ( 0.000000000000000000, 0.000000000000000000, -1.000000000000000000 ) ) ;
#96889 = EDGE_CURVE ( 'NONE', #47981, #64551, #7746, .T. ) ;
#96890 = CARTESIAN_POINT ( 'NONE',  ( -8.750000000000010658, 12.50000000000000000, 2.922977105672686982 ) ) ;
#96891 = LINE ( 'NONE', #45230, #82378 ) ;
#96892 = ORIENTED_EDGE ( 'NONE', *, *, #82414, .T. ) ;
#96894 = CARTESIAN_POINT ( 'NONE',  ( -0.8500000000000386136, 12.50000000000000000, 2.792790559304612064 ) ) ;
#96893 = AXIS2_PLACEMENT_3D ( 'NONE', #50493, #41976, #2667 ) ;
#96895 = CIRCLE ( 'NONE', #25803, 0.06509327318403745899 ) ;
#96896 = CIRCLE ( 'NONE', #44685, 0.06509327318403745899 ) ;
#96897 = CARTESIAN_POINT ( 'NONE',  ( -5.850000000000019185, 2.500000000000000000, 2.165063509461097713 ) ) ;
#96898 = EDGE_LOOP ( 'NONE', ( #117473, #61644 ) ) ;
#96899 = VECTOR ( 'NONE', #75258, 1000.000000000000000 ) ;
#96900 = DIRECTION ( 'NONE',  ( -0.000000000000000000, 1.000000000000000000, -0.000000000000000000 ) ) ;
#96901 = DIRECTION ( 'NONE',  ( -0.000000000000000000, 1.000000000000000000, -0.000000000000000000 ) ) ;
#96902 = FACE_BOUND ( 'NONE', #5283, .T. ) ;
#96903 = CARTESIAN_POINT ( 'NONE',  ( -6.050000000000022027, 2.500000000000000000, -1.918653347947326004 ) ) ;
#96904 = ORIENTED_EDGE ( 'NONE', *, *, #25524, .F. ) ;
#96905 = DIRECTION ( 'NONE',  ( 0.000000000000000000, -0.9999939076577903929, 0.003490651415223739937 ) ) ;
#96906 = ORIENTED_EDGE ( 'NONE', *, *, #116910, .T. ) ;
#96907 = ORIENTED_EDGE ( 'NONE', *, *, #11734, .T. ) ;
#96908 = CARTESIAN_POINT ( 'NONE',  ( 17.91370874550468884, 0.4812889678260186543, -4.985910759330088204 ) ) ;
#96909 = CARTESIAN_POINT ( 'NONE',  ( 184.5052083336747444, -6.551208109652278289, 3.782341765624995134 ) ) ;
#96911 = ORIENTED_EDGE ( 'NONE', *, *, #89063, .T. ) ;
#96910 = VECTOR ( 'NONE', #93676, 1000.000000000000000 ) ;
#96912 = CARTESIAN_POINT ( 'NONE',  ( 186.0468750003414300, -8.734944146203032389, -1.604583208406767949E-15 ) ) ;
#96913 = FACE_OUTER_BOUND ( 'NONE', #56625, .T. ) ;
#96914 = EDGE_CURVE ( 'NONE', #76856, #34681, #15978, .T. ) ;
#96915 = DIRECTION ( 'NONE',  ( 0.000000000000000000, -0.000000000000000000, 1.000000000000000000 ) ) ;
#96916 = DIRECTION ( 'NONE',  ( 0.000000000000000000, 1.000000000000000000, 0.000000000000000000 ) ) ;
#96917 = CIRCLE ( 'NONE', #67673, 0.1000000000000002554 ) ;
#96918 = CONICAL_SURFACE ( 'NONE', #71910, 0.09999999999999999167, 0.003490658503988666988 ) ;
#96919 = VECTOR ( 'NONE', #25233, 1000.000000000000000 ) ;
#96920 = ORIENTED_EDGE ( 'NONE', *, *, #53892, .F. ) ;
#96921 = FACE_OUTER_BOUND ( 'NONE', #100847, .T. ) ;
#96922 = LINE ( 'NONE', #87103, #106142 ) ;
#96923 = FACE_OUTER_BOUND ( 'NONE', #86746, .T. ) ;
#96924 = CARTESIAN_POINT ( 'NONE',  ( -8.350000000000013856, 2.500000000000000000, -5.702370205355745014 ) ) ;
#96925 = ORIENTED_EDGE ( 'NONE', *, *, #58871, .F. ) ;
#96926 = CARTESIAN_POINT ( 'NONE',  ( -10.00000000000000355, 2.500000000000000000, 3.637306695894644726 ) ) ;
#96927 = VERTEX_POINT ( 'NONE', #108535 ) ;
#96928 = VECTOR ( 'NONE', #52158, 1000.000000000000000 ) ;
#96929 = CARTESIAN_POINT ( 'NONE',  ( 1.249999999999953815, 12.50000000000000000, -2.857883832488653741 ) ) ;
#96930 = DIRECTION ( 'NONE',  ( 0.000000000000000000, 0.000000000000000000, 1.000000000000000000 ) ) ;
#96931 = VECTOR ( 'NONE', #122119, 1000.000000000000000 ) ;
#96932 = ORIENTED_EDGE ( 'NONE', *, *, #125927, .F. ) ;
#96934 = CARTESIAN_POINT ( 'NONE',  ( 13.94999999999989626, 2.500000000000000000, 2.511473670974873507 ) ) ;
#96933 = VECTOR ( 'NONE', #123998, 1000.000000000000000 ) ;
#96935 = PLANE ( 'NONE',  #39043 ) ;
#96936 = FACE_OUTER_BOUND ( 'NONE', #112281, .T. ) ;
#96937 = DIRECTION ( 'NONE',  ( 0.000000000000000000, 1.000000000000000000, 0.000000000000000000 ) ) ;
#96938 = EDGE_LOOP ( 'NONE', ( #6292, #24130 ) ) ;
#96939 = CARTESIAN_POINT ( 'NONE',  ( -2.900000000000030109, 2.500000000000000000, 0.6928203230275494784 ) ) ;
#96940 = DIRECTION ( 'NONE',  ( 0.000000000000000000, -0.9999939076577903929, 0.003490651415223739937 ) ) ;
#96941 = DIRECTION ( 'NONE',  ( 0.000000000000000000, 1.000000000000000000, 0.000000000000000000 ) ) ;
#96942 = CARTESIAN_POINT ( 'NONE',  ( 8.749999999999920064, 12.50000000000000000, 5.802370205355744659 ) ) ;
#96943 = AXIS2_PLACEMENT_3D ( 'NONE', #118197, #79568, #128698 ) ;
#96944 = CARTESIAN_POINT ( 'NONE',  ( 139.9358549477330200, 2.500000000000000000, -3.576063159858998475 ) ) ;
#96945 = ORIENTED_EDGE ( 'NONE', *, *, #113217, .F. ) ;
#96946 = VERTEX_POINT ( 'NONE', #128186 ) ;
#96947 = CARTESIAN_POINT ( 'NONE',  ( 175.5000000000000000, 0.000000000000000000, 0.000000000000000000 ) ) ;
#96949 = ORIENTED_EDGE ( 'NONE', *, *, #108531, .T. ) ;
#96948 = CIRCLE ( 'NONE', #122100, 0.1000000000000002554 ) ;
#96950 = AXIS2_PLACEMENT_3D ( 'NONE', #61101, #41489, #121309 ) ;
#96951 = CIRCLE ( 'NONE', #23806, 0.1000000000000000472 ) ;
#96952 = CARTESIAN_POINT ( 'NONE',  ( 7.699999999999925571, 2.500000000000000000, -4.776537180435978414 ) ) ;
#96954 = ORIENTED_EDGE ( 'NONE', *, *, #81640, .T. ) ;
#96953 = VERTEX_POINT ( 'NONE', #70539 ) ;
#96955 = EDGE_LOOP ( 'NONE', ( #6540, #124870 ) ) ;
#96956 = AXIS2_PLACEMENT_3D ( 'NONE', #57817, #117337, #109492 ) ;
#96957 = CARTESIAN_POINT ( 'NONE',  ( -8.150000000000012790, 2.500000000000000000, 1.818653347947321475 ) ) ;
#96958 = CIRCLE ( 'NONE', #9137, 0.06509327318403745899 ) ;
#96960 = EDGE_CURVE ( 'NONE', #69282, #21419, #97474, .T. ) ;
#96959 = CARTESIAN_POINT ( 'NONE',  ( 13.94999999999989271, 2.500000000000000000, -1.918653347947326004 ) ) ;
#96961 = DIRECTION ( 'NONE',  ( 0.000000000000000000, -0.9999939076577903929, 0.003490651415223739937 ) ) ;
#96962 = CARTESIAN_POINT ( 'NONE',  ( -12.89999999999999325, 2.500000000000000000, 0.6928203230275535862 ) ) ;
#96963 = FACE_OUTER_BOUND ( 'NONE', #102551, .T. ) ;
#96964 = FACE_OUTER_BOUND ( 'NONE', #5876, .T. ) ;
#96965 = ADVANCED_FACE ( 'NONE', ( #109828 ), #30596, .T. ) ;
#96966 = ORIENTED_EDGE ( 'NONE', *, *, #47914, .T. ) ;
#96967 = ADVANCED_FACE ( 'NONE', ( #60103 ), #18856, .T. ) ;
#96968 = CARTESIAN_POINT ( 'NONE',  ( 4.599999999999939249, 2.500000000000000000, -3.637306695894650055 ) ) ;
#96969 = ORIENTED_EDGE ( 'NONE', *, *, #11695, .T. ) ;
#96970 = ORIENTED_EDGE ( 'NONE', *, *, #76594, .F. ) ;
#96971 = ORIENTED_EDGE ( 'NONE', *, *, #5373, .F. ) ;
#96972 = EDGE_LOOP ( 'NONE', ( #43950, #73377 ) ) ;
#96973 = EDGE_CURVE ( 'NONE', #65955, #4435, #88899, .T. ) ;
#96975 = EDGE_CURVE ( 'NONE', #56893, #121027, #1320, .T. ) ;
#96974 = CARTESIAN_POINT ( 'NONE',  ( -10.85000000000000142, 2.500000000000000000, -5.802370205355746435 ) ) ;
#96976 = AXIS2_PLACEMENT_3D ( 'NONE', #42425, #14219, #54171 ) ;
#96977 = CONICAL_SURFACE ( 'NONE', #115749, 0.1000000000000000056, 0.003490658503988666988 ) ;
#96979 = ORIENTED_EDGE ( 'NONE', *, *, #69841, .T. ) ;
#96978 = EDGE_CURVE ( 'NONE', #119499, #123701, #82907, .T. ) ;
#96980 = ORIENTED_EDGE ( 'NONE', *, *, #48218, .F. ) ;
#96981 = EDGE_CURVE ( 'NONE', #95501, #80857, #55698, .T. ) ;
#96983 = CARTESIAN_POINT ( 'NONE',  ( 4.599999999999938360, 2.500000000000000000, -2.276824562219559311E-15 ) ) ;
#96982 = AXIS2_PLACEMENT_3D ( 'NONE', #71604, #70964, #111534 ) ;
#96984 = VECTOR ( 'NONE', #82861, 1000.000000000000000 ) ;
#96985 = DIRECTION ( 'NONE',  ( 0.000000000000000000, 1.000000000000000000, 0.000000000000000000 ) ) ;
#96987 = CARTESIAN_POINT ( 'NONE',  ( -11.89999999999999680, 2.500000000000000000, -4.083716857408424161 ) ) ;
#96986 = AXIS2_PLACEMENT_3D ( 'NONE', #107658, #57917, #50663 ) ;
#96988 = LINE ( 'NONE', #49841, #92877 ) ;
#96989 = AXIS2_PLACEMENT_3D ( 'NONE', #60606, #42243, #80881 ) ;
#96990 = AXIS2_PLACEMENT_3D ( 'NONE', #127130, #119225, #118570 ) ;
#96991 = DIRECTION ( 'NONE',  ( 0.000000000000000000, -0.000000000000000000, 1.000000000000000000 ) ) ;
#96992 = ORIENTED_EDGE ( 'NONE', *, *, #35268, .T. ) ;
#96993 = ADVANCED_FACE ( 'NONE', ( #31282 ), #9741, .T. ) ;
#96994 = CARTESIAN_POINT ( 'NONE',  ( 8.149999999999920419, 2.500000000000000000, 6.248780366869521430 ) ) ;
#96995 = ORIENTED_EDGE ( 'NONE', *, *, #28106, .F. ) ;
#96996 = PLANE ( 'NONE',  #84028 ) ;
#96997 = CIRCLE ( 'NONE', #86528, 0.1000000000000002554 ) ;
#96998 = ORIENTED_EDGE ( 'NONE', *, *, #70120, .T. ) ;
#96999 = DIRECTION ( 'NONE',  ( 0.000000000000000000, 0.000000000000000000, -1.000000000000000000 ) ) ;
#97000 = ORIENTED_EDGE ( 'NONE', *, *, #92127, .T. ) ;
#97001 = AXIS2_PLACEMENT_3D ( 'NONE', #41167, #21499, #61444 ) ;
#97002 = ORIENTED_EDGE ( 'NONE', *, *, #19223, .T. ) ;
#97003 = CARTESIAN_POINT ( 'NONE',  ( 185.7812500006828031, 0.000000000000000000, 7.700000000000000178 ) ) ;
#97004 = PLANE ( 'NONE',  #4594 ) ;
#97005 = LINE ( 'NONE', #83501, #113544 ) ;
#97006 = DIRECTION ( 'NONE',  ( -0.000000000000000000, -1.000000000000000000, -0.000000000000000000 ) ) ;
#97007 = PLANE ( 'NONE',  #120273 ) ;
#97008 = ORIENTED_EDGE ( 'NONE', *, *, #57355, .F. ) ;
#97009 = LINE ( 'NONE', #19071, #62431 ) ;
#97010 = CARTESIAN_POINT ( 'NONE',  ( -4.550000000000022915, 12.50000000000000000, -2.165063509461101710 ) ) ;
#97011 = ADVANCED_FACE ( 'NONE', ( #3104 ), #64026, .T. ) ;
#97012 = DIRECTION ( 'NONE',  ( 0.000000000000000000, 0.000000000000000000, 1.000000000000000000 ) ) ;
#97013 = DIRECTION ( 'NONE',  ( 0.000000000000000000, 0.000000000000000000, 1.000000000000000000 ) ) ;
#97014 = AXIS2_PLACEMENT_3D ( 'NONE', #35825, #78342, #58053 ) ;
#97015 = CARTESIAN_POINT ( 'NONE',  ( -7.300000000000016698, 2.500000000000000000, -4.676537180435978769 ) ) ;
#97016 = ORIENTED_EDGE ( 'NONE', *, *, #44435, .F. ) ;
#97017 = VERTEX_POINT ( 'NONE', #113040 ) ;
#97018 = ADVANCED_FACE ( 'NONE', ( #31916 ), #21438, .T. ) ;
#97019 = PLANE ( 'NONE',  #54799 ) ;
#97020 = ADVANCED_FACE ( 'NONE', ( #73750 ), #80764, .T. ) ;
#97021 = EDGE_CURVE ( 'NONE', #105515, #42013, #82953, .T. ) ;
#97022 = ORIENTED_EDGE ( 'NONE', *, *, #91887, .T. ) ;
#97023 = CONICAL_SURFACE ( 'NONE', #69837, 0.1000000000000002554, 0.003490658503988666988 ) ;
#97024 = CARTESIAN_POINT ( 'NONE',  ( 4.349999999999936584, 12.50000000000000000, 6.213873640053558134 ) ) ;
#97025 = DIRECTION ( 'NONE',  ( 0.000000000000000000, -0.9999939076577903929, 0.003490651415223739937 ) ) ;
#97026 = EDGE_CURVE ( 'NONE', #9406, #26024, #7575, .T. ) ;
#97027 = EDGE_CURVE ( 'NONE', #19044, #111256, #18039, .T. ) ;
#97028 = ORIENTED_EDGE ( 'NONE', *, *, #73953, .F. ) ;
#97029 = CARTESIAN_POINT ( 'NONE',  ( 186.1666666666666856, -6.668395609140176816, -3.850000000000003642 ) ) ;
#97030 = DIRECTION ( 'NONE',  ( 0.000000000000000000, 1.000000000000000000, 0.000000000000000000 ) ) ;
#97031 = DIRECTION ( 'NONE',  ( 0.000000000000000000, 0.000000000000000000, 1.000000000000000000 ) ) ;
#97032 = EDGE_CURVE ( 'NONE', #37015, #114052, #51514, .T. ) ;
#97033 = PLANE ( 'NONE',  #64947 ) ;
#97034 = DIRECTION ( 'NONE',  ( 0.000000000000000000, -0.9999939076577903929, 0.003490651415223739937 ) ) ;
#97035 = ORIENTED_EDGE ( 'NONE', *, *, #91846, .F. ) ;
#97036 = EDGE_CURVE ( 'NONE', #126646, #65379, #124672, .T. ) ;
#97037 = ADVANCED_FACE ( 'NONE', ( #93409 ), #13932, .T. ) ;
#97038 = CIRCLE ( 'NONE', #115898, 0.06509327318403745899 ) ;
#97039 = EDGE_CURVE ( 'NONE', #100363, #124, #28524, .T. ) ;
#97040 = CARTESIAN_POINT ( 'NONE',  ( -10.65000000000000391, 2.500000000000000000, -6.741600689897074616 ) ) ;
#97041 = CARTESIAN_POINT ( 'NONE',  ( 11.24999999999990941, 12.50000000000000000, 7.188010851410848723 ) ) ;
#97042 = ORIENTED_EDGE ( 'NONE', *, *, #39582, .T. ) ;
#97043 = CARTESIAN_POINT ( 'NONE',  ( 3.749999999999942268, 12.50000000000000000, -5.867463478539787225 ) ) ;
#97044 = DIRECTION ( 'NONE',  ( 0.000000000000000000, 0.000000000000000000, 1.000000000000000000 ) ) ;
#97045 = EDGE_CURVE ( 'NONE', #54254, #95676, #120549, .T. ) ;
#97046 = CARTESIAN_POINT ( 'NONE',  ( -15.79999999999998117, 12.50000000000000000, 0.000000000000000000 ) ) ;
#97047 = ORIENTED_EDGE ( 'NONE', *, *, #31422, .T. ) ;
#97048 = AXIS2_PLACEMENT_3D ( 'NONE', #5284, #105441, #103506 ) ;
#97049 = AXIS2_PLACEMENT_3D ( 'NONE', #32211, #121850, #102224 ) ;
#97050 = DIRECTION ( 'NONE',  ( 0.000000000000000000, 1.224646799147355426E-16, 1.000000000000000000 ) ) ;
#97052 = VERTEX_POINT ( 'NONE', #102569 ) ;
#97051 = CIRCLE ( 'NONE', #40651, 0.06509327318403745899 ) ;
#97053 = DIRECTION ( 'NONE',  ( 0.000000000000000000, -0.000000000000000000, 1.000000000000000000 ) ) ;
#97054 = CARTESIAN_POINT ( 'NONE',  ( 16.55874544816229132, -0.4845305829427751232, 6.091953208798936537 ) ) ;
#97055 = DIRECTION ( 'NONE',  ( -0.000000000000000000, -1.000000000000000000, -0.000000000000000000 ) ) ;
#97056 = CONICAL_SURFACE ( 'NONE', #7157, 0.09999999999999982514, 0.003490658503988666988 ) ;
#97057 = ORIENTED_EDGE ( 'NONE', *, *, #77601, .T. ) ;
#97058 = CARTESIAN_POINT ( 'NONE',  ( -8.350000000000012079, 2.500000000000000000, -2.857883832488653741 ) ) ;
#97059 = DIRECTION ( 'NONE',  ( 0.000000000000000000, 0.000000000000000000, 1.000000000000000000 ) ) ;
#97060 = ORIENTED_EDGE ( 'NONE', *, *, #81738, .T. ) ;
#97061 = DIRECTION ( 'NONE',  ( 0.000000000000000000, 0.000000000000000000, 1.000000000000000000 ) ) ;
#97062 = EDGE_LOOP ( 'NONE', ( #30156, #115109 ) ) ;
#97063 = CARTESIAN_POINT ( 'NONE',  ( 129.5000000000000000, 0.6250000000000000000, 7.634788798650556707 ) ) ;
#97064 = VERTEX_POINT ( 'NONE', #92106 ) ;
#97065 = CARTESIAN_POINT ( 'NONE',  ( 11.84999999999990727, 2.500000000000000000, -2.411473670974877859 ) ) ;
#97066 = CARTESIAN_POINT ( 'NONE',  ( 5.199999999999933564, 2.500000000000000000, 4.083716857408420609 ) ) ;
#97067 = AXIS2_PLACEMENT_3D ( 'NONE', #8910, #109717, #120176 ) ;
#97068 = AXIS2_PLACEMENT_3D ( 'NONE', #77139, #96760, #88896 ) ;
#97069 = VERTEX_POINT ( 'NONE', #12886 ) ;
#97070 = EDGE_LOOP ( 'NONE', ( #8936, #57996 ) ) ;
#97071 = DIRECTION ( 'NONE',  ( 0.000000000000000000, 1.000000000000000000, 0.000000000000000000 ) ) ;
#97072 = DIRECTION ( 'NONE',  ( -0.000000000000000000, 1.000000000000000000, -0.000000000000000000 ) ) ;
#97073 = VERTEX_POINT ( 'NONE', #42382 ) ;
#97074 = DIRECTION ( 'NONE',  ( -0.000000000000000000, -1.000000000000000000, -0.000000000000000000 ) ) ;
#97076 = CARTESIAN_POINT ( 'NONE',  ( 0.000000000000000000, 0.000000000000000000, 6.000000000000005329 ) ) ;
#97075 = CIRCLE ( 'NONE', #933, 0.09999999999999982514 ) ;
#97077 = CIRCLE ( 'NONE', #32361, 0.06509327318403745899 ) ;
#97078 = EDGE_CURVE ( 'NONE', #39808, #106452, #80852, .T. ) ;
#97079 = CIRCLE ( 'NONE', #128498, 0.09999999999999982514 ) ;
#97080 = LINE ( 'NONE', #7391, #20041 ) ;
#97081 = CARTESIAN_POINT ( 'NONE',  ( 11.44999999999991047, 2.500000000000000000, 6.248780366869520542 ) ) ;
#97082 = CARTESIAN_POINT ( 'NONE',  ( 11.64999999999990266, 2.500000000000000000, 2.265063509461097357 ) ) ;
#97083 = CARTESIAN_POINT ( 'NONE',  ( -9.400000000000009237, 12.50000000000000000, -3.983716857408421852 ) ) ;
#97084 = CIRCLE ( 'NONE', #111673, 0.09999999999999999167 ) ;
#97085 = CIRCLE ( 'NONE', #63653, 0.1000000000000000472 ) ;
#97086 = ORIENTED_EDGE ( 'NONE', *, *, #7640, .F. ) ;
#97087 = VERTEX_POINT ( 'NONE', #72492 ) ;
#97088 = VERTEX_POINT ( 'NONE', #123499 ) ;
#97089 = ORIENTED_EDGE ( 'NONE', *, *, #4058, .F. ) ;
#97090 = DIRECTION ( 'NONE',  ( -0.000000000000000000, -1.000000000000000000, -0.000000000000000000 ) ) ;
#97091 = CARTESIAN_POINT ( 'NONE',  ( -11.84999999999999609, 12.50000000000000000, 2.511473670974873507 ) ) ;
#97092 = AXIS2_PLACEMENT_3D ( 'NONE', #88116, #65274, #115666 ) ;
#97093 = CARTESIAN_POINT ( 'NONE',  ( -14.59999999999998366, 12.50000000000000000, 0.06509327318403732021 ) ) ;
#97094 = VERTEX_POINT ( 'NONE', #33837 ) ;
#97095 = EDGE_CURVE ( 'NONE', #50837, #77356, #68313, .T. ) ;
#97096 = FACE_BOUND ( 'NONE', #114559, .T. ) ;
#97097 = DIRECTION ( 'NONE',  ( 0.000000000000000000, -0.9999939076577903929, 0.003490651415223739937 ) ) ;
#97098 = DIRECTION ( 'NONE',  ( 0.000000000000000000, 1.000000000000000000, 0.000000000000000000 ) ) ;
#97099 = CARTESIAN_POINT ( 'NONE',  ( 1.449999999999952216, 12.50000000000000000, 1.818653347947321475 ) ) ;
#97100 = CARTESIAN_POINT ( 'NONE',  ( -2.050000000000033129, 12.50000000000000000, 6.430097255199259010 ) ) ;
#97101 = CARTESIAN_POINT ( 'NONE',  ( 14.54999999999989591, 2.500000000000000000, 2.165063509461097713 ) ) ;
#97102 = DIRECTION ( 'NONE',  ( -0.000000000000000000, 1.000000000000000000, -0.000000000000000000 ) ) ;
#97103 = DIRECTION ( 'NONE',  ( 0.000000000000000000, -0.000000000000000000, 1.000000000000000000 ) ) ;
#97104 = DIRECTION ( 'NONE',  ( 0.000000000000000000, 0.000000000000000000, -1.000000000000000000 ) ) ;
#97105 = DIRECTION ( 'NONE',  ( 0.000000000000000000, -0.9999939076577903929, 0.003490651415223739937 ) ) ;
#97106 = AXIS2_PLACEMENT_3D ( 'NONE', #37539, #117335, #106897 ) ;
#97107 = DIRECTION ( 'NONE',  ( 0.000000000000000000, -0.000000000000000000, 1.000000000000000000 ) ) ;
#97108 = EDGE_LOOP ( 'NONE', ( #51349, #39528 ) ) ;
#97109 = ORIENTED_EDGE ( 'NONE', *, *, #76209, .T. ) ;
#97110 = EDGE_LOOP ( 'NONE', ( #128290, #19482 ) ) ;
#97111 = VERTEX_POINT ( 'NONE', #16752 ) ;
#97112 = CARTESIAN_POINT ( 'NONE',  ( 10.19999999999991047, 12.50000000000000000, -3.983716857408426293 ) ) ;
#97113 = CARTESIAN_POINT ( 'NONE',  ( -14.19999999999998685, 2.500000000000000000, -1.084202172485504434E-16 ) ) ;
#97115 = ORIENTED_EDGE ( 'NONE', *, *, #50620, .T. ) ;
#97114 = EDGE_LOOP ( 'NONE', ( #78899, #93127 ) ) ;
#97116 = ORIENTED_EDGE ( 'NONE', *, *, #117678, .T. ) ;
#97117 = DIRECTION ( 'NONE',  ( 0.000000000000000000, 1.000000000000000000, 0.000000000000000000 ) ) ;
#97118 = AXIS2_PLACEMENT_3D ( 'NONE', #85502, #4991, #37062 ) ;
#97119 = VECTOR ( 'NONE', #13002, 1000.000000000000000 ) ;
#97120 = EDGE_CURVE ( 'NONE', #99960, #38921, #64109, .T. ) ;
#97121 = CARTESIAN_POINT ( 'NONE',  ( 4.849235612605155232, -2.500000000000000888, 8.943930330503281567 ) ) ;
#97122 = CARTESIAN_POINT ( 'NONE',  ( -3.750000000000029310, 12.50000000000000000, -7.122917578226816815 ) ) ;
#97123 = LINE ( 'NONE', #47389, #103634 ) ;
#97124 = LINE ( 'NONE', #25809, #102053 ) ;
#97125 = EDGE_LOOP ( 'NONE', ( #84617, #53475 ) ) ;
#97126 = EDGE_CURVE ( 'NONE', #102170, #77027, #57868, .T. ) ;
#97127 = CARTESIAN_POINT ( 'NONE',  ( 8.099999999999923261, 12.50000000000000000, 4.676537180435972552 ) ) ;
#97128 = ORIENTED_EDGE ( 'NONE', *, *, #87672, .T. ) ;
#97129 = AXIS2_PLACEMENT_3D ( 'NONE', #8010, #7359, #46026 ) ;
#97130 = ORIENTED_EDGE ( 'NONE', *, *, #19611, .T. ) ;
#97131 = VERTEX_POINT ( 'NONE', #56678 ) ;
#97132 = VECTOR ( 'NONE', #28189, 1000.000000000000000 ) ;
#97133 = ADVANCED_FACE ( 'NONE', ( #64583 ), #105972, .T. ) ;
#97135 = EDGE_CURVE ( 'NONE', #89102, #77185, #32829, .T. ) ;
#97134 = CARTESIAN_POINT ( 'NONE',  ( 2.899999999999944844, 2.500000000000000000, 5.122947341949749323 ) ) ;
#97137 = ORIENTED_EDGE ( 'NONE', *, *, #10675, .F. ) ;
#97136 = EDGE_CURVE ( 'NONE', #70290, #15958, #46894, .T. ) ;
#97138 = ADVANCED_FACE ( 'NONE', ( #85518 ), #37024, .T. ) ;
#97140 = ORIENTED_EDGE ( 'NONE', *, *, #58152, .F. ) ;
#97139 = EDGE_CURVE ( 'NONE', #37274, #79643, #85032, .T. ) ;
#97141 = CARTESIAN_POINT ( 'NONE',  ( -5.000000000000023093, 2.500000000000000000, 5.022947341949748790 ) ) ;
#97142 = DIRECTION ( 'NONE',  ( 0.000000000000000000, 0.000000000000000000, -1.000000000000000000 ) ) ;
#97143 = CARTESIAN_POINT ( 'NONE',  ( -3.550000000000030909, 2.500000000000000000, -6.841600689897078702 ) ) ;
#97144 = DIRECTION ( 'NONE',  ( 0.000000000000000000, 0.000000000000000000, 1.000000000000000000 ) ) ;
#97146 = AXIS2_PLACEMENT_3D ( 'NONE', #107071, #57344, #64577 ) ;
#97145 = DIRECTION ( 'NONE',  ( 0.000000000000000000, 1.000000000000000000, 0.000000000000000000 ) ) ;
#97147 = EDGE_CURVE ( 'NONE', #113918, #63903, #44963, .T. ) ;
#97148 = ORIENTED_EDGE ( 'NONE', *, *, #120225, .T. ) ;
#97149 = AXIS2_PLACEMENT_3D ( 'NONE', #97226, #8192, #118152 ) ;
#97150 = LINE ( 'NONE', #118071, #21978 ) ;
#97151 = EDGE_CURVE ( 'NONE', #37202, #64313, #49553, .T. ) ;
#97152 = EDGE_CURVE ( 'NONE', #53990, #5536, #56045, .T. ) ;
#97153 = EDGE_LOOP ( 'NONE', ( #71119, #11302 ) ) ;
#97154 = LINE ( 'NONE', #127269, #94310 ) ;
#97155 = ORIENTED_EDGE ( 'NONE', *, *, #95780, .F. ) ;
#97156 = DIRECTION ( 'NONE',  ( 0.000000000000000000, 1.000000000000000000, 0.000000000000000000 ) ) ;
#97157 = CARTESIAN_POINT ( 'NONE',  ( 21.25101288990114767, 0.2446430927199364502, -4.189229928197901742 ) ) ;
#97158 = ORIENTED_EDGE ( 'NONE', *, *, #13615, .T. ) ;
#97159 = DIRECTION ( 'NONE',  ( 0.000000000000000000, 0.000000000000000000, -1.000000000000000000 ) ) ;
#97160 = DIRECTION ( 'NONE',  ( 0.000000000000000000, 1.000000000000000000, 0.000000000000000000 ) ) ;
#97161 = ORIENTED_EDGE ( 'NONE', *, *, #60269, .T. ) ;
#97162 = CIRCLE ( 'NONE', #17721, 0.1000000000000002554 ) ;
#97163 = DIRECTION ( 'NONE',  ( -0.000000000000000000, 1.000000000000000000, -0.000000000000000000 ) ) ;
#97164 = ORIENTED_EDGE ( 'NONE', *, *, #54550, .T. ) ;
#97165 = CIRCLE ( 'NONE', #32357, 0.1000000000000002554 ) ;
#97166 = VERTEX_POINT ( 'NONE', #35153 ) ;
#97167 = CARTESIAN_POINT ( 'NONE',  ( 5.449999999999936229, 12.50000000000000000, -2.165063509461101710 ) ) ;
#97168 = LINE ( 'NONE', #7488, #1215 ) ;
#97169 = CARTESIAN_POINT ( 'NONE',  ( 185.2135416670080872, 4.367472073101518859, -7.564683531249999149 ) ) ;
#97170 = DIRECTION ( 'NONE',  ( 0.000000000000000000, -0.000000000000000000, 1.000000000000000000 ) ) ;
#97171 = AXIS2_PLACEMENT_3D ( 'NONE', #57383, #55448, #126117 ) ;
#97172 = DIRECTION ( 'NONE',  ( 0.000000000000000000, 0.000000000000000000, 1.000000000000000000 ) ) ;
#97173 = VECTOR ( 'NONE', #11121, 1000.000000000000000 ) ;
#97174 = AXIS2_PLACEMENT_3D ( 'NONE', #28416, #68326, #58531 ) ;
#97175 = CARTESIAN_POINT ( 'NONE',  ( -6.700000000000016165, 2.500000000000000000, 4.330127018922196314 ) ) ;
#97176 = AXIS2_PLACEMENT_3D ( 'NONE', #20724, #88811, #41674 ) ;
#97177 = VERTEX_POINT ( 'NONE', #14813 ) ;
#97178 = AXIS2_PLACEMENT_3D ( 'NONE', #64633, #95389, #114372 ) ;
#97179 = CARTESIAN_POINT ( 'NONE',  ( 32.27759793366435304, 1.406472199115788468, -4.686460523057745853 ) ) ;
#97181 = VECTOR ( 'NONE', #88204, 1000.000000000000000 ) ;
#97180 = CARTESIAN_POINT ( 'NONE',  ( 1.649999999999949729, 12.50000000000000000, 7.188010851410848723 ) ) ;
#97182 = VERTEX_POINT ( 'NONE', #24032 ) ;
#97183 = CONICAL_SURFACE ( 'NONE', #97092, 0.1000000000000002554, 0.003490658503988666988 ) ;
#97184 = DIRECTION ( 'NONE',  ( 0.000000000000000000, 0.000000000000000000, 1.000000000000000000 ) ) ;
#97185 = CARTESIAN_POINT ( 'NONE',  ( 8.549999999999920774, 2.500000000000000000, -2.511473670974877948 ) ) ;
#97186 = CARTESIAN_POINT ( 'NONE',  ( -12.89999999999999147, 12.50000000000000000, 4.957854068765711553 ) ) ;
#97187 = EDGE_CURVE ( 'NONE', #26124, #80887, #103831, .T. ) ;
#97188 = CARTESIAN_POINT ( 'NONE',  ( 3.949999999999939782, 12.50000000000000000, 2.446380397790835826 ) ) ;
#97189 = CARTESIAN_POINT ( 'NONE',  ( -5.000000000000024869, 12.50000000000000000, -5.022947341949754119 ) ) ;
#97190 = EDGE_LOOP ( 'NONE', ( #76500, #95843, #53496, #71616 ) ) ;
#97191 = EDGE_CURVE ( 'NONE', #109936, #81547, #62076, .T. ) ;
#97192 = ADVANCED_FACE ( 'NONE', ( #84217 ), #55802, .T. ) ;
#97193 = CARTESIAN_POINT ( 'NONE',  ( -11.84999999999999787, 2.500000000000000000, -2.411473670974874306 ) ) ;
#97194 = CARTESIAN_POINT ( 'NONE',  ( 0.8499999999999553468, 2.500000000000000000, -2.165063509461101710 ) ) ;
#97195 = AXIS2_PLACEMENT_3D ( 'NONE', #66334, #68912, #9999 ) ;
#97196 = ORIENTED_EDGE ( 'NONE', *, *, #91402, .T. ) ;
#97197 = EDGE_CURVE ( 'NONE', #73967, #49583, #16107, .T. ) ;
#97198 = LINE ( 'NONE', #8162, #46874 ) ;
#97199 = ORIENTED_EDGE ( 'NONE', *, *, #83616, .T. ) ;
#97200 = PRODUCT_DEFINITION_SHAPE ( 'NONE', 'NONE',  #61261 ) ;
#97201 = ORIENTED_EDGE ( 'NONE', *, *, #37782, .F. ) ;
#97202 = FACE_OUTER_BOUND ( 'NONE', #114178, .T. ) ;
#97204 = EDGE_CURVE ( 'NONE', #115693, #111656, #26557, .T. ) ;
#97203 = ORIENTED_EDGE ( 'NONE', *, *, #117314, .T. ) ;
#97205 = DIRECTION ( 'NONE',  ( 0.000000000000000000, 1.000000000000000000, 0.000000000000000000 ) ) ;
#97206 = DIRECTION ( 'NONE',  ( -4.274815082592931898E-19, -0.9999939076577903929, -0.003490651415223739937 ) ) ;
#97207 = DIRECTION ( 'NONE',  ( -4.274815082592931898E-19, -0.9999939076577903929, -0.003490651415223739937 ) ) ;
#97208 = VECTOR ( 'NONE', #104622, 1000.000000000000000 ) ;
#97209 = EDGE_LOOP ( 'NONE', ( #85042, #35947 ) ) ;
#97210 = FACE_BOUND ( 'NONE', #40529, .T. ) ;
#97212 = ORIENTED_EDGE ( 'NONE', *, *, #66103, .F. ) ;
#97211 = DIRECTION ( 'NONE',  ( 0.000000000000000000, 1.000000000000000000, 0.000000000000000000 ) ) ;
#97213 = DIRECTION ( 'NONE',  ( -0.000000000000000000, -1.000000000000000000, -0.000000000000000000 ) ) ;
#97214 = FACE_OUTER_BOUND ( 'NONE', #68169, .T. ) ;
#97215 = ADVANCED_FACE ( 'NONE', ( #65218 ), #3569, .T. ) ;
#97216 = VERTEX_POINT ( 'NONE', #116258 ) ;
#97217 = CIRCLE ( 'NONE', #40815, 0.1000000000000002554 ) ;
#97218 = EDGE_LOOP ( 'NONE', ( #74987, #96911 ) ) ;
#97219 = AXIS2_PLACEMENT_3D ( 'NONE', #36584, #64086, #14948 ) ;
#97220 = VERTEX_POINT ( 'NONE', #94054 ) ;
#97221 = DIRECTION ( 'NONE',  ( -0.000000000000000000, -1.000000000000000000, -0.000000000000000000 ) ) ;
#97222 = FACE_OUTER_BOUND ( 'NONE', #22679, .T. ) ;
#97223 = DIRECTION ( 'NONE',  ( -0.000000000000000000, 1.000000000000000000, -0.000000000000000000 ) ) ;
#97224 = FACE_BOUND ( 'NONE', #84125, .T. ) ;
#97225 = VERTEX_POINT ( 'NONE', #4348 ) ;
#97226 = CARTESIAN_POINT ( 'NONE',  ( 12.09999999999990550, 2.500000000000000000, 4.330127018922196314 ) ) ;
#97227 = DIRECTION ( 'NONE',  ( 0.000000000000000000, 0.000000000000000000, 1.000000000000000000 ) ) ;
#97228 = ORIENTED_EDGE ( 'NONE', *, *, #86187, .T. ) ;
#97230 = DIRECTION ( 'NONE',  ( -4.274815082592931898E-19, -0.9999939076577903929, -0.003490651415223739937 ) ) ;
#97229 = VECTOR ( 'NONE', #74219, 1000.000000000000000 ) ;
#97231 = ADVANCED_FACE ( 'NONE', ( #44299 ), #114282, .T. ) ;
#97232 = DIRECTION ( 'NONE',  ( -4.274815082592931898E-19, -0.9999939076577903929, -0.003490651415223739937 ) ) ;
#97233 = DIRECTION ( 'NONE',  ( -0.000000000000000000, -1.000000000000000000, -0.000000000000000000 ) ) ;
#97234 = DIRECTION ( 'NONE',  ( 0.000000000000000000, -0.000000000000000000, 1.000000000000000000 ) ) ;
#97235 = CARTESIAN_POINT ( 'NONE',  ( -4.200000000000025935, 2.500000000000000000, 4.330127018922196314 ) ) ;
#97236 = ORIENTED_EDGE ( 'NONE', *, *, #92145, .F. ) ;
#97237 = ORIENTED_EDGE ( 'NONE', *, *, #98744, .F. ) ;
#97238 = ORIENTED_EDGE ( 'NONE', *, *, #16180, .T. ) ;
#97239 = ORIENTED_EDGE ( 'NONE', *, *, #85771, .F. ) ;
#97240 = ORIENTED_EDGE ( 'NONE', *, *, #92669, .T. ) ;
#97241 = FACE_OUTER_BOUND ( 'NONE', #125245, .T. ) ;
#97242 = LINE ( 'NONE', #47512, #80149 ) ;
#97243 = ORIENTED_EDGE ( 'NONE', *, *, #22732, .T. ) ;
#97244 = ADVANCED_FACE ( 'NONE', ( #29828 ), #59960, .T. ) ;
#97245 = FACE_BOUND ( 'NONE', #43602, .T. ) ;
#97246 = DIRECTION ( 'NONE',  ( 0.000000000000000000, 0.000000000000000000, 1.000000000000000000 ) ) ;
#97247 = AXIS2_PLACEMENT_3D ( 'NONE', #84276, #122931, #31977 ) ;
#97248 = DIRECTION ( 'NONE',  ( 0.000000000000000000, 0.000000000000000000, 1.000000000000000000 ) ) ;
#97249 = AXIS2_PLACEMENT_3D ( 'NONE', #54649, #124705, #4253 ) ;
#97250 = AXIS2_PLACEMENT_3D ( 'NONE', #39982, #109350, #68781 ) ;
#97251 = CARTESIAN_POINT ( 'NONE',  ( -4.150000000000025224, 2.500000000000000000, 6.395190528383296602 ) ) ;
#97252 = DIRECTION ( 'NONE',  ( 0.000000000000000000, 1.000000000000000000, 0.000000000000000000 ) ) ;
#97253 = LINE ( 'NONE', #35137, #110198 ) ;
#97254 = ORIENTED_EDGE ( 'NONE', *, *, #115753, .T. ) ;
#97255 = DIRECTION ( 'NONE',  ( -0.000000000000000000, -1.000000000000000000, -0.000000000000000000 ) ) ;
#97256 = VECTOR ( 'NONE', #95066, 1000.000000000000000 ) ;
#97257 = ORIENTED_EDGE ( 'NONE', *, *, #104769, .F. ) ;
#97258 = AXIS2_PLACEMENT_3D ( 'NONE', #36801, #28256, #76710 ) ;
#97259 = ORIENTED_EDGE ( 'NONE', *, *, #54044, .F. ) ;
#97260 = ORIENTED_EDGE ( 'NONE', *, *, #111179, .T. ) ;
#97261 = DIRECTION ( 'NONE',  ( 0.000000000000000000, 0.000000000000000000, -1.000000000000000000 ) ) ;
#97262 = CIRCLE ( 'NONE', #113994, 0.06509327318403745899 ) ;
#97263 = CARTESIAN_POINT ( 'NONE',  ( -3.550000000000028688, 12.50000000000000000, 6.776507416713035248 ) ) ;
#97264 = LINE ( 'NONE', #55415, #25856 ) ;
#97265 = ORIENTED_EDGE ( 'NONE', *, *, #68206, .F. ) ;
#97266 = CARTESIAN_POINT ( 'NONE',  ( 3.677919667777222568, 2.499999999999998668, -8.999999999876376222 ) ) ;
#97267 = AXIS2_PLACEMENT_3D ( 'NONE', #49523, #29871, #40350 ) ;
#97268 = CIRCLE ( 'NONE', #32544, 0.06509327318403745899 ) ;
#97269 = DIRECTION ( 'NONE',  ( 0.000000000000000000, 1.000000000000000000, 0.000000000000000000 ) ) ;
#97270 = EDGE_CURVE ( 'NONE', #37520, #31054, #66256, .T. ) ;
#97271 = DIRECTION ( 'NONE',  ( -0.000000000000000000, 1.000000000000000000, -0.000000000000000000 ) ) ;
#97272 = CARTESIAN_POINT ( 'NONE',  ( 183.9895833340161175, -4.445597072760115509, -7.700000000000001954 ) ) ;
#97273 = PLANE ( 'NONE',  #103144 ) ;
#97275 = AXIS2_PLACEMENT_3D ( 'NONE', #114708, #106195, #101842 ) ;
#97274 = CARTESIAN_POINT ( 'NONE',  ( 129.5000000000000000, -0.6250000000000024425, -6.000000000000000000 ) ) ;
#97276 = DIRECTION ( 'NONE',  ( 0.000000000000000000, -0.9999939076577903929, 0.003490651415223739937 ) ) ;
#97277 = ORIENTED_EDGE ( 'NONE', *, *, #110931, .T. ) ;
#97278 = CARTESIAN_POINT ( 'NONE',  ( -11.64999999999999680, 2.500000000000000000, 2.857883832488649301 ) ) ;
#97279 = EDGE_CURVE ( 'NONE', #21310, #40453, #112242, .T. ) ;
#97280 = ORIENTED_EDGE ( 'NONE', *, *, #94612, .F. ) ;
#97281 = VERTEX_POINT ( 'NONE', #97910 ) ;
#97282 = DIRECTION ( 'NONE',  ( 0.000000000000000000, -0.000000000000000000, 1.000000000000000000 ) ) ;
#97283 = EDGE_CURVE ( 'NONE', #92671, #74675, #1409, .T. ) ;
#97284 = CARTESIAN_POINT ( 'NONE',  ( -10.65000000000000213, 2.500000000000000000, 6.841600689897072485 ) ) ;
#97286 = ADVANCED_FACE ( 'NONE', ( #29200 ), #117526, .T. ) ;
#97285 = CARTESIAN_POINT ( 'NONE',  ( 3.149999999999946176, 12.50000000000000000, -1.753560074763288457 ) ) ;
#97287 = EDGE_CURVE ( 'NONE', #74651, #84244, #72541, .T. ) ;
#97288 = EDGE_CURVE ( 'NONE', #109488, #29207, #76732, .T. ) ;
#97289 = AXIS2_PLACEMENT_3D ( 'NONE', #127677, #95010, #66809 ) ;
#97290 = VERTEX_POINT ( 'NONE', #10188 ) ;
#97291 = ORIENTED_EDGE ( 'NONE', *, *, #86145, .T. ) ;
#97292 = CARTESIAN_POINT ( 'NONE',  ( 11.24999999999990763, 2.500000000000000000, 1.472243186433545459 ) ) ;
#97293 = CARTESIAN_POINT ( 'NONE',  ( 11.64999999999990443, 2.500000000000000000, 2.857883832488649301 ) ) ;
#97294 = ADVANCED_FACE ( 'NONE', ( #69093 ), #27887, .T. ) ;
#97295 = CARTESIAN_POINT ( 'NONE',  ( -7.700000000000014388, 2.500000000000000000, -4.776537180435977525 ) ) ;
#97296 = ORIENTED_EDGE ( 'NONE', *, *, #27611, .F. ) ;
#97297 = ORIENTED_EDGE ( 'NONE', *, *, #123517, .T. ) ;
#97298 = ADVANCED_FACE ( 'NONE', ( #27235 ), #93455, .T. ) ;
#97299 = FACE_OUTER_BOUND ( 'NONE', #24532, .T. ) ;
#97300 = AXIS2_PLACEMENT_3D ( 'NONE', #119962, #91144, #30314 ) ;
#97301 = EDGE_CURVE ( 'NONE', #66020, #27914, #20295, .T. ) ;
#97302 = AXIS2_PLACEMENT_3D ( 'NONE', #49321, #8071, #127224 ) ;
#97303 = ORIENTED_EDGE ( 'NONE', *, *, #26542, .F. ) ;
#97305 = AXIS2_PLACEMENT_3D ( 'NONE', #14148, #56642, #86102 ) ;
#97304 = DIRECTION ( 'NONE',  ( 0.000000000000000000, -0.000000000000000000, 1.000000000000000000 ) ) ;
#97306 = EDGE_CURVE ( 'NONE', #120320, #54255, #75004, .T. ) ;
#97307 = EDGE_CURVE ( 'NONE', #30363, #98217, #18707, .T. ) ;
#97308 = CARTESIAN_POINT ( 'NONE',  ( -2.700000000000030820, 2.500000000000000000, 0.3464101615137735735 ) ) ;
#97309 = ORIENTED_EDGE ( 'NONE', *, *, #14338, .T. ) ;
#97310 = DIRECTION ( 'NONE',  ( 0.000000000000000000, 0.000000000000000000, 1.000000000000000000 ) ) ;
#97311 = DIRECTION ( 'NONE',  ( -0.000000000000000000, 1.000000000000000000, -0.000000000000000000 ) ) ;
#97312 = DIRECTION ( 'NONE',  ( 0.000000000000000000, 0.000000000000000000, 1.000000000000000000 ) ) ;
#97314 = EDGE_CURVE ( 'NONE', #45883, #50211, #24825, .T. ) ;
#97313 = DIRECTION ( 'NONE',  ( -4.274815082592931898E-19, -0.9999939076577903929, -0.003490651415223739937 ) ) ;
#97315 = ORIENTED_EDGE ( 'NONE', *, *, #43195, .F. ) ;
#97316 = AXIS2_PLACEMENT_3D ( 'NONE', #88332, #1269, #18957 ) ;
#97317 = CARTESIAN_POINT ( 'NONE',  ( 10.39999999999991154, 2.500000000000000000, 3.637306695894644726 ) ) ;
#97318 = CONICAL_SURFACE ( 'NONE', #17887, 0.1000000000000002554, 0.003490658503988666988 ) ;
#97319 = EDGE_LOOP ( 'NONE', ( #25443, #63113 ) ) ;
#97320 = ORIENTED_EDGE ( 'NONE', *, *, #123175, .T. ) ;
#97321 = FACE_OUTER_BOUND ( 'NONE', #5446, .T. ) ;
#97322 = CARTESIAN_POINT ( 'NONE',  ( 9.799999999999915445, 2.500000000000000000, 4.083716857408421497 ) ) ;
#97323 = DIRECTION ( 'NONE',  ( 0.000000000000000000, -0.9999939076577903929, 0.003490651415223739937 ) ) ;
#97324 = DIRECTION ( 'NONE',  ( -4.274815082592931898E-19, -0.9999939076577903929, -0.003490651415223739937 ) ) ;
#97325 = DIRECTION ( 'NONE',  ( 0.000000000000000000, -0.9999939076577903929, 0.003490651415223739937 ) ) ;
#97326 = DIRECTION ( 'NONE',  ( 0.000000000000000000, 1.000000000000000000, 0.000000000000000000 ) ) ;
#97327 = AXIS2_PLACEMENT_3D ( 'NONE', #3541, #33024, #2233 ) ;
#97328 = CARTESIAN_POINT ( 'NONE',  ( 17.50982738792208693, 2.500000000000000000, -4.074750937467086942 ) ) ;
#97329 = CARTESIAN_POINT ( 'NONE',  ( 6.249999999999967137, 2.500000000000000000, -2.165063509461101710 ) ) ;
#97330 = LINE ( 'NONE', #56727, #23348 ) ;
#97331 = FACE_OUTER_BOUND ( 'NONE', #127722, .T. ) ;
#97332 = VERTEX_POINT ( 'NONE', #19342 ) ;
#97333 = CARTESIAN_POINT ( 'NONE',  ( -13.09999999999999076, 2.500000000000000000, 4.083716857408421497 ) ) ;
#97334 = DIRECTION ( 'NONE',  ( -4.274815082592931898E-19, -0.9999939076577903929, -0.003490651415223739937 ) ) ;
#97335 = CARTESIAN_POINT ( 'NONE',  ( 4.149999999999941735, 2.500000000000000000, -1.472243186433550122 ) ) ;
#97336 = AXIS2_PLACEMENT_3D ( 'NONE', #126933, #119041, #97462 ) ;
#97337 = CARTESIAN_POINT ( 'NONE',  ( -2.500000000000032419, 12.50000000000000000, -3.637306695894650055 ) ) ;
#97338 = DIRECTION ( 'NONE',  ( 0.000000000000000000, 0.000000000000000000, 1.000000000000000000 ) ) ;
#97339 = VERTEX_POINT ( 'NONE', #107738 ) ;
#97340 = DIRECTION ( 'NONE',  ( 0.000000000000000000, 0.000000000000000000, 1.000000000000000000 ) ) ;
#97341 = ADVANCED_FACE ( 'NONE', ( #18057 ), #77059, .T. ) ;
#97342 = CONICAL_SURFACE ( 'NONE', #34672, 0.09999999999999982514, 0.003490658503988666988 ) ;
#97343 = CONICAL_SURFACE ( 'NONE', #116121, 0.1000000000000000472, 0.003490658503988666988 ) ;
#97344 = EDGE_CURVE ( 'NONE', #34729, #45963, #48176, .T. ) ;
#97345 = FACE_OUTER_BOUND ( 'NONE', #44786, .T. ) ;
#97347 = ORIENTED_EDGE ( 'NONE', *, *, #27347, .F. ) ;
#97346 = DIRECTION ( 'NONE',  ( 0.000000000000000000, -0.9999939076577903929, 0.003490651415223739937 ) ) ;
#97348 = ORIENTED_EDGE ( 'NONE', *, *, #45590, .T. ) ;
#97350 = ADVANCED_FACE ( 'NONE', ( #48834 ), #33157, .T. ) ;
#97349 = CONICAL_SURFACE ( 'NONE', #67816, 0.1000000000000000056, 0.003490658503988666988 ) ;
#97351 = EDGE_LOOP ( 'NONE', ( #51258, #94429, #6311, #63576 ) ) ;
#97352 = ORIENTED_EDGE ( 'NONE', *, *, #100325, .F. ) ;
#97353 = EDGE_LOOP ( 'NONE', ( #122260, #46902 ) ) ;
#97354 = DIRECTION ( 'NONE',  ( 0.000000000000000000, 0.000000000000000000, 1.000000000000000000 ) ) ;
#97355 = CARTESIAN_POINT ( 'NONE',  ( 3.749999999999975131, 12.50000000000000000, 6.495190528383297135 ) ) ;
#97356 = LINE ( 'NONE', #107165, #83866 ) ;
#97357 = VECTOR ( 'NONE', #76249, 1000.000000000000000 ) ;
#97358 = DIRECTION ( 'NONE',  ( 0.000000000000000000, 0.000000000000000000, 1.000000000000000000 ) ) ;
#97359 = CIRCLE ( 'NONE', #15878, 0.06509327318403745899 ) ;
#97360 = ORIENTED_EDGE ( 'NONE', *, *, #11465, .F. ) ;
#97361 = CIRCLE ( 'NONE', #43018, 0.1000000000000000472 ) ;
#97363 = CIRCLE ( 'NONE', #55327, 0.06509327318403745899 ) ;
#97362 = DIRECTION ( 'NONE',  ( -0.000000000000000000, -1.000000000000000000, -0.000000000000000000 ) ) ;
#97364 = VERTEX_POINT ( 'NONE', #61879 ) ;
#97365 = CARTESIAN_POINT ( 'NONE',  ( 32.27111852109496226, -3.178312372603624425, -3.140919221371700321 ) ) ;
#97366 = CARTESIAN_POINT ( 'NONE',  ( 12.30568799110296396, -2.500000000000000000, -7.490555764796996918 ) ) ;
#97367 = FACE_OUTER_BOUND ( 'NONE', #98862, .T. ) ;
#97368 = DIRECTION ( 'NONE',  ( 0.000000000000000000, 1.000000000000000000, 0.000000000000000000 ) ) ;
#97369 = CARTESIAN_POINT ( 'NONE',  ( 1.049999999999954525, 2.500000000000000000, 1.818653347947321475 ) ) ;
#97370 = ORIENTED_EDGE ( 'NONE', *, *, #16029, .F. ) ;
#97371 = EDGE_LOOP ( 'NONE', ( #6796, #117552, #15051, #3771 ) ) ;
#97372 = VERTEX_POINT ( 'NONE', #95036 ) ;
#97373 = EDGE_LOOP ( 'NONE', ( #72685, #58447, #86839, #91996 ) ) ;
#97374 = FACE_OUTER_BOUND ( 'NONE', #122893, .T. ) ;
#97375 = DIRECTION ( 'NONE',  ( 0.000000000000000000, 1.000000000000000000, 0.000000000000000000 ) ) ;
#97376 = CARTESIAN_POINT ( 'NONE',  ( -4.350000000000023626, 2.500000000000000000, -2.611473670974877592 ) ) ;
#97377 = FACE_BOUND ( 'NONE', #112748, .T. ) ;
#97378 = DIRECTION ( 'NONE',  ( -4.274815082592931898E-19, -0.9999939076577903929, -0.003490651415223739937 ) ) ;
#97379 = DIRECTION ( 'NONE',  ( 0.000000000000000000, -1.000000000000000000, 0.000000000000000000 ) ) ;
#97380 = DIRECTION ( 'NONE',  ( -4.274815082592931898E-19, -0.9999939076577903929, -0.003490651415223739937 ) ) ;
#97381 = DIRECTION ( 'NONE',  ( 0.000000000000000000, 0.000000000000000000, 1.000000000000000000 ) ) ;
#97382 = EDGE_CURVE ( 'NONE', #68683, #6418, #100049, .T. ) ;
#97383 = CARTESIAN_POINT ( 'NONE',  ( 186.1718750003414016, 9.264065473108010111E-16, -7.564683531250000925 ) ) ;
#97384 = DIRECTION ( 'NONE',  ( -0.000000000000000000, -1.000000000000000000, -0.000000000000000000 ) ) ;
#97385 = DIRECTION ( 'NONE',  ( 0.000000000000000000, 0.000000000000000000, -1.000000000000000000 ) ) ;
#97386 = CIRCLE ( 'NONE', #43047, 0.06509327318403745899 ) ;
#97387 = VECTOR ( 'NONE', #6730, 1000.000000000000000 ) ;
#97388 = DIRECTION ( 'NONE',  ( 0.000000000000000000, 0.000000000000000000, 1.000000000000000000 ) ) ;
#97389 = AXIS2_PLACEMENT_3D ( 'NONE', #49120, #109304, #51054 ) ;
#97390 = VERTEX_POINT ( 'NONE', #70395 ) ;
#97391 = EDGE_LOOP ( 'NONE', ( #28050, #128579 ) ) ;
#97392 = ORIENTED_EDGE ( 'NONE', *, *, #5105, .T. ) ;
#97393 = ORIENTED_EDGE ( 'NONE', *, *, #54347, .F. ) ;
#97394 = EDGE_CURVE ( 'NONE', #103978, #125076, #4683, .T. ) ;
#97395 = CARTESIAN_POINT ( 'NONE',  ( -8.150000000000009237, 2.500000000000000000, 6.841600689897072485 ) ) ;
#97396 = ADVANCED_FACE ( 'NONE', ( #52053 ), #20636, .T. ) ;
#97397 = FACE_BOUND ( 'NONE', #123685, .T. ) ;
#97398 = CARTESIAN_POINT ( 'NONE',  ( 11.04999999999990656, 2.500000000000000000, 2.411473670974873862 ) ) ;
#97399 = LINE ( 'NONE', #126220, #10128 ) ;
#97401 = CIRCLE ( 'NONE', #9583, 0.06509327318403745899 ) ;
#97400 = CONICAL_SURFACE ( 'NONE', #34738, 0.1000000000000002554, 0.003490658503988666988 ) ;
#97402 = ORIENTED_EDGE ( 'NONE', *, *, #125004, .T. ) ;
#97403 = DIRECTION ( 'NONE',  ( -4.274815082592931898E-19, -0.9999939076577903929, -0.003490651415223739937 ) ) ;
#97404 = EDGE_CURVE ( 'NONE', #115977, #13480, #106302, .T. ) ;
#97405 = DIRECTION ( 'NONE',  ( 0.000000000000000000, -0.000000000000000000, 1.000000000000000000 ) ) ;
#97406 = CARTESIAN_POINT ( 'NONE',  ( 165.4999999999999716, 6.123233995736767268E-17, 2.500000000000000000 ) ) ;
#97407 = ORIENTED_EDGE ( 'NONE', *, *, #18905, .T. ) ;
#97408 = CARTESIAN_POINT ( 'NONE',  ( 187.5000000000000000, 0.000000000000000000, 0.000000000000000000 ) ) ;
#97409 = DIRECTION ( 'NONE',  ( -0.000000000000000000, 1.000000000000000000, -0.000000000000000000 ) ) ;
#97410 = AXIS2_PLACEMENT_3D ( 'NONE', #2107, #23055, #81964 ) ;
#97411 = ORIENTED_EDGE ( 'NONE', *, *, #47959, .F. ) ;
#97412 = CARTESIAN_POINT ( 'NONE',  ( 6.649999999999931966, 2.500000000000000000, -5.802370205355749988 ) ) ;
#97413 = DIRECTION ( 'NONE',  ( 0.000000000000000000, -0.000000000000000000, 1.000000000000000000 ) ) ;
#97414 = ORIENTED_EDGE ( 'NONE', *, *, #31860, .F. ) ;
#97415 = CARTESIAN_POINT ( 'NONE',  ( 1.649999999999951950, 12.50000000000000000, -7.188010851410854052 ) ) ;
#97416 = PLANE ( 'NONE',  #66509 ) ;
#97417 = VERTEX_POINT ( 'NONE', #32434 ) ;
#97418 = FACE_OUTER_BOUND ( 'NONE', #68435, .T. ) ;
#97419 = ORIENTED_EDGE ( 'NONE', *, *, #22365, .F. ) ;
#97420 = ORIENTED_EDGE ( 'NONE', *, *, #44709, .F. ) ;
#97421 = CARTESIAN_POINT ( 'NONE',  ( -11.64999999999999680, 12.50000000000000000, 2.922977105672686982 ) ) ;
#97422 = VERTEX_POINT ( 'NONE', #20657 ) ;
#97423 = DIRECTION ( 'NONE',  ( 0.000000000000000000, 1.000000000000000000, 0.000000000000000000 ) ) ;
#97424 = FACE_BOUND ( 'NONE', #42522, .T. ) ;
#97425 = EDGE_CURVE ( 'NONE', #93012, #82725, #26884, .T. ) ;
#97426 = CIRCLE ( 'NONE', #82873, 0.06509327318403745899 ) ;
#97427 = ORIENTED_EDGE ( 'NONE', *, *, #76194, .T. ) ;
#97428 = AXIS2_PLACEMENT_3D ( 'NONE', #96, #78016, #97013 ) ;
#97429 = CARTESIAN_POINT ( 'NONE',  ( 112.4769073329632931, 7.370384220483499504, 2.250641841625343531 ) ) ;
#97430 = EDGE_LOOP ( 'NONE', ( #62063, #75335, #119105, #122412 ) ) ;
#97431 = DIRECTION ( 'NONE',  ( 0.000000000000000000, 0.000000000000000000, -1.000000000000000000 ) ) ;
#97432 = CARTESIAN_POINT ( 'NONE',  ( 9.999999999999912959, 12.50000000000000000, 3.637306695894644726 ) ) ;
#97433 = CARTESIAN_POINT ( 'NONE',  ( -4.550000000000022915, 2.500000000000000000, 6.495190528383297135 ) ) ;
#97435 = ADVANCED_FACE ( 'NONE', ( #91966 ), #104248, .T. ) ;
#97434 = CARTESIAN_POINT ( 'NONE',  ( 4.149999999999939959, 12.50000000000000000, -6.430097255199264339 ) ) ;
#97436 = CARTESIAN_POINT ( 'NONE',  ( 3.749999999999978684, 2.500000000000000000, -2.165063509461101710 ) ) ;
#97437 = EDGE_CURVE ( 'NONE', #106593, #85023, #12194, .T. ) ;
#97440 = VERTEX_POINT ( 'NONE', #91320 ) ;
#97439 = CONICAL_SURFACE ( 'NONE', #13801, 0.1000000000000000472, 0.003490658503988666988 ) ;
#97438 = VECTOR ( 'NONE', #116812, 1000.000000000000000 ) ;
#97441 = ORIENTED_EDGE ( 'NONE', *, *, #67031, .T. ) ;
#97442 = DIRECTION ( 'NONE',  ( 0.000000000000000000, 0.000000000000000000, 1.000000000000000000 ) ) ;
#97443 = CARTESIAN_POINT ( 'NONE',  ( 6.449999999999931788, 12.50000000000000000, -6.213873640053564351 ) ) ;
#97444 = EDGE_CURVE ( 'NONE', #113589, #61474, #37361, .T. ) ;
#97445 = CARTESIAN_POINT ( 'NONE',  ( 3.549999999999944755, 2.500000000000000000, -2.611473670974877592 ) ) ;
#97447 = VERTEX_POINT ( 'NONE', #62524 ) ;
#97446 = VERTEX_POINT ( 'NONE', #12107 ) ;
#97448 = EDGE_CURVE ( 'NONE', #55495, #19791, #16385, .T. ) ;
#97449 = ORIENTED_EDGE ( 'NONE', *, *, #24597, .F. ) ;
#97450 = ADVANCED_FACE ( 'NONE', ( #100490 ), #110505, .T. ) ;
#97451 = CARTESIAN_POINT ( 'NONE',  ( 5.849999999999933920, 2.500000000000000000, -2.165063509461101710 ) ) ;
#97453 = VECTOR ( 'NONE', #79992, 1000.000000000000000 ) ;
#97452 = AXIS2_PLACEMENT_3D ( 'NONE', #117264, #75427, #67526 ) ;
#97454 = DIRECTION ( 'NONE',  ( -0.000000000000000000, -1.000000000000000000, -0.000000000000000000 ) ) ;
#97455 = LINE ( 'NONE', #110961, #66531 ) ;
#97456 = AXIS2_PLACEMENT_3D ( 'NONE', #87776, #127712, #126442 ) ;
#97457 = ITEM_DEFINED_TRANSFORMATION ( 'NONE', 'NONE', #83365,  #108296 ) ;
#97458 = EDGE_CURVE ( 'NONE', #66944, #121198, #121416, .T. ) ;
#97459 = DIRECTION ( 'NONE',  ( 0.000000000000000000, 0.000000000000000000, -1.000000000000000000 ) ) ;
#97460 = DIRECTION ( 'NONE',  ( -0.000000000000000000, -1.000000000000000000, -0.000000000000000000 ) ) ;
#97461 = CARTESIAN_POINT ( 'NONE',  ( 15.39999999999989200, 2.500000000000000000, 0.7928203230275495672 ) ) ;
#97462 = DIRECTION ( 'NONE',  ( 0.000000000000000000, 0.000000000000000000, 1.000000000000000000 ) ) ;
#97463 = DIRECTION ( 'NONE',  ( 0.000000000000000000, -0.9999939076577903929, 0.003490651415223739937 ) ) ;
#97464 = EDGE_CURVE ( 'NONE', #129286, #118274, #64910, .T. ) ;
#97466 = EDGE_CURVE ( 'NONE', #91316, #90767, #51938, .T. ) ;
#97465 = DIRECTION ( 'NONE',  ( 0.000000000000000000, 0.000000000000000000, 1.000000000000000000 ) ) ;
#97467 = VERTEX_POINT ( 'NONE', #120142 ) ;
#97468 = ORIENTED_EDGE ( 'NONE', *, *, #17448, .T. ) ;
#97469 = CARTESIAN_POINT ( 'NONE',  ( 6.649999999999931077, 12.50000000000000000, -6.560283801567339701 ) ) ;
#97470 = VERTEX_POINT ( 'NONE', #74750 ) ;
#97471 = EDGE_LOOP ( 'NONE', ( #121239, #106894 ) ) ;
#97472 = CARTESIAN_POINT ( 'NONE',  ( 11.64999999999990266, 12.50000000000000000, -6.430097255199264339 ) ) ;
#97473 = DIRECTION ( 'NONE',  ( 0.000000000000000000, 0.000000000000000000, -1.000000000000000000 ) ) ;
#97474 = CIRCLE ( 'NONE', #39018, 0.06509327318403745899 ) ;
#97475 = CARTESIAN_POINT ( 'NONE',  ( -5.400000000000023448, 12.50000000000000000, -5.088040615133791356 ) ) ;
#97476 = CARTESIAN_POINT ( 'NONE',  ( -8.550000000000013145, 2.500000000000000000, 2.611473670974873151 ) ) ;
#97477 = DIRECTION ( 'NONE',  ( 0.000000000000000000, 1.000000000000000000, 0.000000000000000000 ) ) ;
#97478 = DIRECTION ( 'NONE',  ( 0.000000000000000000, 0.000000000000000000, 1.000000000000000000 ) ) ;
#97479 = CIRCLE ( 'NONE', #87010, 0.09999999999999982514 ) ;
#97480 = DIRECTION ( 'NONE',  ( -0.000000000000000000, -1.000000000000000000, -0.000000000000000000 ) ) ;
#97481 = VERTEX_POINT ( 'NONE', #114659 ) ;
#97482 = DIRECTION ( 'NONE',  ( 0.000000000000000000, 1.000000000000000000, 0.000000000000000000 ) ) ;
#97483 = CIRCLE ( 'NONE', #124681, 0.1000000000000002554 ) ;
#97484 = CIRCLE ( 'NONE', #28536, 0.09999999999999982514 ) ;
#97485 = VECTOR ( 'NONE', #27678, 1000.000000000000000 ) ;
#97486 = CARTESIAN_POINT ( 'NONE',  ( -10.65000000000000391, 2.500000000000000000, -2.511473670974873951 ) ) ;
#97487 = ORIENTED_EDGE ( 'NONE', *, *, #112117, .T. ) ;
#97488 = VECTOR ( 'NONE', #7066, 1000.000000000000000 ) ;
#97489 = ORIENTED_EDGE ( 'NONE', *, *, #59480, .F. ) ;
#97490 = EDGE_LOOP ( 'NONE', ( #30458, #116483, #46311, #50284 ) ) ;
#97491 = ORIENTED_EDGE ( 'NONE', *, *, #67109, .T. ) ;
#97492 = DIRECTION ( 'NONE',  ( 0.000000000000000000, 1.000000000000000000, 0.000000000000000000 ) ) ;
#97493 = DIRECTION ( 'NONE',  ( 0.000000000000000000, 0.000000000000000000, 1.000000000000000000 ) ) ;
#97494 = AXIS2_PLACEMENT_3D ( 'NONE', #11572, #51513, #22061 ) ;
#97495 = ORIENTED_EDGE ( 'NONE', *, *, #40082, .F. ) ;
#97496 = DIRECTION ( 'NONE',  ( -0.000000000000000000, 1.000000000000000000, -0.000000000000000000 ) ) ;
#97497 = EDGE_CURVE ( 'NONE', #43212, #124362, #8706, .T. ) ;
#97498 = CARTESIAN_POINT ( 'NONE',  ( -4.350000000000027178, 12.50000000000000000, -6.841600689897077814 ) ) ;
#97500 = AXIS2_PLACEMENT_3D ( 'NONE', #6589, #17052, #27537 ) ;
#97499 = AXIS2_PLACEMENT_3D ( 'NONE', #61407, #91493, #1813 ) ;
#97501 = EDGE_CURVE ( 'NONE', #61453, #36022, #45675, .T. ) ;
#97502 = DIRECTION ( 'NONE',  ( 0.000000000000000000, 1.000000000000000000, 0.000000000000000000 ) ) ;
#97503 = ORIENTED_EDGE ( 'NONE', *, *, #61971, .T. ) ;
#97504 = DIRECTION ( 'NONE',  ( 0.000000000000000000, -0.000000000000000000, 1.000000000000000000 ) ) ;
#97505 = CARTESIAN_POINT ( 'NONE',  ( 2.049999999999950084, 2.500000000000000000, 2.165063509461097713 ) ) ;
#97506 = ORIENTED_EDGE ( 'NONE', *, *, #125339, .F. ) ;
#97507 = ORIENTED_EDGE ( 'NONE', *, *, #41042, .F. ) ;
#97508 = ORIENTED_EDGE ( 'NONE', *, *, #58877, .F. ) ;
#97509 = DIRECTION ( 'NONE',  ( 0.000000000000000000, -0.000000000000000000, 1.000000000000000000 ) ) ;
#97510 = DIRECTION ( 'NONE',  ( -0.000000000000000000, 1.000000000000000000, -0.000000000000000000 ) ) ;
#97511 = VERTEX_POINT ( 'NONE', #106766 ) ;
#97512 = FACE_OUTER_BOUND ( 'NONE', #89176, .T. ) ;
#97513 = CARTESIAN_POINT ( 'NONE',  ( 11.04999999999991189, 12.50000000000000000, 6.083687093685483660 ) ) ;
#97514 = PLANE ( 'NONE',  #35807 ) ;
#97515 = CARTESIAN_POINT ( 'NONE',  ( -1.450000000000035483, 12.50000000000000000, 6.213873640053559022 ) ) ;
#97516 = VERTEX_POINT ( 'NONE', #27551 ) ;
#97517 = CONICAL_SURFACE ( 'NONE', #53618, 0.1000000000000002554, 0.003490658503988666988 ) ;
#97518 = FACE_OUTER_BOUND ( 'NONE', #17204, .T. ) ;
#97519 = AXIS2_PLACEMENT_3D ( 'NONE', #52278, #129575, #10408 ) ;
#97520 = EDGE_LOOP ( 'NONE', ( #95634, #39601, #22141, #129366 ) ) ;
#97521 = VERTEX_POINT ( 'NONE', #96952 ) ;
#97522 = DIRECTION ( 'NONE',  ( 0.000000000000000000, 1.000000000000000000, 0.000000000000000000 ) ) ;
#97523 = CARTESIAN_POINT ( 'NONE',  ( 8.149999999999923972, 12.50000000000000000, -6.841600689897077814 ) ) ;
#97524 = FACE_BOUND ( 'NONE', #59944, .T. ) ;
#97525 = CARTESIAN_POINT ( 'NONE',  ( 186.1979166673494603, 6.668395609140176816, 3.850000000000000977 ) ) ;
#97526 = DIRECTION ( 'NONE',  ( 0.000000000000000000, 1.000000000000000000, 0.000000000000000000 ) ) ;
#97527 = CIRCLE ( 'NONE', #36912, 0.06509327318403745899 ) ;
#97528 = DIRECTION ( 'NONE',  ( -0.000000000000000000, 1.000000000000000000, -0.000000000000000000 ) ) ;
#97529 = EDGE_CURVE ( 'NONE', #106540, #17110, #87503, .T. ) ;
#97530 = ORIENTED_EDGE ( 'NONE', *, *, #30655, .F. ) ;
#97531 = DIRECTION ( 'NONE',  ( -0.000000000000000000, 1.000000000000000000, -0.000000000000000000 ) ) ;
#97532 = DIRECTION ( 'NONE',  ( -4.274815082592931898E-19, -0.9999939076577903929, -0.003490651415223739937 ) ) ;
#97533 = DIRECTION ( 'NONE',  ( 0.000000000000000000, 1.000000000000000000, 0.000000000000000000 ) ) ;
#97534 = DIRECTION ( 'NONE',  ( -0.000000000000000000, -1.000000000000000000, -0.000000000000000000 ) ) ;
#97535 = ORIENTED_EDGE ( 'NONE', *, *, #111289, .T. ) ;
#97537 = AXIS2_PLACEMENT_3D ( 'NONE', #21064, #61657, #112039 ) ;
#97536 = CONICAL_SURFACE ( 'NONE', #41135, 0.1000000000000000472, 0.003490658503988666988 ) ;
#97538 = ADVANCED_FACE ( 'NONE', ( #46556 ), #66582, .T. ) ;
#97539 = CARTESIAN_POINT ( 'NONE',  ( -1.900000000000034106, 2.500000000000000000, -3.983716857408426293 ) ) ;
#97540 = AXIS2_PLACEMENT_3D ( 'NONE', #34698, #12442, #73955 ) ;
#97541 = CARTESIAN_POINT ( 'NONE',  ( 6.699999999999930012, 2.500000000000000000, -4.430127018922202176 ) ) ;
#97542 = ORIENTED_EDGE ( 'NONE', *, *, #48710, .T. ) ;
#97543 = ORIENTED_EDGE ( 'NONE', *, *, #34063, .T. ) ;
#97544 = EDGE_CURVE ( 'NONE', #18257, #7901, #85371, .T. ) ;
#97545 = CARTESIAN_POINT ( 'NONE',  ( 3.149999999999942624, 2.500000000000000000, 6.248780366869521430 ) ) ;
#97547 = EDGE_CURVE ( 'NONE', #122621, #129104, #75372, .T. ) ;
#97546 = DIRECTION ( 'NONE',  ( 0.000000000000000000, 0.000000000000000000, 1.000000000000000000 ) ) ;
#97548 = FACE_BOUND ( 'NONE', #43980, .T. ) ;
#97549 = CARTESIAN_POINT ( 'NONE',  ( -15.19999999999998153, 2.500000000000000000, -0.3464101615137759604 ) ) ;
#97550 = VERTEX_POINT ( 'NONE', #47224 ) ;
#97551 = FACE_OUTER_BOUND ( 'NONE', #2803, .T. ) ;
#97552 = EDGE_CURVE ( 'NONE', #12366, #51199, #62407, .T. ) ;
#97553 = ORIENTED_EDGE ( 'NONE', *, *, #88399, .T. ) ;
#97554 = ORIENTED_EDGE ( 'NONE', *, *, #37325, .F. ) ;
#97555 = DIRECTION ( 'NONE',  ( 0.000000000000000000, -0.000000000000000000, 1.000000000000000000 ) ) ;
#97556 = ADVANCED_FACE ( 'NONE', ( #87130 ), #120972, .T. ) ;
#97557 = CARTESIAN_POINT ( 'NONE',  ( 186.6666666666666856, -6.668395609140176816, -3.850000000000003642 ) ) ;
#97558 = AXIS2_PLACEMENT_3D ( 'NONE', #103876, #26603, #126078 ) ;
#97559 = ORIENTED_EDGE ( 'NONE', *, *, #55020, .F. ) ;
#97560 = CARTESIAN_POINT ( 'NONE',  ( 1.249999999999953815, 2.500000000000000000, 1.372243186433545370 ) ) ;
#97561 = AXIS2_PLACEMENT_3D ( 'NONE', #837, #123202, #30965 ) ;
#97562 = LINE ( 'NONE', #48467, #47257 ) ;
#97563 = AXIS2_PLACEMENT_3D ( 'NONE', #86074, #115539, #127329 ) ;
#97564 = CARTESIAN_POINT ( 'NONE',  ( -10.65000000000000213, 12.50000000000000000, 1.818653347947321475 ) ) ;
#97565 = DIRECTION ( 'NONE',  ( 0.000000000000000000, 0.000000000000000000, 1.000000000000000000 ) ) ;
#97566 = AXIS2_PLACEMENT_3D ( 'NONE', #71166, #10319, #69220 ) ;
#97567 = CIRCLE ( 'NONE', #72552, 0.06509327318403745899 ) ;
#97568 = ORIENTED_EDGE ( 'NONE', *, *, #93171, .F. ) ;
#97569 = CIRCLE ( 'NONE', #70394, 0.06509327318403745899 ) ;
#97570 = LINE ( 'NONE', #77289, #39276 ) ;
#97571 = DIRECTION ( 'NONE',  ( 0.000000000000000000, -0.9999939076577903929, 0.003490651415223739937 ) ) ;
#97572 = DIRECTION ( 'NONE',  ( 0.000000000000000000, 0.000000000000000000, -1.000000000000000000 ) ) ;
#97573 = VERTEX_POINT ( 'NONE', #37409 ) ;
#97574 = CARTESIAN_POINT ( 'NONE',  ( 87.50000000000001421, 3.975344334345554120, -6.360552532166837914 ) ) ;
#97575 = ORIENTED_EDGE ( 'NONE', *, *, #100636, .T. ) ;
#97576 = CIRCLE ( 'NONE', #28641, 0.1000000000000002554 ) ;
#97577 = DIRECTION ( 'NONE',  ( 0.000000000000000000, 0.000000000000000000, -1.000000000000000000 ) ) ;
#97578 = AXIS2_PLACEMENT_3D ( 'NONE', #18815, #58752, #48940 ) ;
#97579 = ORIENTED_EDGE ( 'NONE', *, *, #12192, .F. ) ;
#97580 = DIRECTION ( 'NONE',  ( 0.000000000000000000, 0.000000000000000000, 1.000000000000000000 ) ) ;
#97581 = CARTESIAN_POINT ( 'NONE',  ( 17.50000000000000000, -2.500000000000000000, -0.3333333333333280413 ) ) ;
#97582 = EDGE_CURVE ( 'NONE', #27222, #32827, #102099, .T. ) ;
#97583 = CARTESIAN_POINT ( 'NONE',  ( 10.44999999999991402, 2.500000000000000000, -2.265063509461101798 ) ) ;
#97585 = AXIS2_PLACEMENT_3D ( 'NONE', #67443, #70533, #27532 ) ;
#97584 = CIRCLE ( 'NONE', #32858, 0.09999999999999982514 ) ;
#97586 = CARTESIAN_POINT ( 'NONE',  ( -14.14999999999998614, 2.500000000000000000, -2.957883832488651610 ) ) ;
#97587 = EDGE_LOOP ( 'NONE', ( #107338, #87495, #56736, #8466 ) ) ;
#97588 = CARTESIAN_POINT ( 'NONE',  ( -7.950000000000012612, 2.500000000000000000, -2.265063509461101798 ) ) ;
#97589 = CARTESIAN_POINT ( 'NONE',  ( -4.600000000000028066, 12.50000000000000000, -5.022947341949754119 ) ) ;
#97590 = CARTESIAN_POINT ( 'NONE',  ( 185.6927083336747160, 6.551208109652275624, -3.782341765624998686 ) ) ;
#97591 = CARTESIAN_POINT ( 'NONE',  ( 187.5000000000000000, 0.000000000000000000, 7.700000000000000178 ) ) ;
#97592 = ADVANCED_FACE ( 'NONE', ( #26934 ), #114701, .T. ) ;
#97593 = DIRECTION ( 'NONE',  ( 0.000000000000000000, -0.000000000000000000, 1.000000000000000000 ) ) ;
#97594 = ADVANCED_FACE ( 'NONE', ( #125137 ), #77317, .T. ) ;
#97595 = ORIENTED_EDGE ( 'NONE', *, *, #29076, .F. ) ;
#97596 = ORIENTED_EDGE ( 'NONE', *, *, #25472, .F. ) ;
#97597 = DIRECTION ( 'NONE',  ( 0.000000000000000000, 1.000000000000000000, 0.000000000000000000 ) ) ;
#97598 = VERTEX_POINT ( 'NONE', #96301 ) ;
#97599 = DIRECTION ( 'NONE',  ( 0.000000000000000000, 0.000000000000000000, 1.000000000000000000 ) ) ;
#97600 = EDGE_CURVE ( 'NONE', #85528, #42572, #15807, .T. ) ;
#97602 = ORIENTED_EDGE ( 'NONE', *, *, #54293, .T. ) ;
#97601 = ORIENTED_EDGE ( 'NONE', *, *, #24851, .F. ) ;
#97603 = VERTEX_POINT ( 'NONE', #66840 ) ;
#97604 = EDGE_CURVE ( 'NONE', #4802, #69367, #18472, .T. ) ;
#97605 = AXIS2_PLACEMENT_3D ( 'NONE', #35784, #115613, #126081 ) ;
#97606 = DIRECTION ( 'NONE',  ( 0.000000000000000000, 1.000000000000000000, 0.000000000000000000 ) ) ;
#97607 = EDGE_CURVE ( 'NONE', #46462, #3084, #58289, .T. ) ;
#97608 = CARTESIAN_POINT ( 'NONE',  ( 11.64999999999990621, 2.500000000000000000, 6.595190528383296780 ) ) ;
#97609 = DIRECTION ( 'NONE',  ( 0.000000000000000000, 0.000000000000000000, 1.000000000000000000 ) ) ;
#97610 = ADVANCED_FACE ( 'NONE', ( #108063 ), #67469, .T. ) ;
#97611 = FACE_OUTER_BOUND ( 'NONE', #121146, .T. ) ;
#97612 = DIRECTION ( 'NONE',  ( 0.000000000000000000, 1.000000000000000000, 0.000000000000000000 ) ) ;
#97613 = DIRECTION ( 'NONE',  ( 0.000000000000000000, 0.000000000000000000, 1.000000000000000000 ) ) ;
#97614 = CARTESIAN_POINT ( 'NONE',  ( -1.250000000000037970, 2.500000000000000000, 7.188010851410848723 ) ) ;
#97615 = ORIENTED_EDGE ( 'NONE', *, *, #65533, .T. ) ;
#97617 = EDGE_CURVE ( 'NONE', #9937, #56654, #17740, .T. ) ;
#97616 = CARTESIAN_POINT ( 'NONE',  ( 0.4499999999999573785, 2.500000000000000000, -6.495190528383302464 ) ) ;
#97618 = ORIENTED_EDGE ( 'NONE', *, *, #42178, .T. ) ;
#97619 = EDGE_CURVE ( 'NONE', #7894, #70834, #47874, .T. ) ;
#97621 = EDGE_LOOP ( 'NONE', ( #58735, #83021, #7334, #36162 ) ) ;
#97620 = AXIS2_PLACEMENT_3D ( 'NONE', #95513, #45777, #122404 ) ;
#97622 = EDGE_LOOP ( 'NONE', ( #24793, #93808 ) ) ;
#97623 = ORIENTED_EDGE ( 'NONE', *, *, #80856, .T. ) ;
#97624 = CIRCLE ( 'NONE', #16116, 7.700000000000000178 ) ;
#97625 = CARTESIAN_POINT ( 'NONE',  ( 7.699999999999923794, 12.50000000000000000, -0.2813168883297409439 ) ) ;
#97626 = ORIENTED_EDGE ( 'NONE', *, *, #54533, .F. ) ;
#97627 = VERTEX_POINT ( 'NONE', #58343 ) ;
#97629 = CIRCLE ( 'NONE', #55853, 0.06509327318403745899 ) ;
#97628 = CIRCLE ( 'NONE', #118551, 0.1000000000000002554 ) ;
#97630 = DIRECTION ( 'NONE',  ( 0.000000000000000000, 0.000000000000000000, 1.000000000000000000 ) ) ;
#97631 = DIRECTION ( 'NONE',  ( 0.000000000000000000, 1.000000000000000000, 0.000000000000000000 ) ) ;
#97632 = CARTESIAN_POINT ( 'NONE',  ( 8.349999999999923261, 12.50000000000000000, -6.495190528383302464 ) ) ;
#97633 = FACE_OUTER_BOUND ( 'NONE', #56530, .T. ) ;
#97634 = DIRECTION ( 'NONE',  ( -0.000000000000000000, -1.000000000000000000, -0.000000000000000000 ) ) ;
#97635 = EDGE_LOOP ( 'NONE', ( #70058, #25236, #26384, #43069 ) ) ;
#97636 = CARTESIAN_POINT ( 'NONE',  ( -6.450000000000014388, 12.50000000000000000, 6.148780366869520897 ) ) ;
#97638 = AXIS2_PLACEMENT_3D ( 'NONE', #107366, #7214, #127651 ) ;
#97637 = VECTOR ( 'NONE', #20715, 1000.000000000000000 ) ;
#97639 = ORIENTED_EDGE ( 'NONE', *, *, #85436, .F. ) ;
#97640 = CARTESIAN_POINT ( 'NONE',  ( -8.550000000000009592, 12.50000000000000000, 6.841600689897072485 ) ) ;
#97641 = AXIS2_PLACEMENT_3D ( 'NONE', #34326, #74231, #4178 ) ;
#97642 = EDGE_LOOP ( 'NONE', ( #32906, #107695, #107333, #57087 ) ) ;
#97643 = DIRECTION ( 'NONE',  ( -0.000000000000000000, -1.000000000000000000, -0.000000000000000000 ) ) ;
#97644 = ORIENTED_EDGE ( 'NONE', *, *, #33156, .T. ) ;
#97645 = VERTEX_POINT ( 'NONE', #79269 ) ;
#97646 = CARTESIAN_POINT ( 'NONE',  ( -7.900000000000011013, 2.500000000000000000, 4.430127018922196847 ) ) ;
#97647 = LINE ( 'NONE', #59687, #48558 ) ;
#97648 = FACE_OUTER_BOUND ( 'NONE', #58345, .T. ) ;
#97649 = ADVANCED_FACE ( 'NONE', ( #20336 ), #51100, .T. ) ;
#97650 = LINE ( 'NONE', #98943, #69807 ) ;
#97651 = CARTESIAN_POINT ( 'NONE',  ( -1.850000000000033396, 12.50000000000000000, -6.148780366869526226 ) ) ;
#97652 = EDGE_LOOP ( 'NONE', ( #7820, #110640 ) ) ;
#97653 = DIRECTION ( 'NONE',  ( 0.000000000000000000, 0.000000000000000000, 1.000000000000000000 ) ) ;
#97654 = CARTESIAN_POINT ( 'NONE',  ( 10.44999999999991402, 2.500000000000000000, 6.595190528383296780 ) ) ;
#97655 = CARTESIAN_POINT ( 'NONE',  ( -13.14999999999999147, 2.500000000000000000, 1.818653347947325472 ) ) ;
#97656 = DIRECTION ( 'NONE',  ( 0.000000000000000000, 1.000000000000000000, 0.000000000000000000 ) ) ;
#97657 = CIRCLE ( 'NONE', #47493, 0.06509327318403745899 ) ;
#97659 = EDGE_CURVE ( 'NONE', #43021, #87479, #128834, .T. ) ;
#97658 = DIRECTION ( 'NONE',  ( 0.000000000000000000, -0.000000000000000000, 1.000000000000000000 ) ) ;
#97660 = ORIENTED_EDGE ( 'NONE', *, *, #52884, .T. ) ;
#97661 = AXIS2_PLACEMENT_3D ( 'NONE', #61815, #81447, #72912 ) ;
#97662 = ORIENTED_EDGE ( 'NONE', *, *, #9943, .T. ) ;
#97663 = CARTESIAN_POINT ( 'NONE',  ( -11.84999999999999787, 2.500000000000000000, -6.148780366869522673 ) ) ;
#97664 = VECTOR ( 'NONE', #124633, 1000.000000000000000 ) ;
#97665 = ORIENTED_EDGE ( 'NONE', *, *, #120950, .F. ) ;
#97666 = AXIS2_PLACEMENT_3D ( 'NONE', #68433, #110302, #20645 ) ;
#97667 = DIRECTION ( 'NONE',  ( 0.000000000000000000, 1.000000000000000000, 0.000000000000000000 ) ) ;
#97668 = DIRECTION ( 'NONE',  ( 0.000000000000000000, -0.000000000000000000, 1.000000000000000000 ) ) ;
#97669 = CONICAL_SURFACE ( 'NONE', #93559, 0.09999999999999982514, 0.003490658503988666988 ) ;
#97670 = VERTEX_POINT ( 'NONE', #121106 ) ;
#97671 = CARTESIAN_POINT ( 'NONE',  ( 185.6250000000000284, -8.891194145520236347, -1.633285867636356693E-15 ) ) ;
#97673 = CIRCLE ( 'NONE', #30796, 0.09999999999999982514 ) ;
#97672 = CARTESIAN_POINT ( 'NONE',  ( 3.349999999999941025, 2.500000000000000000, 7.088010851410848190 ) ) ;
#97674 = DIRECTION ( 'NONE',  ( 0.000000000000000000, 0.000000000000000000, -1.000000000000000000 ) ) ;
#97675 = CARTESIAN_POINT ( 'NONE',  ( 6.649999999999929301, 2.500000000000000000, 6.495190528383297135 ) ) ;
#97676 = ORIENTED_EDGE ( 'NONE', *, *, #117370, .T. ) ;
#97677 = AXIS2_PLACEMENT_3D ( 'NONE', #109547, #97786, #7457 ) ;
#97678 = CARTESIAN_POINT ( 'NONE',  ( -1.650000000000035216, 2.500000000000000000, -1.472243186433550122 ) ) ;
#97679 = FACE_OUTER_BOUND ( 'NONE', #74003, .T. ) ;
#97680 = ORIENTED_EDGE ( 'NONE', *, *, #39930, .F. ) ;
#97681 = CARTESIAN_POINT ( 'NONE',  ( -2.100000000000033396, 12.50000000000000000, -3.637306695894650055 ) ) ;
#97682 = CARTESIAN_POINT ( 'NONE',  ( 3.549999999999944755, 2.500000000000000000, -2.511473670974877948 ) ) ;
#97683 = DIRECTION ( 'NONE',  ( 0.000000000000000000, 1.000000000000000000, 0.000000000000000000 ) ) ;
#97684 = ORIENTED_EDGE ( 'NONE', *, *, #65483, .T. ) ;
#97685 = FACE_OUTER_BOUND ( 'NONE', #48247, .T. ) ;
#97686 = VERTEX_POINT ( 'NONE', #119820 ) ;
#97687 = DIRECTION ( 'NONE',  ( 0.000000000000000000, 0.000000000000000000, 1.000000000000000000 ) ) ;
#97688 = DIRECTION ( 'NONE',  ( -0.000000000000000000, -1.000000000000000000, -0.000000000000000000 ) ) ;
#97689 = CIRCLE ( 'NONE', #35029, 0.06509327318403745899 ) ;
#97690 = CARTESIAN_POINT ( 'NONE',  ( 3.949999999999939782, 12.50000000000000000, 2.511473670974873507 ) ) ;
#97691 = ORIENTED_EDGE ( 'NONE', *, *, #97139, .F. ) ;
#97692 = ADVANCED_FACE ( 'NONE', ( #110010 ), #3319, .T. ) ;
#97693 = CARTESIAN_POINT ( 'NONE',  ( -9.550000000000002487, 2.500000000000000000, 6.495190528383297135 ) ) ;
#97694 = VERTEX_POINT ( 'NONE', #20974 ) ;
#97695 = EDGE_CURVE ( 'NONE', #18337, #72434, #118331, .T. ) ;
#97696 = CARTESIAN_POINT ( 'NONE',  ( -11.24999999999996270, 2.500000000000000000, 2.165063509461097713 ) ) ;
#97697 = EDGE_CURVE ( 'NONE', #11408, #24701, #61561, .T. ) ;
#97698 = ORIENTED_EDGE ( 'NONE', *, *, #81965, .F. ) ;
#97699 = DIRECTION ( 'NONE',  ( 0.000000000000000000, 1.000000000000000000, 0.000000000000000000 ) ) ;
#97700 = AXIS2_PLACEMENT_3D ( 'NONE', #89882, #40151, #105167 ) ;
#97701 = VECTOR ( 'NONE', #127938, 1000.000000000000000 ) ;
#97702 = ORIENTED_EDGE ( 'NONE', *, *, #33345, .F. ) ;
#97703 = FACE_OUTER_BOUND ( 'NONE', #21881, .T. ) ;
#97704 = DIRECTION ( 'NONE',  ( 0.000000000000000000, 1.000000000000000000, 0.000000000000000000 ) ) ;
#97705 = EDGE_CURVE ( 'NONE', #80059, #2046, #30170, .T. ) ;
#97706 = ADVANCED_FACE ( 'NONE', ( #89080 ), #47251, .T. ) ;
#97707 = ORIENTED_EDGE ( 'NONE', *, *, #99936, .T. ) ;
#97708 = VERTEX_POINT ( 'NONE', #39358 ) ;
#97709 = EDGE_CURVE ( 'NONE', #108298, #8661, #21625, .T. ) ;
#97710 = DIRECTION ( 'NONE',  ( 0.000000000000000000, 0.000000000000000000, 1.000000000000000000 ) ) ;
#97711 = CARTESIAN_POINT ( 'NONE',  ( -11.64999999999999680, 2.500000000000000000, 5.702370205355745014 ) ) ;
#97712 = ORIENTED_EDGE ( 'NONE', *, *, #73505, .T. ) ;
#97714 = CONICAL_SURFACE ( 'NONE', #87237, 0.09999999999999982514, 0.003490658503988666988 ) ;
#97713 = CONICAL_SURFACE ( 'NONE', #74742, 0.1000000000000002554, 0.003490658503988666988 ) ;
#97715 = DIRECTION ( 'NONE',  ( -0.000000000000000000, 1.000000000000000000, -0.000000000000000000 ) ) ;
#97716 = DIRECTION ( 'NONE',  ( 0.000000000000000000, 0.000000000000000000, 1.000000000000000000 ) ) ;
#97717 = AXIS2_PLACEMENT_3D ( 'NONE', #101647, #23082, #11962 ) ;
#97718 = CARTESIAN_POINT ( 'NONE',  ( 107.6617659101945748, 7.119691004531019551, -5.000000000000002665 ) ) ;
#97719 = DIRECTION ( 'NONE',  ( 0.000000000000000000, 0.000000000000000000, -1.000000000000000000 ) ) ;
#97720 = DIRECTION ( 'NONE',  ( -4.274815082592931898E-19, -0.9999939076577903929, -0.003490651415223739937 ) ) ;
#97721 = CARTESIAN_POINT ( 'NONE',  ( -6.450000000000019718, 2.500000000000000000, -6.248780366869526759 ) ) ;
#97722 = CIRCLE ( 'NONE', #114176, 0.09999999999999982514 ) ;
#97723 = AXIS2_PLACEMENT_3D ( 'NONE', #99680, #12558, #80684 ) ;
#97724 = ORIENTED_EDGE ( 'NONE', *, *, #101984, .T. ) ;
#97725 = ORIENTED_EDGE ( 'NONE', *, *, #38679, .T. ) ;
#97726 = ORIENTED_EDGE ( 'NONE', *, *, #47535, .T. ) ;
#97727 = EDGE_LOOP ( 'NONE', ( #125889, #9616, #53347, #99685 ) ) ;
#97728 = CARTESIAN_POINT ( 'NONE',  ( -3.950000000000026379, 2.500000000000000000, 2.611473670974873151 ) ) ;
#97729 = CARTESIAN_POINT ( 'NONE',  ( -11.44999999999999751, 2.500000000000000000, 2.511473670974873507 ) ) ;
#97730 = CARTESIAN_POINT ( 'NONE',  ( 8.349999999999919709, 2.500000000000000000, 5.802370205355744659 ) ) ;
#97731 = EDGE_LOOP ( 'NONE', ( #40684, #33648 ) ) ;
#97732 = FACE_BOUND ( 'NONE', #97731, .T. ) ;
#97733 = EDGE_LOOP ( 'NONE', ( #128116, #12778, #35747, #66785 ) ) ;
#97734 = DIRECTION ( 'NONE',  ( -0.000000000000000000, -1.000000000000000000, -0.000000000000000000 ) ) ;
#97735 = DIRECTION ( 'NONE',  ( 0.000000000000000000, 0.000000000000000000, 1.000000000000000000 ) ) ;
#97736 = CARTESIAN_POINT ( 'NONE',  ( 3.949999999999942446, 2.500000000000000000, -2.411473670974877859 ) ) ;
#97737 = VECTOR ( 'NONE', #93247, 1000.000000000000000 ) ;
#97738 = DIRECTION ( 'NONE',  ( -0.000000000000000000, 1.000000000000000000, -0.000000000000000000 ) ) ;
#97739 = CARTESIAN_POINT ( 'NONE',  ( 11.64999999999990798, 2.500000000000000000, 5.702370205355745014 ) ) ;
#97740 = CIRCLE ( 'NONE', #106158, 0.06509327318403745899 ) ;
#97741 = DIRECTION ( 'NONE',  ( 0.000000000000000000, 1.000000000000000000, 0.000000000000000000 ) ) ;
#97742 = DIRECTION ( 'NONE',  ( 0.000000000000000000, -0.000000000000000000, 1.000000000000000000 ) ) ;
#97743 = DIRECTION ( 'NONE',  ( 0.000000000000000000, 0.000000000000000000, 1.000000000000000000 ) ) ;
#97744 = DIRECTION ( 'NONE',  ( -4.274815082592931898E-19, -0.9999939076577903929, -0.003490651415223739937 ) ) ;
#97745 = AXIS2_PLACEMENT_3D ( 'NONE', #56210, #86968, #16902 ) ;
#97746 = VECTOR ( 'NONE', #109999, 1000.000000000000000 ) ;
#97747 = LINE ( 'NONE', #108211, #48089 ) ;
#97748 = ORIENTED_EDGE ( 'NONE', *, *, #88684, .F. ) ;
#97750 = ORIENTED_EDGE ( 'NONE', *, *, #82978, .T. ) ;
#97749 = CIRCLE ( 'NONE', #7856, 0.09999999999999982514 ) ;
#97751 = ORIENTED_EDGE ( 'NONE', *, *, #122754, .F. ) ;
#97752 = ORIENTED_EDGE ( 'NONE', *, *, #119921, .T. ) ;
#97753 = CARTESIAN_POINT ( 'NONE',  ( 10.84999999999991260, 2.500000000000000000, -1.472243186433550122 ) ) ;
#97754 = ADVANCED_FACE ( 'NONE', ( #81194 ), #72383, .T. ) ;
#97755 = PLANE ( 'NONE',  #6708 ) ;
#97756 = EDGE_CURVE ( 'NONE', #127901, #56703, #19025, .T. ) ;
#97758 = VERTEX_POINT ( 'NONE', #98885 ) ;
#97757 = ORIENTED_EDGE ( 'NONE', *, *, #20443, .F. ) ;
#97760 = ORIENTED_EDGE ( 'NONE', *, *, #43108, .T. ) ;
#97759 = VECTOR ( 'NONE', #75514, 1000.000000000000000 ) ;
#97761 = ADVANCED_FACE ( 'NONE', ( #31452 ), #9582, .T. ) ;
#97763 = VECTOR ( 'NONE', #82133, 1000.000000000000000 ) ;
#97762 = FACE_OUTER_BOUND ( 'NONE', #122414, .T. ) ;
#97764 = AXIS2_PLACEMENT_3D ( 'NONE', #126832, #57448, #56142 ) ;
#97765 = CARTESIAN_POINT ( 'NONE',  ( 14.54999999999989591, 12.50000000000000000, 2.230156782645134950 ) ) ;
#97766 = DIRECTION ( 'NONE',  ( -0.000000000000000000, -1.000000000000000000, -0.000000000000000000 ) ) ;
#97767 = EDGE_CURVE ( 'NONE', #127558, #62304, #40998, .T. ) ;
#97768 = DIRECTION ( 'NONE',  ( 0.000000000000000000, 0.000000000000000000, -1.000000000000000000 ) ) ;
#97769 = EDGE_CURVE ( 'NONE', #41599, #51279, #124181, .T. ) ;
#97770 = DIRECTION ( 'NONE',  ( -0.000000000000000000, 1.000000000000000000, -0.000000000000000000 ) ) ;
#97771 = CARTESIAN_POINT ( 'NONE',  ( -13.74999999999998757, 2.500000000000000000, -2.857883832488651521 ) ) ;
#97772 = AXIS2_PLACEMENT_3D ( 'NONE', #96006, #116274, #45631 ) ;
#97773 = ORIENTED_EDGE ( 'NONE', *, *, #7981, .T. ) ;
#97775 = EDGE_CURVE ( 'NONE', #126779, #108066, #70225, .T. ) ;
#97774 = CARTESIAN_POINT ( 'NONE',  ( 13.94999999999989804, 12.50000000000000000, 1.818653347947321475 ) ) ;
#97776 = ORIENTED_EDGE ( 'NONE', *, *, #76038, .F. ) ;
#97778 = EDGE_CURVE ( 'NONE', #100183, #123328, #63960, .T. ) ;
#97777 = AXIS2_PLACEMENT_3D ( 'NONE', #2155, #100370, #30358 ) ;
#97779 = ORIENTED_EDGE ( 'NONE', *, *, #9483, .F. ) ;
#97780 = EDGE_LOOP ( 'NONE', ( #108992, #117550 ) ) ;
#97781 = CARTESIAN_POINT ( 'NONE',  ( -7.900000000000014566, 2.500000000000000000, -0.1000000000000022815 ) ) ;
#97782 = ORIENTED_EDGE ( 'NONE', *, *, #28576, .T. ) ;
#97783 = ORIENTED_EDGE ( 'NONE', *, *, #34063, .F. ) ;
#97784 = ADVANCED_FACE ( 'NONE', ( #63481 ), #83132, .T. ) ;
#97785 = DIRECTION ( 'NONE',  ( 0.000000000000000000, 0.000000000000000000, 1.000000000000000000 ) ) ;
#97786 = DIRECTION ( 'NONE',  ( -0.000000000000000000, -1.000000000000000000, -0.000000000000000000 ) ) ;
#97787 = CARTESIAN_POINT ( 'NONE',  ( 179.5000000000000000, 1.375000000000002442, -7.576237522675751457 ) ) ;
#97788 = DIRECTION ( 'NONE',  ( 0.000000000000000000, 1.000000000000000000, 0.000000000000000000 ) ) ;
#97789 = DIRECTION ( 'NONE',  ( 0.000000000000000000, 1.000000000000000000, 0.000000000000000000 ) ) ;
#97790 = ORIENTED_EDGE ( 'NONE', *, *, #111446, .F. ) ;
#97791 = CARTESIAN_POINT ( 'NONE',  ( -2.900000000000030109, 12.50000000000000000, -3.637306695894650055 ) ) ;
#97792 = ORIENTED_EDGE ( 'NONE', *, *, #59937, .F. ) ;
#97793 = DIRECTION ( 'NONE',  ( 0.000000000000000000, 0.000000000000000000, 1.000000000000000000 ) ) ;
#97794 = VERTEX_POINT ( 'NONE', #3272 ) ;
#97795 = CARTESIAN_POINT ( 'NONE',  ( 111.0583702135628528, 7.744754444937881566, -3.968742208708922359 ) ) ;
#97796 = CARTESIAN_POINT ( 'NONE',  ( -11.84999999999999609, 2.500000000000000000, 6.841600689897072485 ) ) ;
#97797 = ORIENTED_EDGE ( 'NONE', *, *, #124061, .T. ) ;
#97798 = LINE ( 'NONE', #8755, #121911 ) ;
#97799 = DIRECTION ( 'NONE',  ( 0.000000000000000000, 0.000000000000000000, -1.000000000000000000 ) ) ;
#97800 = ORIENTED_EDGE ( 'NONE', *, *, #95593, .T. ) ;
#97801 = CIRCLE ( 'NONE', #18377, 0.06509327318403745899 ) ;
#97802 = FACE_OUTER_BOUND ( 'NONE', #121264, .T. ) ;
#97803 = ORIENTED_EDGE ( 'NONE', *, *, #6378, .T. ) ;
#97804 = EDGE_LOOP ( 'NONE', ( #7542, #28899 ) ) ;
#97805 = FACE_OUTER_BOUND ( 'NONE', #8357, .T. ) ;
#97806 = DIRECTION ( 'NONE',  ( 0.000000000000000000, 1.000000000000000000, 0.000000000000000000 ) ) ;
#97807 = CARTESIAN_POINT ( 'NONE',  ( 187.3385416670080872, 6.551208109652274736, 3.782341765625001351 ) ) ;
#97808 = CARTESIAN_POINT ( 'NONE',  ( 6.649999999999928413, 2.500000000000000000, 2.857883832488649301 ) ) ;
#97809 = VECTOR ( 'NONE', #117397, 1000.000000000000000 ) ;
#97810 = AXIS2_PLACEMENT_3D ( 'NONE', #11158, #120481, #111962 ) ;
#97812 = EDGE_CURVE ( 'NONE', #2544, #18098, #111942, .T. ) ;
#97811 = LINE ( 'NONE', #76253, #10251 ) ;
#97813 = CIRCLE ( 'NONE', #112683, 0.06509327318403745899 ) ;
#97814 = DIRECTION ( 'NONE',  ( 0.000000000000000000, 0.000000000000000000, -1.000000000000000000 ) ) ;
#97815 = VERTEX_POINT ( 'NONE', #62209 ) ;
#97816 = DIRECTION ( 'NONE',  ( -0.000000000000000000, -1.000000000000000000, -0.000000000000000000 ) ) ;
#97817 = DIRECTION ( 'NONE',  ( 0.000000000000000000, 1.000000000000000000, 0.000000000000000000 ) ) ;
#97818 = ORIENTED_EDGE ( 'NONE', *, *, #90020, .T. ) ;
#97819 = AXIS2_PLACEMENT_3D ( 'NONE', #68347, #106967, #8762 ) ;
#97820 = FACE_OUTER_BOUND ( 'NONE', #10684, .T. ) ;
#97821 = DIRECTION ( 'NONE',  ( 0.000000000000000000, 0.000000000000000000, 1.000000000000000000 ) ) ;
#97822 = DIRECTION ( 'NONE',  ( 0.000000000000000000, 1.000000000000000000, 0.000000000000000000 ) ) ;
#97823 = CARTESIAN_POINT ( 'NONE',  ( 9.349999999999916156, 12.50000000000000000, 6.841600689897072485 ) ) ;
#97824 = DIRECTION ( 'NONE',  ( 0.000000000000000000, -0.9999939076577903929, 0.003490651415223739937 ) ) ;
#97825 = EDGE_LOOP ( 'NONE', ( #58919, #23371 ) ) ;
#97826 = AXIS2_PLACEMENT_3D ( 'NONE', #41375, #81285, #89166 ) ;
#97827 = DIRECTION ( 'NONE',  ( 0.000000000000000000, 0.000000000000000000, -1.000000000000000000 ) ) ;
#97828 = DIRECTION ( 'NONE',  ( 0.000000000000000000, 0.000000000000000000, 1.000000000000000000 ) ) ;
#97829 = AXIS2_PLACEMENT_3D ( 'NONE', #68299, #15967, #108231 ) ;
#97830 = ORIENTED_EDGE ( 'NONE', *, *, #80290, .T. ) ;
#97831 = CONICAL_SURFACE ( 'NONE', #114555, 0.1000000000000002554, 0.003490658503988666988 ) ;
#97832 = DIRECTION ( 'NONE',  ( 0.000000000000000000, 0.000000000000000000, -1.000000000000000000 ) ) ;
#97833 = CIRCLE ( 'NONE', #112436, 0.09999999999999982514 ) ;
#97834 = EDGE_LOOP ( 'NONE', ( #48739, #52825 ) ) ;
#97835 = ORIENTED_EDGE ( 'NONE', *, *, #58832, .T. ) ;
#97836 = DIRECTION ( 'NONE',  ( 0.000000000000000000, -0.9999939076577903929, 0.003490651415223739937 ) ) ;
#97837 = CIRCLE ( 'NONE', #128989, 0.06509327318403745899 ) ;
#97838 = ORIENTED_EDGE ( 'NONE', *, *, #111637, .F. ) ;
#97839 = DIRECTION ( 'NONE',  ( -1.000000000000000000, -0.000000000000000000, -0.000000000000000000 ) ) ;
#97840 = DIRECTION ( 'NONE',  ( 0.000000000000000000, 0.000000000000000000, 1.000000000000000000 ) ) ;
#97841 = DIRECTION ( 'NONE',  ( 0.000000000000000000, 0.000000000000000000, 1.000000000000000000 ) ) ;
#97842 = ORIENTED_EDGE ( 'NONE', *, *, #120970, .F. ) ;
#97843 = EDGE_CURVE ( 'NONE', #56218, #42111, #120399, .T. ) ;
#97844 = DIRECTION ( 'NONE',  ( 0.000000000000000000, -0.000000000000000000, 1.000000000000000000 ) ) ;
#97846 = VERTEX_POINT ( 'NONE', #93585 ) ;
#97845 = LINE ( 'NONE', #119411, #84948 ) ;
#97847 = DIRECTION ( 'NONE',  ( 0.000000000000000000, 0.000000000000000000, 1.000000000000000000 ) ) ;
#97848 = CIRCLE ( 'NONE', #30994, 0.06509327318403745899 ) ;
#97849 = EDGE_CURVE ( 'NONE', #31054, #106287, #2605, .T. ) ;
#97850 = DIRECTION ( 'NONE',  ( 0.000000000000000000, -0.000000000000000000, 1.000000000000000000 ) ) ;
#97851 = EDGE_CURVE ( 'NONE', #119823, #14270, #101478, .T. ) ;
#97852 = ORIENTED_EDGE ( 'NONE', *, *, #64069, .F. ) ;
#97853 = VECTOR ( 'NONE', #118612, 1000.000000000000000 ) ;
#97854 = VERTEX_POINT ( 'NONE', #122411 ) ;
#97855 = VERTEX_POINT ( 'NONE', #64117 ) ;
#97856 = CARTESIAN_POINT ( 'NONE',  ( -8.550000000000011369, 12.50000000000000000, 1.818653347947321475 ) ) ;
#97857 = CARTESIAN_POINT ( 'NONE',  ( -1.650000000000034772, 2.500000000000000000, 2.165063509461097713 ) ) ;
#97858 = EDGE_CURVE ( 'NONE', #50747, #112355, #54299, .T. ) ;
#97859 = EDGE_CURVE ( 'NONE', #121535, #89650, #32753, .T. ) ;
#97860 = DIRECTION ( 'NONE',  ( 0.000000000000000000, 0.000000000000000000, 1.000000000000000000 ) ) ;
#97861 = ADVANCED_FACE ( 'NONE', ( #22919 ), #7511, .T. ) ;
#97862 = FACE_BOUND ( 'NONE', #108970, .T. ) ;
#97864 = EDGE_CURVE ( 'NONE', #127371, #96017, #99476, .T. ) ;
#97863 = ORIENTED_EDGE ( 'NONE', *, *, #9581, .T. ) ;
#97865 = EDGE_CURVE ( 'NONE', #92342, #58017, #78650, .T. ) ;
#97866 = LINE ( 'NONE', #27835, #84631 ) ;
#97867 = CARTESIAN_POINT ( 'NONE',  ( -7.100000000000017408, 2.500000000000000000, -3.637306695894650055 ) ) ;
#97868 = ORIENTED_EDGE ( 'NONE', *, *, #93940, .F. ) ;
#97869 = LINE ( 'NONE', #56636, #34564 ) ;
#97870 = DIRECTION ( 'NONE',  ( 0.000000000000000000, 0.000000000000000000, 1.000000000000000000 ) ) ;
#97871 = FACE_OUTER_BOUND ( 'NONE', #106118, .T. ) ;
#97872 = ADVANCED_FACE ( 'NONE', ( #66048 ), #97400, .T. ) ;
#97873 = LINE ( 'NONE', #128665, #82651 ) ;
#97874 = CARTESIAN_POINT ( 'NONE',  ( -5.850000000000021849, 2.500000000000000000, -7.188010851410854052 ) ) ;
#97875 = CIRCLE ( 'NONE', #110496, 0.09999999999999982514 ) ;
#97876 = EDGE_LOOP ( 'NONE', ( #96791, #93475 ) ) ;
#97877 = ORIENTED_EDGE ( 'NONE', *, *, #76882, .T. ) ;
#97878 = ORIENTED_EDGE ( 'NONE', *, *, #104431, .T. ) ;
#97879 = AXIS2_PLACEMENT_3D ( 'NONE', #1316, #110631, #60275 ) ;
#97880 = AXIS2_PLACEMENT_3D ( 'NONE', #44483, #104054, #14363 ) ;
#97881 = ORIENTED_EDGE ( 'NONE', *, *, #123403, .F. ) ;
#97882 = VERTEX_POINT ( 'NONE', #126918 ) ;
#97883 = DIRECTION ( 'NONE',  ( 0.000000000000000000, 0.000000000000000000, 1.000000000000000000 ) ) ;
#97884 = DIRECTION ( 'NONE',  ( -0.000000000000000000, 1.000000000000000000, -0.000000000000000000 ) ) ;
#97885 = ORIENTED_EDGE ( 'NONE', *, *, #41521, .F. ) ;
#97886 = FACE_BOUND ( 'NONE', #86894, .T. ) ;
#97887 = CARTESIAN_POINT ( 'NONE',  ( -11.25000000000000000, 12.50000000000000000, -2.857883832488649745 ) ) ;
#97888 = CIRCLE ( 'NONE', #116757, 0.06509327318403745899 ) ;
#97889 = DIRECTION ( 'NONE',  ( 0.000000000000000000, -0.000000000000000000, 1.000000000000000000 ) ) ;
#97890 = CARTESIAN_POINT ( 'NONE',  ( 184.5000000000000000, -2.439371826966624468, 7.284141803326471099 ) ) ;
#97891 = DIRECTION ( 'NONE',  ( 0.000000000000000000, 1.000000000000000000, 0.000000000000000000 ) ) ;
#97892 = DIRECTION ( 'NONE',  ( 0.000000000000000000, -0.000000000000000000, 1.000000000000000000 ) ) ;
#97893 = VERTEX_POINT ( 'NONE', #107264 ) ;
#97894 = CARTESIAN_POINT ( 'NONE',  ( 8.949999999999921130, 2.500000000000000000, -6.841600689897078702 ) ) ;
#97895 = AXIS2_PLACEMENT_3D ( 'NONE', #98650, #49586, #128801 ) ;
#97896 = ORIENTED_EDGE ( 'NONE', *, *, #54766, .F. ) ;
#97897 = AXIS2_PLACEMENT_3D ( 'NONE', #39293, #119740, #87699 ) ;
#97898 = ORIENTED_EDGE ( 'NONE', *, *, #17313, .T. ) ;
#97899 = VERTEX_POINT ( 'NONE', #94870 ) ;
#97900 = PLANE ( 'NONE',  #48472 ) ;
#97901 = PLANE ( 'NONE',  #56803 ) ;
#97902 = DIRECTION ( 'NONE',  ( 0.000000000000000000, -0.9999939076577903929, 0.003490651415223739937 ) ) ;
#97903 = EDGE_CURVE ( 'NONE', #113580, #114828, #15645, .T. ) ;
#97904 = ORIENTED_EDGE ( 'NONE', *, *, #2588, .T. ) ;
#97905 = CARTESIAN_POINT ( 'NONE',  ( -9.350000000000008527, 2.500000000000000000, -6.048780366869521252 ) ) ;
#97906 = EDGE_CURVE ( 'NONE', #50060, #67824, #87617, .T. ) ;
#97907 = AXIS2_PLACEMENT_3D ( 'NONE', #103383, #72641, #115101 ) ;
#97908 = CARTESIAN_POINT ( 'NONE',  ( -1.450000000000035039, 12.50000000000000000, -6.776507416713039689 ) ) ;
#97909 = EDGE_CURVE ( 'NONE', #21143, #87403, #20058, .T. ) ;
#97910 = CARTESIAN_POINT ( 'NONE',  ( 7.049999999999930544, 2.500000000000000000, -6.595190528383302109 ) ) ;
#97911 = CARTESIAN_POINT ( 'NONE',  ( 185.0677083336747160, -4.367472073101514418, -7.564683531250002702 ) ) ;
#97912 = DIRECTION ( 'NONE',  ( 0.000000000000000000, 0.000000000000000000, 1.000000000000000000 ) ) ;
#97913 = LINE ( 'NONE', #109012, #25847 ) ;
#97914 = AXIS2_PLACEMENT_3D ( 'NONE', #104258, #125809, #105551 ) ;
#97915 = DIRECTION ( 'NONE',  ( 0.000000000000000000, 1.000000000000000000, 0.000000000000000000 ) ) ;
#97916 = ADVANCED_FACE ( 'NONE', ( #76527 ), #11721, .T. ) ;
#97917 = VERTEX_POINT ( 'NONE', #116430 ) ;
#97918 = DIRECTION ( 'NONE',  ( 0.000000000000000000, 0.000000000000000000, -1.000000000000000000 ) ) ;
#97919 = EDGE_CURVE ( 'NONE', #115380, #41348, #28464, .T. ) ;
#97920 = AXIS2_PLACEMENT_3D ( 'NONE', #96826, #78512, #58226 ) ;
#97921 = EDGE_CURVE ( 'NONE', #95937, #118189, #55642, .T. ) ;
#97922 = ORIENTED_EDGE ( 'NONE', *, *, #38676, .T. ) ;
#97923 = EDGE_CURVE ( 'NONE', #94609, #24381, #125785, .T. ) ;
#97924 = EDGE_LOOP ( 'NONE', ( #74900, #106861 ) ) ;
#97925 =( GEOMETRIC_REPRESENTATION_CONTEXT ( 3 ) GLOBAL_UNCERTAINTY_ASSIGNED_CONTEXT ( ( #129187 ) ) GLOBAL_UNIT_ASSIGNED_CONTEXT ( ( #57700, #66852, #8563 ) ) REPRESENTATION_CONTEXT ( 'NONE', 'WORKASPACE' ) );
#97926 = DIRECTION ( 'NONE',  ( -0.000000000000000000, -1.000000000000000000, -0.000000000000000000 ) ) ;
#97927 = DIRECTION ( 'NONE',  ( 0.000000000000000000, 1.000000000000000000, 0.000000000000000000 ) ) ;
#97928 = DIRECTION ( 'NONE',  ( 0.000000000000000000, 1.000000000000000000, 0.000000000000000000 ) ) ;
#97929 = VERTEX_POINT ( 'NONE', #14987 ) ;
#97930 = CIRCLE ( 'NONE', #81306, 0.06509327318403741736 ) ;
#97931 = ADVANCED_FACE ( 'NONE', ( #96786 ), #53502, .T. ) ;
#97932 = VERTEX_POINT ( 'NONE', #75863 ) ;
#97933 = LINE ( 'NONE', #61898, #55988 ) ;
#97934 = AXIS2_PLACEMENT_3D ( 'NONE', #17824, #47948, #87847 ) ;
#97935 = DIRECTION ( 'NONE',  ( 0.000000000000000000, 0.000000000000000000, 1.000000000000000000 ) ) ;
#97936 = CARTESIAN_POINT ( 'NONE',  ( -14.34999999999998543, 2.500000000000000000, 1.918653347947325338 ) ) ;
#97937 = ORIENTED_EDGE ( 'NONE', *, *, #62451, .T. ) ;
#97938 = ORIENTED_EDGE ( 'NONE', *, *, #79808, .T. ) ;
#97939 = CARTESIAN_POINT ( 'NONE',  ( 7.049999999999928768, 12.50000000000000000, -2.165063509461101710 ) ) ;
#97940 = VECTOR ( 'NONE', #89208, 1000.000000000000000 ) ;
#97941 = ORIENTED_EDGE ( 'NONE', *, *, #78020, .F. ) ;
#97942 = CARTESIAN_POINT ( 'NONE',  ( -4.350000000000023626, 2.500000000000000000, -1.918653347947325782 ) ) ;
#97943 = CARTESIAN_POINT ( 'NONE',  ( -7.700000000000010836, 2.500000000000000000, 3.883716857408421319 ) ) ;
#97944 = ORIENTED_EDGE ( 'NONE', *, *, #107795, .T. ) ;
#97945 = DIRECTION ( 'NONE',  ( 0.000000000000000000, 0.000000000000000000, 1.000000000000000000 ) ) ;
#97946 = FACE_OUTER_BOUND ( 'NONE', #59670, .T. ) ;
#97947 = CARTESIAN_POINT ( 'NONE',  ( 13.34999999999989662, 2.500000000000000000, -1.472243186433550122 ) ) ;
#97948 = AXIS2_PLACEMENT_3D ( 'NONE', #12864, #54105, #45582 ) ;
#97949 = EDGE_CURVE ( 'NONE', #110675, #70171, #109938, .T. ) ;
#97950 = CARTESIAN_POINT ( 'NONE',  ( -14.19999999999998685, 2.500000000000000000, -1.084202172485504434E-16 ) ) ;
#97951 = ORIENTED_EDGE ( 'NONE', *, *, #60956, .T. ) ;
#97952 = DIRECTION ( 'NONE',  ( 0.000000000000000000, 0.000000000000000000, -1.000000000000000000 ) ) ;
#97954 = AXIS2_PLACEMENT_3D ( 'NONE', #116979, #105895, #107166 ) ;
#97953 = VECTOR ( 'NONE', #65027, 1000.000000000000000 ) ;
#97955 = VERTEX_POINT ( 'NONE', #97443 ) ;
#97956 = EDGE_LOOP ( 'NONE', ( #97420, #42707 ) ) ;
#97957 = CARTESIAN_POINT ( 'NONE',  ( 5.599999999999933031, 12.50000000000000000, 0.2813168883297361700 ) ) ;
#97958 = DIRECTION ( 'NONE',  ( 0.000000000000000000, 1.000000000000000000, 0.000000000000000000 ) ) ;
#97959 = DIRECTION ( 'NONE',  ( -4.274815082592931898E-19, -0.9999939076577903929, -0.003490651415223739937 ) ) ;
#97960 = CARTESIAN_POINT ( 'NONE',  ( 11.44999999999990514, 2.500000000000000000, 2.511473670974873507 ) ) ;
#97961 = CARTESIAN_POINT ( 'NONE',  ( -11.05000000000000071, 2.500000000000000000, 2.511473670974873507 ) ) ;
#97962 = CARTESIAN_POINT ( 'NONE',  ( -12.09999999999999609, 12.50000000000000000, -0.6928203230275501445 ) ) ;
#97964 = ADVANCED_FACE ( 'NONE', ( #77790 ), #115794, .T. ) ;
#97963 = DIRECTION ( 'NONE',  ( 0.000000000000000000, 0.000000000000000000, 1.000000000000000000 ) ) ;
#97965 = DIRECTION ( 'NONE',  ( 0.000000000000000000, 0.000000000000000000, 1.000000000000000000 ) ) ;
#97966 = CARTESIAN_POINT ( 'NONE',  ( 9.149999999999915090, 2.500000000000000000, 6.595190528383296780 ) ) ;
#97967 = AXIS2_PLACEMENT_3D ( 'NONE', #61675, #110747, #21080 ) ;
#97968 = DIRECTION ( 'NONE',  ( -0.000000000000000000, -1.000000000000000000, -0.000000000000000000 ) ) ;
#97969 = CIRCLE ( 'NONE', #14425, 0.06509327318403741736 ) ;
#97970 = CIRCLE ( 'NONE', #68725, 0.06509327318403745899 ) ;
#97971 = VERTEX_POINT ( 'NONE', #117706 ) ;
#97972 = VECTOR ( 'NONE', #36469, 1000.000000000000000 ) ;
#97973 = CARTESIAN_POINT ( 'NONE',  ( 10.64999999999991331, 12.50000000000000000, -1.818653347947325916 ) ) ;
#97974 = EDGE_CURVE ( 'NONE', #36786, #52806, #54936, .T. ) ;
#97975 = FACE_OUTER_BOUND ( 'NONE', #62873, .T. ) ;
#97976 = CARTESIAN_POINT ( 'NONE',  ( 9.349999999999916156, 2.500000000000000000, 6.148780366869520009 ) ) ;
#97977 = FACE_OUTER_BOUND ( 'NONE', #36891, .T. ) ;
#97978 = DIRECTION ( 'NONE',  ( 0.000000000000000000, 0.000000000000000000, -1.000000000000000000 ) ) ;
#97979 = AXIS2_PLACEMENT_3D ( 'NONE', #36768, #28227, #16441 ) ;
#97980 = ORIENTED_EDGE ( 'NONE', *, *, #98186, .T. ) ;
#97981 = AXIS2_PLACEMENT_3D ( 'NONE', #61430, #82358, #119673 ) ;
#97982 = CARTESIAN_POINT ( 'NONE',  ( 7.099999999999928590, 2.500000000000000000, 3.737306695894644371 ) ) ;
#97983 = FACE_OUTER_BOUND ( 'NONE', #39769, .T. ) ;
#97985 = ORIENTED_EDGE ( 'NONE', *, *, #113262, .T. ) ;
#97984 = DIRECTION ( 'NONE',  ( 0.000000000000000000, 0.000000000000000000, 1.000000000000000000 ) ) ;
#97986 = VECTOR ( 'NONE', #74361, 1000.000000000000000 ) ;
#97987 = ORIENTED_EDGE ( 'NONE', *, *, #60039, .F. ) ;
#97988 = PLANE ( 'NONE',  #115715 ) ;
#97989 = VERTEX_POINT ( 'NONE', #26139 ) ;
#97990 = ORIENTED_EDGE ( 'NONE', *, *, #24128, .T. ) ;
#97991 = EDGE_LOOP ( 'NONE', ( #30365, #63378, #109863, #71200 ) ) ;
#97992 = FACE_OUTER_BOUND ( 'NONE', #75672, .T. ) ;
#97993 = CARTESIAN_POINT ( 'NONE',  ( 3.549999999999942091, 2.500000000000000000, 2.511473670974873507 ) ) ;
#97994 = CARTESIAN_POINT ( 'NONE',  ( -4.800000000000024691, 2.500000000000000000, 4.676537180435972552 ) ) ;
#97995 = DIRECTION ( 'NONE',  ( -4.274815082592931898E-19, -0.9999939076577903929, -0.003490651415223739937 ) ) ;
#97996 = AXIS2_PLACEMENT_3D ( 'NONE', #11618, #69904, #19502 ) ;
#97997 = EDGE_LOOP ( 'NONE', ( #40525, #125671 ) ) ;
#97998 = ADVANCED_FACE ( 'NONE', ( #9062 ), #59493, .T. ) ;
#97999 = DIRECTION ( 'NONE',  ( 0.000000000000000000, 1.000000000000000000, 0.000000000000000000 ) ) ;
#98000 = ORIENTED_EDGE ( 'NONE', *, *, #34177, .F. ) ;
#98001 = AXIS2_PLACEMENT_3D ( 'NONE', #87817, #117263, #97653 ) ;
#98002 = DIRECTION ( 'NONE',  ( 0.000000000000000000, -0.000000000000000000, 1.000000000000000000 ) ) ;
#98003 = CARTESIAN_POINT ( 'NONE',  ( 16.31260002278194321, -1.499999999999773515, -6.357732714000996488 ) ) ;
#98004 = CARTESIAN_POINT ( 'NONE',  ( 19.40342015654644925, 2.551666867760719715, 4.359384978533469734 ) ) ;
#98005 = CARTESIAN_POINT ( 'NONE',  ( -2.900000000000029665, 12.50000000000000000, 3.702399969078682407 ) ) ;
#98006 = CARTESIAN_POINT ( 'NONE',  ( -3.749999999999991118, 2.500000000000000000, -2.165063509461101710 ) ) ;
#98007 = ORIENTED_EDGE ( 'NONE', *, *, #82930, .T. ) ;
#98008 = ORIENTED_EDGE ( 'NONE', *, *, #20431, .T. ) ;
#98009 = ORIENTED_EDGE ( 'NONE', *, *, #56452, .T. ) ;
#98010 = ORIENTED_EDGE ( 'NONE', *, *, #121149, .F. ) ;
#98011 = ORIENTED_EDGE ( 'NONE', *, *, #26245, .T. ) ;
#98012 = DIRECTION ( 'NONE',  ( 0.000000000000000000, -0.000000000000000000, 1.000000000000000000 ) ) ;
#98013 = DIRECTION ( 'NONE',  ( 0.000000000000000000, 1.000000000000000000, 0.000000000000000000 ) ) ;
#98014 = ADVANCED_FACE ( 'NONE', ( #29368 ), #18878, .T. ) ;
#98015 = EDGE_CURVE ( 'NONE', #84709, #94668, #74516, .T. ) ;
#98016 = CARTESIAN_POINT ( 'NONE',  ( -2.500000000000031086, 2.500000000000000000, 3.537306695894645081 ) ) ;
#98017 = EDGE_CURVE ( 'NONE', #99630, #80752, #58188, .T. ) ;
#98018 = FACE_BOUND ( 'NONE', #98782, .T. ) ;
#98019 = EDGE_CURVE ( 'NONE', #60331, #96594, #93297, .T. ) ;
#98020 = DIRECTION ( 'NONE',  ( 0.000000000000000000, 0.000000000000000000, 1.000000000000000000 ) ) ;
#98021 = CARTESIAN_POINT ( 'NONE',  ( 186.5729166673494603, 4.445597072760120838, -7.699999999999998401 ) ) ;
#98022 = AXIS2_PLACEMENT_3D ( 'NONE', #105010, #64452, #122101 ) ;
#98023 = CARTESIAN_POINT ( 'NONE',  ( -1.450000000000035039, 2.500000000000000000, -6.841600689897077814 ) ) ;
#98024 = DIRECTION ( 'NONE',  ( 0.000000000000000000, -0.000000000000000000, 1.000000000000000000 ) ) ;
#98025 = VECTOR ( 'NONE', #89000, 1000.000000000000000 ) ;
#98026 = EDGE_CURVE ( 'NONE', #20666, #98359, #18067, .T. ) ;
#98027 = CARTESIAN_POINT ( 'NONE',  ( 185.9635416670080588, -4.367472073101520635, 7.564683531249999149 ) ) ;
#98028 = CARTESIAN_POINT ( 'NONE',  ( 10.19999999999991225, 12.50000000000000000, 3.918623584224382839 ) ) ;
#98029 = AXIS2_PLACEMENT_3D ( 'NONE', #52055, #69748, #20016 ) ;
#98030 = EDGE_CURVE ( 'NONE', #21459, #76682, #18235, .T. ) ;
#98031 = CARTESIAN_POINT ( 'NONE',  ( 14.39999999999989555, 12.50000000000000000, 0.2813168883297362810 ) ) ;
#98032 = EDGE_CURVE ( 'NONE', #52139, #88048, #88247, .T. ) ;
#98033 = EDGE_CURVE ( 'NONE', #128319, #37369, #79114, .T. ) ;
#98034 = PLANE ( 'NONE',  #107906 ) ;
#98035 = CIRCLE ( 'NONE', #22850, 0.06509327318403745899 ) ;
#98036 = ORIENTED_EDGE ( 'NONE', *, *, #67891, .F. ) ;
#98037 = EDGE_LOOP ( 'NONE', ( #82643, #73272, #17648, #96685 ) ) ;
#98038 = EDGE_LOOP ( 'NONE', ( #92878, #117366 ) ) ;
#98039 = ORIENTED_EDGE ( 'NONE', *, *, #100556, .T. ) ;
#98040 = VECTOR ( 'NONE', #40273, 1000.000000000000000 ) ;
#98041 = PRODUCT_DEFINITION ( 'UNKNOWN', '', #69288, #36291 ) ;
#98042 = CARTESIAN_POINT ( 'NONE',  ( -6.850000000000017408, 2.500000000000000000, -2.411473670974877859 ) ) ;
#98043 = FACE_BOUND ( 'NONE', #19598, .T. ) ;
#98044 = EDGE_CURVE ( 'NONE', #27644, #127171, #9669, .T. ) ;
#98045 = DIRECTION ( 'NONE',  ( 0.000000000000000000, 1.000000000000000000, 0.000000000000000000 ) ) ;
#98046 = AXIS2_PLACEMENT_3D ( 'NONE', #67068, #115536, #97841 ) ;
#98047 = EDGE_LOOP ( 'NONE', ( #69318, #63478, #40696, #74252, #105983, #1966, #91336, #63016, #90366, #13720, #57437, #67202, #15731, #65058 ) ) ;
#98048 = CARTESIAN_POINT ( 'NONE',  ( -9.350000000000008527, 12.50000000000000000, -6.213873640053559022 ) ) ;
#98049 = DIRECTION ( 'NONE',  ( 0.000000000000000000, 0.000000000000000000, 1.000000000000000000 ) ) ;
#98050 = DIRECTION ( 'NONE',  ( 0.000000000000000000, 0.000000000000000000, -1.000000000000000000 ) ) ;
#98051 = VERTEX_POINT ( 'NONE', #108560 ) ;
#98052 = CARTESIAN_POINT ( 'NONE',  ( 187.5000000000000000, -1.065442715258197248E-15, 8.699999999999999289 ) ) ;
#98053 = CARTESIAN_POINT ( 'NONE',  ( -0.6000000000000388356, 12.50000000000000000, 4.676537180435972552 ) ) ;
#98054 = ORIENTED_EDGE ( 'NONE', *, *, #99508, .T. ) ;
#98055 = ORIENTED_EDGE ( 'NONE', *, *, #53322, .T. ) ;
#98056 = AXIS2_PLACEMENT_3D ( 'NONE', #42874, #111582, #22582 ) ;
#98057 = DIRECTION ( 'NONE',  ( 0.000000000000000000, -0.000000000000000000, 1.000000000000000000 ) ) ;
#98058 = PLANE ( 'NONE',  #89481 ) ;
#98059 = CIRCLE ( 'NONE', #93960, 0.1000000000000002554 ) ;
#98060 = DIRECTION ( 'NONE',  ( 0.000000000000000000, 1.000000000000000000, 0.000000000000000000 ) ) ;
#98061 = AXIS2_PLACEMENT_3D ( 'NONE', #85719, #15024, #104087 ) ;
#98062 = DIRECTION ( 'NONE',  ( 0.000000000000000000, 0.000000000000000000, 1.000000000000000000 ) ) ;
#98063 = DIRECTION ( 'NONE',  ( 0.000000000000000000, 1.000000000000000000, 0.000000000000000000 ) ) ;
#98064 = ORIENTED_EDGE ( 'NONE', *, *, #4214, .F. ) ;
#98065 = ORIENTED_EDGE ( 'NONE', *, *, #128317, .F. ) ;
#98066 = FACE_OUTER_BOUND ( 'NONE', #30629, .T. ) ;
#98068 = EDGE_LOOP ( 'NONE', ( #102007, #68167, #74075, #33827 ) ) ;
#98067 = CIRCLE ( 'NONE', #102201, 0.06509327318403745899 ) ;
#98069 = CARTESIAN_POINT ( 'NONE',  ( 3.149999999999946176, 12.50000000000000000, -6.906693963081115051 ) ) ;
#98070 = FACE_BOUND ( 'NONE', #92098, .T. ) ;
#98071 = CONICAL_SURFACE ( 'NONE', #70979, 0.1000000000000002554, 0.003490658503988666988 ) ;
#98072 = ADVANCED_FACE ( 'NONE', ( #10976 ), #30619, .T. ) ;
#98073 = AXIS2_PLACEMENT_3D ( 'NONE', #111950, #13067, #73948 ) ;
#98074 = ORIENTED_EDGE ( 'NONE', *, *, #102292, .F. ) ;
#98076 = EDGE_CURVE ( 'NONE', #102847, #79650, #120487, .T. ) ;
#98075 = CARTESIAN_POINT ( 'NONE',  ( 112.9334202320777365, 7.656891339828185039, 0.8302582904282872489 ) ) ;
#98077 = VERTEX_POINT ( 'NONE', #38557 ) ;
#98078 = FACE_OUTER_BOUND ( 'NONE', #7678, .T. ) ;
#98079 = DIRECTION ( 'NONE',  ( -0.000000000000000000, 1.000000000000000000, -0.000000000000000000 ) ) ;
#98080 = LINE ( 'NONE', #8401, #115575 ) ;
#98081 = LINE ( 'NONE', #86316, #41210 ) ;
#98082 = CIRCLE ( 'NONE', #102306, 0.1000000000000002554 ) ;
#98083 = ORIENTED_EDGE ( 'NONE', *, *, #129182, .F. ) ;
#98084 = EDGE_CURVE ( 'NONE', #77768, #53425, #26407, .T. ) ;
#98085 = EDGE_LOOP ( 'NONE', ( #32477, #122797, #11436, #82319 ) ) ;
#98087 = ORIENTED_EDGE ( 'NONE', *, *, #87826, .T. ) ;
#98086 = AXIS2_PLACEMENT_3D ( 'NONE', #22822, #62741, #20872 ) ;
#98088 = CARTESIAN_POINT ( 'NONE',  ( 2.099999999999947686, 2.500000000000000000, 5.022947341949748790 ) ) ;
#98089 = DIRECTION ( 'NONE',  ( -0.000000000000000000, 1.000000000000000000, -0.000000000000000000 ) ) ;
#98090 = CARTESIAN_POINT ( 'NONE',  ( 1.449999999999952660, 2.500000000000000000, -6.941600689897078347 ) ) ;
#98092 = VERTEX_POINT ( 'NONE', #49659 ) ;
#98091 = ORIENTED_EDGE ( 'NONE', *, *, #22743, .F. ) ;
#98093 = ORIENTED_EDGE ( 'NONE', *, *, #82251, .F. ) ;
#98094 = DIRECTION ( 'NONE',  ( -0.000000000000000000, -1.000000000000000000, -0.000000000000000000 ) ) ;
#98095 = DIRECTION ( 'NONE',  ( 0.000000000000000000, 0.000000000000000000, 1.000000000000000000 ) ) ;
#98096 = APPLICATION_PROTOCOL_DEFINITION ( 'draft international standard', 'automotive_design', 1998, #84818 ) ;
#98097 = DIRECTION ( 'NONE',  ( 0.000000000000000000, 1.000000000000000000, 0.000000000000000000 ) ) ;
#98098 = CARTESIAN_POINT ( 'NONE',  ( -0.8500000000000390576, 12.50000000000000000, -6.430097255199264339 ) ) ;
#98099 = CARTESIAN_POINT ( 'NONE',  ( -6.650000000000014566, 2.500000000000000000, 5.802370205355744659 ) ) ;
#98100 = DIRECTION ( 'NONE',  ( 0.000000000000000000, -0.9999939076577903929, 0.003490651415223739937 ) ) ;
#98101 = AXIS2_PLACEMENT_3D ( 'NONE', #105658, #97117, #8084 ) ;
#98102 = DIRECTION ( 'NONE',  ( 0.000000000000000000, 0.000000000000000000, -1.000000000000000000 ) ) ;
#98103 = DIRECTION ( 'NONE',  ( -0.000000000000000000, 1.000000000000000000, -0.000000000000000000 ) ) ;
#98104 = ORIENTED_EDGE ( 'NONE', *, *, #58155, .F. ) ;
#98105 = ORIENTED_EDGE ( 'NONE', *, *, #91998, .T. ) ;
#98106 = DIRECTION ( 'NONE',  ( 0.000000000000000000, -0.000000000000000000, 1.000000000000000000 ) ) ;
#98107 = CARTESIAN_POINT ( 'NONE',  ( 0.8499999999999545697, 2.500000000000000000, -1.472243186433550122 ) ) ;
#98108 = VERTEX_POINT ( 'NONE', #89560 ) ;
#98109 = ORIENTED_EDGE ( 'NONE', *, *, #54703, .F. ) ;
#98110 = CARTESIAN_POINT ( 'NONE',  ( 186.2760416670080588, 6.551208109652274736, 3.782341765625001351 ) ) ;
#98111 = CARTESIAN_POINT ( 'NONE',  ( 7.699999999999923794, 2.500000000000000000, -3.983716857408426293 ) ) ;
#98112 = CIRCLE ( 'NONE', #14468, 0.06509327318403745899 ) ;
#98113 = CARTESIAN_POINT ( 'NONE',  ( 2.500000000000001332, 2.392226903609813160, -9.521986658763280431 ) ) ;
#98114 = DIRECTION ( 'NONE',  ( -0.000000000000000000, -1.000000000000000000, -0.000000000000000000 ) ) ;
#98115 = DIRECTION ( 'NONE',  ( 0.000000000000000000, 0.000000000000000000, -1.000000000000000000 ) ) ;
#98116 = CARTESIAN_POINT ( 'NONE',  ( -3.100000000000028511, 2.500000000000000000, 0.3464101615137736845 ) ) ;
#98117 = ORIENTED_EDGE ( 'NONE', *, *, #114119, .F. ) ;
#98118 = DIRECTION ( 'NONE',  ( 0.000000000000000000, 1.000000000000000000, 0.000000000000000000 ) ) ;
#98119 = CIRCLE ( 'NONE', #119062, 0.06509327318403745899 ) ;
#98120 = DIRECTION ( 'NONE',  ( 0.000000000000000000, 1.000000000000000000, 0.000000000000000000 ) ) ;
#98121 = ORIENTED_EDGE ( 'NONE', *, *, #36990, .T. ) ;
#98123 = AXIS2_PLACEMENT_3D ( 'NONE', #36553, #58755, #7701 ) ;
#98122 = AXIS2_PLACEMENT_3D ( 'NONE', #58708, #76420, #9603 ) ;
#98124 = ORIENTED_EDGE ( 'NONE', *, *, #50326, .T. ) ;
#98125 = EDGE_CURVE ( 'NONE', #49878, #1609, #64050, .T. ) ;
#98126 = AXIS2_PLACEMENT_3D ( 'NONE', #103041, #93240, #76818 ) ;
#98127 = ORIENTED_EDGE ( 'NONE', *, *, #112479, .T. ) ;
#98129 = EDGE_LOOP ( 'NONE', ( #108662, #111727 ) ) ;
#98128 = ADVANCED_FACE ( 'NONE', ( #50942 ), #81042, .T. ) ;
#98130 = LINE ( 'NONE', #96836, #39952 ) ;
#98131 = DIRECTION ( 'NONE',  ( 0.000000000000000000, -0.9999939076577903929, 0.003490651415223739937 ) ) ;
#98133 = ORIENTED_EDGE ( 'NONE', *, *, #32919, .T. ) ;
#98132 = CONICAL_SURFACE ( 'NONE', #102358, 0.09999999999999999167, 0.003490658503988666988 ) ;
#98134 = FACE_OUTER_BOUND ( 'NONE', #16768, .T. ) ;
#98135 = DIRECTION ( 'NONE',  ( 0.000000000000000000, 0.000000000000000000, -1.000000000000000000 ) ) ;
#98136 = CARTESIAN_POINT ( 'NONE',  ( -6.505213034913026604E-15, 12.50000000000000000, 4.330127018922196314 ) ) ;
#98138 = EDGE_LOOP ( 'NONE', ( #14560, #12479, #113685, #42062 ) ) ;
#98137 = DIRECTION ( 'NONE',  ( 1.000000000000000000, 0.000000000000000000, 0.000000000000000000 ) ) ;
#98139 = EDGE_CURVE ( 'NONE', #80664, #33748, #90182, .T. ) ;
#98140 = DIRECTION ( 'NONE',  ( -4.274815082592931898E-19, -0.9999939076577903929, -0.003490651415223739937 ) ) ;
#98141 = CARTESIAN_POINT ( 'NONE',  ( 0.5999999999999560130, 12.50000000000000000, -3.983716857408426293 ) ) ;
#98142 = VERTEX_POINT ( 'NONE', #58818 ) ;
#98143 = VERTEX_POINT ( 'NONE', #520 ) ;
#98144 = EDGE_LOOP ( 'NONE', ( #58602, #76497 ) ) ;
#98145 = AXIS2_PLACEMENT_3D ( 'NONE', #106903, #7409, #28366 ) ;
#98146 = FACE_OUTER_BOUND ( 'NONE', #117151, .T. ) ;
#98147 = DIRECTION ( 'NONE',  ( 0.000000000000000000, -0.9999939076577903929, 0.003490651415223739937 ) ) ;
#98148 = AXIS2_PLACEMENT_3D ( 'NONE', #12658, #4127, #52596 ) ;
#98149 = AXIS2_PLACEMENT_3D ( 'NONE', #58699, #26664, #98595 ) ;
#98150 = EDGE_CURVE ( 'NONE', #116591, #38872, #89098, .T. ) ;
#98151 = ORIENTED_EDGE ( 'NONE', *, *, #65545, .F. ) ;
#98152 = CARTESIAN_POINT ( 'NONE',  ( -1.650000000000035216, 2.500000000000000000, -1.372243186433550033 ) ) ;
#98153 = CARTESIAN_POINT ( 'NONE',  ( -9.200000000000006395, 2.500000000000000000, 4.430127018922196847 ) ) ;
#98154 = DIRECTION ( 'NONE',  ( 0.000000000000000000, -0.9999939076577903929, 0.003490651415223739937 ) ) ;
#98155 = DIRECTION ( 'NONE',  ( -0.000000000000000000, 1.000000000000000000, -0.000000000000000000 ) ) ;
#98157 = CONICAL_SURFACE ( 'NONE', #114884, 0.1000000000000002554, 0.003490658503988666988 ) ;
#98156 = AXIS2_PLACEMENT_3D ( 'NONE', #49516, #89425, #119519 ) ;
#98158 = EDGE_CURVE ( 'NONE', #47149, #114968, #92797, .T. ) ;
#98159 = ORIENTED_EDGE ( 'NONE', *, *, #118438, .F. ) ;
#98160 = CIRCLE ( 'NONE', #12187, 0.09999999999999982514 ) ;
#98161 = DIRECTION ( 'NONE',  ( 0.000000000000000000, 0.000000000000000000, 1.000000000000000000 ) ) ;
#98162 = EDGE_LOOP ( 'NONE', ( #93649, #66336, #39558, #48578 ) ) ;
#98163 = ORIENTED_EDGE ( 'NONE', *, *, #64374, .T. ) ;
#98164 = DIRECTION ( 'NONE',  ( 0.000000000000000000, -0.000000000000000000, 1.000000000000000000 ) ) ;
#98165 = ADVANCED_FACE ( 'NONE', ( #53516 ), #51586, .T. ) ;
#98166 = EDGE_CURVE ( 'NONE', #41996, #74009, #16006, .T. ) ;
#98167 = CARTESIAN_POINT ( 'NONE',  ( -4.400000000000025224, 2.500000000000000000, 4.083716857408420609 ) ) ;
#98168 = ADVANCED_FACE ( 'NONE', ( #63319 ), #59877, .T. ) ;
#98169 = FACE_BOUND ( 'NONE', #19532, .T. ) ;
#98170 = EDGE_CURVE ( 'NONE', #120218, #47149, #51544, .T. ) ;
#98171 = CARTESIAN_POINT ( 'NONE',  ( -3.100000000000028955, 12.50000000000000000, 4.676537180435972552 ) ) ;
#98172 = DIRECTION ( 'NONE',  ( -0.000000000000000000, 1.000000000000000000, -0.000000000000000000 ) ) ;
#98173 = DIRECTION ( 'NONE',  ( 0.000000000000000000, 1.000000000000000000, 0.000000000000000000 ) ) ;
#98174 = AXIS2_PLACEMENT_3D ( 'NONE', #29105, #19921, #88650 ) ;
#98175 = ADVANCED_FACE ( 'NONE', ( #123518, #33856, #44320, #81668, #3123 ), #43073, .F. ) ;
#98176 = ORIENTED_EDGE ( 'NONE', *, *, #124974, .F. ) ;
#98177 = CARTESIAN_POINT ( 'NONE',  ( -14.99999999999998401, 2.500000000000000000, 0.6928203230275518099 ) ) ;
#98178 = DIRECTION ( 'NONE',  ( 0.000000000000000000, 0.000000000000000000, 1.000000000000000000 ) ) ;
#98179 = EDGE_CURVE ( 'NONE', #14963, #44951, #122550, .T. ) ;
#98180 = CARTESIAN_POINT ( 'NONE',  ( 11.04999999999991189, 12.50000000000000000, -2.511473670974877948 ) ) ;
#98181 = CARTESIAN_POINT ( 'NONE',  ( 187.5000000000000000, -1.500000000000000000, -6.000000000000000000 ) ) ;
#98182 = ORIENTED_EDGE ( 'NONE', *, *, #84990, .F. ) ;
#98183 = CIRCLE ( 'NONE', #83627, 0.06509327318403743123 ) ;
#98184 = DIRECTION ( 'NONE',  ( 0.000000000000000000, 1.000000000000000000, 0.000000000000000000 ) ) ;
#98185 = EDGE_CURVE ( 'NONE', #111368, #22839, #128924, .T. ) ;
#98186 = EDGE_CURVE ( 'NONE', #12644, #24551, #91241, .T. ) ;
#98187 = CARTESIAN_POINT ( 'NONE',  ( 5.649999999999936406, 2.500000000000000000, -6.148780366869526226 ) ) ;
#98188 = AXIS2_PLACEMENT_3D ( 'NONE', #120627, #48673, #79431 ) ;
#98189 = VERTEX_POINT ( 'NONE', #113719 ) ;
#98190 = ORIENTED_EDGE ( 'NONE', *, *, #117521, .F. ) ;
#98191 = CARTESIAN_POINT ( 'NONE',  ( 4.549999999999939426, 2.500000000000000000, -6.495190528383302464 ) ) ;
#98192 = DIRECTION ( 'NONE',  ( 0.000000000000000000, -0.000000000000000000, 1.000000000000000000 ) ) ;
#98193 = FACE_BOUND ( 'NONE', #96955, .T. ) ;
#98194 = ADVANCED_FACE ( 'NONE', ( #122258 ), #11812, .T. ) ;
#98195 = CARTESIAN_POINT ( 'NONE',  ( 11.44999999999990692, 12.50000000000000000, -6.841600689897078702 ) ) ;
#98196 = EDGE_LOOP ( 'NONE', ( #26292, #27094 ) ) ;
#98197 = DIRECTION ( 'NONE',  ( 0.000000000000000000, 1.000000000000000000, 0.000000000000000000 ) ) ;
#98198 = ORIENTED_EDGE ( 'NONE', *, *, #124325, .F. ) ;
#98199 = ORIENTED_EDGE ( 'NONE', *, *, #44391, .F. ) ;
#98200 = DIRECTION ( 'NONE',  ( 0.000000000000000000, 0.000000000000000000, 1.000000000000000000 ) ) ;
#98201 = CARTESIAN_POINT ( 'NONE',  ( 185.8333333333333144, 6.668395609140177704, -3.849999999999998312 ) ) ;
#98202 = EDGE_LOOP ( 'NONE', ( #69908, #77875 ) ) ;
#98203 = CARTESIAN_POINT ( 'NONE',  ( 0.6499999999999566125, 2.500000000000000000, -6.941600689897077459 ) ) ;
#98204 = FACE_OUTER_BOUND ( 'NONE', #73643, .T. ) ;
#98205 = PLANE ( 'NONE',  #44262 ) ;
#98206 = AXIS2_PLACEMENT_3D ( 'NONE', #125602, #16287, #115795 ) ;
#98207 = LINE ( 'NONE', #9834, #84440 ) ;
#98208 = ORIENTED_EDGE ( 'NONE', *, *, #60773, .T. ) ;
#98209 = DIRECTION ( 'NONE',  ( 0.000000000000000000, 0.000000000000000000, -1.000000000000000000 ) ) ;
#98211 = CONICAL_SURFACE ( 'NONE', #12, 0.1000000000000002554, 0.003490658503988666988 ) ;
#98210 = CIRCLE ( 'NONE', #33403, 0.1000000000000002554 ) ;
#98212 = DIRECTION ( 'NONE',  ( 0.000000000000000000, 0.000000000000000000, 1.000000000000000000 ) ) ;
#98213 = CARTESIAN_POINT ( 'NONE',  ( 1.249999999999952038, 2.500000000000000000, -1.572243186433550211 ) ) ;
#98214 = CARTESIAN_POINT ( 'NONE',  ( 21.25104878433765876, -0.2455272941117648267, -4.189300629080492833 ) ) ;
#98215 = ORIENTED_EDGE ( 'NONE', *, *, #108251, .T. ) ;
#98216 = DIRECTION ( 'NONE',  ( 0.000000000000000000, 0.000000000000000000, 1.000000000000000000 ) ) ;
#98217 = VERTEX_POINT ( 'NONE', #112437 ) ;
#98218 = DIRECTION ( 'NONE',  ( -0.000000000000000000, 1.000000000000000000, -0.000000000000000000 ) ) ;
#98219 = EDGE_LOOP ( 'NONE', ( #30326, #44091, #96423, #84532 ) ) ;
#98220 = CARTESIAN_POINT ( 'NONE',  ( -6.250000000000019540, 2.500000000000000000, -2.857883832488653741 ) ) ;
#98223 = CARTESIAN_POINT ( 'NONE',  ( 17.50000000000000000, -2.499999999999999556, -1.666666666666662300 ) ) ;
#98222 = CONICAL_SURFACE ( 'NONE', #41821, 0.09999999999999982514, 0.003490658503988666988 ) ;
#98221 = CIRCLE ( 'NONE', #127486, 0.1000000000000002554 ) ;
#98224 = EDGE_CURVE ( 'NONE', #50587, #105674, #36867, .T. ) ;
#98225 = DIRECTION ( 'NONE',  ( 0.000000000000000000, -0.9999939076577903929, 0.003490651415223739937 ) ) ;
#98226 = DIRECTION ( 'NONE',  ( 0.000000000000000000, 0.000000000000000000, 1.000000000000000000 ) ) ;
#98227 = ORIENTED_EDGE ( 'NONE', *, *, #91837, .F. ) ;
#98229 = EDGE_CURVE ( 'NONE', #60288, #26496, #110031, .T. ) ;
#98228 = DIRECTION ( 'NONE',  ( 0.000000000000000000, 0.000000000000000000, 1.000000000000000000 ) ) ;
#98230 = DIRECTION ( 'NONE',  ( -0.000000000000000000, -1.000000000000000000, -0.000000000000000000 ) ) ;
#98231 = CARTESIAN_POINT ( 'NONE',  ( 87.50000000000001421, 3.974992050023848922, -6.359987280038160051 ) ) ;
#98232 = CARTESIAN_POINT ( 'NONE',  ( 185.1093750003413732, 9.264065473108010111E-16, -7.564683531250000925 ) ) ;
#98233 = CARTESIAN_POINT ( 'NONE',  ( -12.89999999999999325, 12.50000000000000000, -3.637306695894647390 ) ) ;
#98234 = CARTESIAN_POINT ( 'NONE',  ( 162.5000000000000000, 0.5000000000000000000, -7.500000000000005329 ) ) ;
#98235 = ORIENTED_EDGE ( 'NONE', *, *, #118658, .F. ) ;
#98236 = VERTEX_POINT ( 'NONE', #22137 ) ;
#98237 = CARTESIAN_POINT ( 'NONE',  ( -11.84999999999999609, 2.500000000000000000, 6.148780366869520897 ) ) ;
#98238 = VERTEX_POINT ( 'NONE', #3757 ) ;
#98239 = DIRECTION ( 'NONE',  ( 0.000000000000000000, 1.000000000000000000, 0.000000000000000000 ) ) ;
#98241 = ORIENTED_EDGE ( 'NONE', *, *, #4366, .F. ) ;
#98240 = EDGE_LOOP ( 'NONE', ( #107904, #79783 ) ) ;
#98242 = EDGE_LOOP ( 'NONE', ( #87785, #34241 ) ) ;
#98243 = CARTESIAN_POINT ( 'NONE',  ( 87.50000000000001421, 3.974992050023852475, -6.359987280038158275 ) ) ;
#98244 = AXIS2_PLACEMENT_3D ( 'NONE', #58828, #8420, #126283 ) ;
#98245 = FACE_OUTER_BOUND ( 'NONE', #106301, .T. ) ;
#98246 = CIRCLE ( 'NONE', #14607, 0.06509327318403745899 ) ;
#98247 = CARTESIAN_POINT ( 'NONE',  ( -10.85000000000000142, 2.500000000000000000, -2.957883832488649833 ) ) ;
#98248 =( LENGTH_UNIT ( ) NAMED_UNIT ( * ) SI_UNIT ( .MILLI., .METRE. ) );
#98249 = PLANE ( 'NONE',  #59840 ) ;
#98250 = DIRECTION ( 'NONE',  ( -4.274815082592931898E-19, -0.9999939076577903929, -0.003490651415223739937 ) ) ;
#98251 = DIRECTION ( 'NONE',  ( 0.000000000000000000, 0.000000000000000000, 1.000000000000000000 ) ) ;
#98252 = DIRECTION ( 'NONE',  ( -4.274815082592931898E-19, -0.9999939076577903929, -0.003490651415223739937 ) ) ;
#98254 = CONICAL_SURFACE ( 'NONE', #31379, 0.1000000000000002554, 0.003490658503988666988 ) ;
#98253 = DIRECTION ( 'NONE',  ( -0.000000000000000000, -1.000000000000000000, -0.000000000000000000 ) ) ;
#98255 = ORIENTED_EDGE ( 'NONE', *, *, #3023, .F. ) ;
#98256 = VERTEX_POINT ( 'NONE', #83621 ) ;
#98257 = ORIENTED_EDGE ( 'NONE', *, *, #19568, .T. ) ;
#98258 = FACE_OUTER_BOUND ( 'NONE', #14777, .T. ) ;
#98259 = EDGE_LOOP ( 'NONE', ( #11543, #59495, #9244, #73292 ) ) ;
#98260 = ORIENTED_EDGE ( 'NONE', *, *, #16995, .T. ) ;
#98261 = DIRECTION ( 'NONE',  ( 0.000000000000000000, -0.9999939076577903929, 0.003490651415223739937 ) ) ;
#98262 = CIRCLE ( 'NONE', #41854, 0.06509327318403745899 ) ;
#98264 = EDGE_CURVE ( 'NONE', #55968, #107226, #68240, .T. ) ;
#98263 = VECTOR ( 'NONE', #29571, 1000.000000000000000 ) ;
#98265 = DIRECTION ( 'NONE',  ( -0.000000000000000000, 1.000000000000000000, -0.000000000000000000 ) ) ;
#98266 = DIRECTION ( 'NONE',  ( 0.000000000000000000, 0.000000000000000000, 1.000000000000000000 ) ) ;
#98267 = CIRCLE ( 'NONE', #41859, 0.1000000000000002554 ) ;
#98268 = FACE_OUTER_BOUND ( 'NONE', #27225, .T. ) ;
#98269 = PLANE ( 'NONE',  #99430 ) ;
#98270 = DIRECTION ( 'NONE',  ( 0.000000000000000000, 0.000000000000000000, 1.000000000000000000 ) ) ;
#98271 = ORIENTED_EDGE ( 'NONE', *, *, #127003, .T. ) ;
#98272 = CARTESIAN_POINT ( 'NONE',  ( -11.69999999999999574, 2.500000000000000000, 4.330127018922196314 ) ) ;
#98273 = ORIENTED_EDGE ( 'NONE', *, *, #102788, .T. ) ;
#98274 = CARTESIAN_POINT ( 'NONE',  ( -11.44999999999999751, 2.500000000000000000, -6.841600689897074261 ) ) ;
#98275 = VERTEX_POINT ( 'NONE', #11644 ) ;
#98276 = DIRECTION ( 'NONE',  ( -0.000000000000000000, 1.000000000000000000, -0.000000000000000000 ) ) ;
#98277 = AXIS2_PLACEMENT_3D ( 'NONE', #21573, #121056, #49766 ) ;
#98278 = ORIENTED_EDGE ( 'NONE', *, *, #8145, .T. ) ;
#98279 = EDGE_CURVE ( 'NONE', #35495, #20160, #2448, .T. ) ;
#98280 = EDGE_CURVE ( 'NONE', #25512, #11963, #62049, .T. ) ;
#98281 = EDGE_LOOP ( 'NONE', ( #31827, #57812 ) ) ;
#98282 = CARTESIAN_POINT ( 'NONE',  ( 7.499999999999927169, 12.50000000000000000, -5.088040615133791356 ) ) ;
#98283 = CARTESIAN_POINT ( 'NONE',  ( -12.49999999999995914, 12.50000000000000000, 1.843143693225357538E-15 ) ) ;
#98284 = CARTESIAN_POINT ( 'NONE',  ( -6.850000000000013856, 2.500000000000000000, 2.511473670974873507 ) ) ;
#98285 = DIRECTION ( 'NONE',  ( 0.000000000000000000, 0.000000000000000000, 1.000000000000000000 ) ) ;
#98286 = FACE_OUTER_BOUND ( 'NONE', #11061, .T. ) ;
#98287 = VERTEX_POINT ( 'NONE', #22777 ) ;
#98288 = PLANE ( 'NONE',  #108465 ) ;
#98289 = CARTESIAN_POINT ( 'NONE',  ( 9.599999999999914380, 2.500000000000000000, -4.330127018922201643 ) ) ;
#98290 = ADVANCED_FACE ( 'NONE', ( #62693 ), #103766, .T. ) ;
#98291 = DIRECTION ( 'NONE',  ( 0.000000000000000000, 0.000000000000000000, 1.000000000000000000 ) ) ;
#98292 = CARTESIAN_POINT ( 'NONE',  ( 12.49999999999993960, 12.50000000000000000, 4.330127018922196314 ) ) ;
#98293 = FACE_OUTER_BOUND ( 'NONE', #117900, .T. ) ;
#98294 = VERTEX_POINT ( 'NONE', #24695 ) ;
#98295 = VERTEX_POINT ( 'NONE', #116917 ) ;
#98296 = AXIS2_PLACEMENT_3D ( 'NONE', #28565, #39055, #109709 ) ;
#98297 = DIRECTION ( 'NONE',  ( -0.000000000000000000, -1.000000000000000000, -0.000000000000000000 ) ) ;
#98298 = CONICAL_SURFACE ( 'NONE', #119237, 0.1000000000000002554, 0.003490658503988666988 ) ;
#98299 = ORIENTED_EDGE ( 'NONE', *, *, #6502, .F. ) ;
#98300 = LINE ( 'NONE', #9291, #19481 ) ;
#98301 = CARTESIAN_POINT ( 'NONE',  ( -5.650000000000019895, 2.500000000000000000, 2.511473670974873507 ) ) ;
#98303 = AXIS2_PLACEMENT_3D ( 'NONE', #8827, #48783, #69049 ) ;
#98302 = AXIS2_PLACEMENT_3D ( 'NONE', #15224, #53889, #93817 ) ;
#98304 = ORIENTED_EDGE ( 'NONE', *, *, #108839, .T. ) ;
#98305 = CARTESIAN_POINT ( 'NONE',  ( 185.6666666666666856, -6.668395609140176816, -3.850000000000003642 ) ) ;
#98306 = DIRECTION ( 'NONE',  ( 0.000000000000000000, -0.000000000000000000, 1.000000000000000000 ) ) ;
#98307 = CARTESIAN_POINT ( 'NONE',  ( -4.550000000000022915, 12.50000000000000000, 2.099970236277060032 ) ) ;
#98308 = CARTESIAN_POINT ( 'NONE',  ( 13.09999999999989839, 12.50000000000000000, -0.3464101615137783474 ) ) ;
#98309 = ORIENTED_EDGE ( 'NONE', *, *, #45695, .T. ) ;
#98310 = EDGE_CURVE ( 'NONE', #98275, #57844, #87029, .T. ) ;
#98311 = CARTESIAN_POINT ( 'NONE',  ( 3.749999999999944045, 12.50000000000000000, -7.188010851410854052 ) ) ;
#98312 = EDGE_LOOP ( 'NONE', ( #4820, #15148 ) ) ;
#98313 = EDGE_CURVE ( 'NONE', #62529, #95423, #118423, .T. ) ;
#98314 = CARTESIAN_POINT ( 'NONE',  ( 34.93098733902322550, 2.900247951333832841, -4.640741454330529869 ) ) ;
#98315 = CARTESIAN_POINT ( 'NONE',  ( -2.500000000000032419, 2.500000000000000000, 0.6928203230275494784 ) ) ;
#98316 = ADVANCED_FACE ( 'NONE', ( #66535 ), #104535, .T. ) ;
#98317 = CARTESIAN_POINT ( 'NONE',  ( 2.899999999999945732, 2.500000000000000000, -4.230127018922201998 ) ) ;
#98318 = EDGE_LOOP ( 'NONE', ( #128474, #117712, #18976, #96493 ) ) ;
#98319 = CARTESIAN_POINT ( 'NONE',  ( -3.100000000000028511, 2.500000000000000000, -0.3464101615137782364 ) ) ;
#98320 = EDGE_CURVE ( 'NONE', #67065, #114454, #59972, .T. ) ;
#98321 = EDGE_CURVE ( 'NONE', #36118, #9409, #96007, .T. ) ;
#98322 = EDGE_LOOP ( 'NONE', ( #84814, #52564, #58473, #50559 ) ) ;
#98323 = CARTESIAN_POINT ( 'NONE',  ( 9.149999999999918643, 12.50000000000000000, 2.165063509461097713 ) ) ;
#98324 = LINE ( 'NONE', #118619, #98978 ) ;
#98325 = EDGE_CURVE ( 'NONE', #70057, #41901, #57899, .T. ) ;
#98326 = EDGE_CURVE ( 'NONE', #1374, #4680, #30721, .T. ) ;
#98327 = FACE_OUTER_BOUND ( 'NONE', #45998, .T. ) ;
#98328 = ORIENTED_EDGE ( 'NONE', *, *, #46913, .F. ) ;
#98329 = AXIS2_PLACEMENT_3D ( 'NONE', #127125, #47917, #77371 ) ;
#98330 = FACE_OUTER_BOUND ( 'NONE', #13978, .T. ) ;
#98331 = VECTOR ( 'NONE', #124840, 1000.000000000000000 ) ;
#98332 = EDGE_CURVE ( 'NONE', #78481, #120522, #6308, .T. ) ;
#98333 = CARTESIAN_POINT ( 'NONE',  ( -4.200000000000025935, 2.500000000000000000, -2.385244779468109755E-15 ) ) ;
#98334 = ORIENTED_EDGE ( 'NONE', *, *, #77364, .F. ) ;
#98335 = CARTESIAN_POINT ( 'NONE',  ( -0.8500000000000386136, 2.500000000000000000, 7.288010851410849256 ) ) ;
#98336 = EDGE_LOOP ( 'NONE', ( #53808, #24121, #96979, #13237 ) ) ;
#98337 = EDGE_CURVE ( 'NONE', #45239, #110014, #17739, .T. ) ;
#98338 = DIRECTION ( 'NONE',  ( -0.000000000000000000, 1.000000000000000000, -0.000000000000000000 ) ) ;
#98339 = EDGE_LOOP ( 'NONE', ( #23011, #2795 ) ) ;
#98340 = CARTESIAN_POINT ( 'NONE',  ( 187.5000000000000000, 9.429780353434619030E-16, -7.700000000000000178 ) ) ;
#98341 = DIRECTION ( 'NONE',  ( 0.000000000000000000, 1.000000000000000000, 0.000000000000000000 ) ) ;
#98342 = ORIENTED_EDGE ( 'NONE', *, *, #8458, .F. ) ;
#98343 = VERTEX_POINT ( 'NONE', #25310 ) ;
#98344 = DIRECTION ( 'NONE',  ( 0.000000000000000000, 1.000000000000000000, 0.000000000000000000 ) ) ;
#98345 = FACE_OUTER_BOUND ( 'NONE', #7383, .T. ) ;
#98346 = ORIENTED_EDGE ( 'NONE', *, *, #121851, .F. ) ;
#98348 = CARTESIAN_POINT ( 'NONE',  ( 185.5416666666666856, -4.445597072760063107, 7.700000000000102318 ) ) ;
#98347 = AXIS2_PLACEMENT_3D ( 'NONE', #38780, #110074, #21040 ) ;
#98349 = CARTESIAN_POINT ( 'NONE',  ( 186.4427083336747160, -6.551208109652278289, 3.782341765624995134 ) ) ;
#98350 = AXIS2_PLACEMENT_3D ( 'NONE', #73231, #78714, #118616 ) ;
#98351 = DIRECTION ( 'NONE',  ( 0.000000000000000000, 1.000000000000000000, 0.000000000000000000 ) ) ;
#98352 = DIRECTION ( 'NONE',  ( 0.000000000000000000, 0.000000000000000000, 1.000000000000000000 ) ) ;
#98353 = CARTESIAN_POINT ( 'NONE',  ( -2.100000000000034284, 12.50000000000000000, -4.330127018922201643 ) ) ;
#98354 = DIRECTION ( 'NONE',  ( -0.000000000000000000, -1.000000000000000000, -0.000000000000000000 ) ) ;
#98355 = DIRECTION ( 'NONE',  ( 0.000000000000000000, 0.000000000000000000, 1.000000000000000000 ) ) ;
#98356 = CONICAL_SURFACE ( 'NONE', #56587, 0.1000000000000002554, 0.003490658503988666988 ) ;
#98357 = ORIENTED_EDGE ( 'NONE', *, *, #22308, .T. ) ;
#98358 = EDGE_LOOP ( 'NONE', ( #115098, #126346 ) ) ;
#98359 = VERTEX_POINT ( 'NONE', #126765 ) ;
#98360 = VERTEX_POINT ( 'NONE', #124178 ) ;
#98361 = CIRCLE ( 'NONE', #37749, 0.5000000000000000000 ) ;
#98362 = CARTESIAN_POINT ( 'NONE',  ( 0.1999999999999627909, 12.50000000000000000, 0.3464101615137758494 ) ) ;
#98363 = CARTESIAN_POINT ( 'NONE',  ( 10.84999999999990905, 12.50000000000000000, 2.165063509461097713 ) ) ;
#98364 = DIRECTION ( 'NONE',  ( 0.000000000000000000, 0.000000000000000000, 1.000000000000000000 ) ) ;
#98365 = ORIENTED_EDGE ( 'NONE', *, *, #21835, .F. ) ;
#98366 = FACE_BOUND ( 'NONE', #127118, .T. ) ;
#98367 = ORIENTED_EDGE ( 'NONE', *, *, #4222, .F. ) ;
#98368 = FACE_OUTER_BOUND ( 'NONE', #3654, .T. ) ;
#98369 = DIRECTION ( 'NONE',  ( 0.000000000000000000, 0.000000000000000000, 1.000000000000000000 ) ) ;
#98370 = DIRECTION ( 'NONE',  ( 0.000000000000000000, -0.9999939076577903929, 0.003490651415223739937 ) ) ;
#98371 = EDGE_CURVE ( 'NONE', #75848, #125178, #112273, .T. ) ;
#98372 = CARTESIAN_POINT ( 'NONE',  ( -10.65000000000000213, 2.500000000000000000, 6.841600689897072485 ) ) ;
#98373 = DIRECTION ( 'NONE',  ( -4.274815082592931898E-19, -0.9999939076577903929, -0.003490651415223739937 ) ) ;
#98374 = CARTESIAN_POINT ( 'NONE',  ( 10.84999999999990905, 12.50000000000000000, -5.802370205355749988 ) ) ;
#98375 = CARTESIAN_POINT ( 'NONE',  ( -4.600000000000024514, 12.50000000000000000, -0.6928203230275542523 ) ) ;
#98376 = DIRECTION ( 'NONE',  ( 0.000000000000000000, 1.000000000000000000, 0.000000000000000000 ) ) ;
#98377 = DIRECTION ( 'NONE',  ( -0.000000000000000000, -1.000000000000000000, -0.000000000000000000 ) ) ;
#98378 = DIRECTION ( 'NONE',  ( 0.000000000000000000, 0.000000000000000000, 1.000000000000000000 ) ) ;
#98379 = EDGE_CURVE ( 'NONE', #106850, #35030, #76666, .T. ) ;
#98380 = ORIENTED_EDGE ( 'NONE', *, *, #78900, .T. ) ;
#98381 = ORIENTED_EDGE ( 'NONE', *, *, #76038, .T. ) ;
#98382 = VERTEX_POINT ( 'NONE', #76374 ) ;
#98383 = VERTEX_POINT ( 'NONE', #75706 ) ;
#98384 = DIRECTION ( 'NONE',  ( -0.000000000000000000, -1.000000000000000000, -0.000000000000000000 ) ) ;
#98385 = AXIS2_PLACEMENT_3D ( 'NONE', #19722, #118550, #110663 ) ;
#98386 = CARTESIAN_POINT ( 'NONE',  ( 4.799999999999939426, 2.500000000000000000, -4.576537180435977348 ) ) ;
#98387 = AXIS2_PLACEMENT_3D ( 'NONE', #2820, #63032, #83329 ) ;
#98388 = CIRCLE ( 'NONE', #2239, 0.06509327318403741736 ) ;
#98390 = ORIENTED_EDGE ( 'NONE', *, *, #117956, .F. ) ;
#98389 = ORIENTED_EDGE ( 'NONE', *, *, #124892, .T. ) ;
#98391 = EDGE_LOOP ( 'NONE', ( #51977, #10599, #64401, #99210 ) ) ;
#98392 = DIRECTION ( 'NONE',  ( 0.000000000000000000, 1.000000000000000000, 0.000000000000000000 ) ) ;
#98393 = AXIS2_PLACEMENT_3D ( 'NONE', #110, #61632, #89788 ) ;
#98394 = DIRECTION ( 'NONE',  ( -0.000000000000000000, -1.000000000000000000, -0.000000000000000000 ) ) ;
#98395 = CARTESIAN_POINT ( 'NONE',  ( -1.050000000000038680, 2.500000000000000000, 2.411473670974873862 ) ) ;
#98396 = CARTESIAN_POINT ( 'NONE',  ( -10.20000000000000462, 12.50000000000000000, 0.3464101615137735735 ) ) ;
#98397 = CARTESIAN_POINT ( 'NONE',  ( 11.44999999999990514, 2.500000000000000000, 2.511473670974873507 ) ) ;
#98398 = DIRECTION ( 'NONE',  ( 0.000000000000000000, 0.000000000000000000, 1.000000000000000000 ) ) ;
#98399 = CIRCLE ( 'NONE', #73359, 0.06509327318403745899 ) ;
#98400 = DIRECTION ( 'NONE',  ( 0.000000000000000000, 0.000000000000000000, 1.000000000000000000 ) ) ;
#98401 = EDGE_LOOP ( 'NONE', ( #107478, #3733 ) ) ;
#98402 = CARTESIAN_POINT ( 'NONE',  ( 6.249999999999930722, 12.50000000000000000, 1.472243186433545459 ) ) ;
#98403 = ORIENTED_EDGE ( 'NONE', *, *, #109078, .F. ) ;
#98404 = VERTEX_POINT ( 'NONE', #15498 ) ;
#98405 = VERTEX_POINT ( 'NONE', #34530 ) ;
#98406 = CARTESIAN_POINT ( 'NONE',  ( -0.8500000000000386136, 2.500000000000000000, 7.188010851410848723 ) ) ;
#98407 = EDGE_LOOP ( 'NONE', ( #118743, #16775 ) ) ;
#98408 = ORIENTED_EDGE ( 'NONE', *, *, #87631, .F. ) ;
#98409 = DIRECTION ( 'NONE',  ( 0.000000000000000000, 0.000000000000000000, -1.000000000000000000 ) ) ;
#98410 = EDGE_CURVE ( 'NONE', #115296, #115890, #5671, .T. ) ;
#98411 = DIRECTION ( 'NONE',  ( -0.000000000000000000, 1.000000000000000000, -0.000000000000000000 ) ) ;
#98412 = DIRECTION ( 'NONE',  ( 0.000000000000000000, -0.000000000000000000, 1.000000000000000000 ) ) ;
#98413 = DIRECTION ( 'NONE',  ( 0.000000000000000000, 1.000000000000000000, 0.000000000000000000 ) ) ;
#98414 = DIRECTION ( 'NONE',  ( 0.000000000000000000, 0.000000000000000000, 1.000000000000000000 ) ) ;
#98415 = VERTEX_POINT ( 'NONE', #26622 ) ;
#98416 = FACE_OUTER_BOUND ( 'NONE', #100733, .T. ) ;
#98417 = VECTOR ( 'NONE', #99593, 1000.000000000000000 ) ;
#98418 = EDGE_CURVE ( 'NONE', #93494, #4249, #129014, .T. ) ;
#98419 = CIRCLE ( 'NONE', #58733, 0.1000000000000000472 ) ;
#98420 = VERTEX_POINT ( 'NONE', #16772 ) ;
#98421 = DIRECTION ( 'NONE',  ( 0.000000000000000000, -0.000000000000000000, 1.000000000000000000 ) ) ;
#98422 = VERTEX_POINT ( 'NONE', #56696 ) ;
#98423 = CARTESIAN_POINT ( 'NONE',  ( 108.3381794683780583, 7.119691004531020440, 5.000000000000002665 ) ) ;
#98424 = FACE_OUTER_BOUND ( 'NONE', #46029, .T. ) ;
#98425 = ORIENTED_EDGE ( 'NONE', *, *, #83752, .T. ) ;
#98427 = ADVANCED_FACE ( 'NONE', ( #6947 ), #46920, .T. ) ;
#98426 = CARTESIAN_POINT ( 'NONE',  ( 8.099999999999923261, 2.500000000000000000, -4.676537180435978769 ) ) ;
#98428 = CARTESIAN_POINT ( 'NONE',  ( 1.249999999999954259, 12.50000000000000000, -7.253104124594891289 ) ) ;
#98429 = ADVANCED_FACE ( 'NONE', ( #9564 ), #93390, .T. ) ;
#98430 = ORIENTED_EDGE ( 'NONE', *, *, #51288, .T. ) ;
#98431 = AXIS2_PLACEMENT_3D ( 'NONE', #91194, #101668, #882 ) ;
#98432 = AXIS2_PLACEMENT_3D ( 'NONE', #40674, #65, #110665 ) ;
#98433 = EDGE_CURVE ( 'NONE', #92053, #76876, #7688, .T. ) ;
#98434 = DIRECTION ( 'NONE',  ( 0.000000000000000000, 1.000000000000000000, 0.000000000000000000 ) ) ;
#98435 = ORIENTED_EDGE ( 'NONE', *, *, #127581, .T. ) ;
#98436 = ORIENTED_EDGE ( 'NONE', *, *, #11897, .F. ) ;
#98437 = CARTESIAN_POINT ( 'NONE',  ( -0.4000000000000401013, 2.500000000000000000, -3.637306695894650055 ) ) ;
#98438 = DIRECTION ( 'NONE',  ( 0.000000000000000000, 1.000000000000000000, 0.000000000000000000 ) ) ;
#98439 = EDGE_CURVE ( 'NONE', #110749, #74045, #74607, .T. ) ;
#98440 = CARTESIAN_POINT ( 'NONE',  ( 185.7552083336747444, 6.551208109652275624, -3.782341765624998686 ) ) ;
#98441 = CARTESIAN_POINT ( 'NONE',  ( 0.1999999999999562961, 2.500000000000000000, 4.576537180435972019 ) ) ;
#98442 = AXIS2_PLACEMENT_3D ( 'NONE', #122328, #92195, #103322 ) ;
#98443 = VECTOR ( 'NONE', #17513, 1000.000000000000000 ) ;
#98444 = DIRECTION ( 'NONE',  ( -1.000000000000000000, 0.000000000000000000, 0.000000000000000000 ) ) ;
#98445 = ORIENTED_EDGE ( 'NONE', *, *, #62514, .T. ) ;
#98446 = CARTESIAN_POINT ( 'NONE',  ( -10.20000000000000284, 2.500000000000000000, 3.983716857408420964 ) ) ;
#98447 = AXIS2_PLACEMENT_3D ( 'NONE', #118306, #127494, #59416 ) ;
#98448 = ORIENTED_EDGE ( 'NONE', *, *, #29085, .T. ) ;
#98449 = DIRECTION ( 'NONE',  ( 0.000000000000000000, 1.000000000000000000, 0.000000000000000000 ) ) ;
#98450 = DIRECTION ( 'NONE',  ( -0.000000000000000000, -1.000000000000000000, -0.000000000000000000 ) ) ;
#98451 = VERTEX_POINT ( 'NONE', #109704 ) ;
#98452 = CIRCLE ( 'NONE', #39998, 0.06509327318403745899 ) ;
#98453 = CARTESIAN_POINT ( 'NONE',  ( -11.24999999999996447, 2.500000000000000000, -2.265063509461097802 ) ) ;
#98454 = DIRECTION ( 'NONE',  ( -4.274815082592931898E-19, -0.9999939076577903929, -0.003490651415223739937 ) ) ;
#98455 = DIRECTION ( 'NONE',  ( -0.000000000000000000, -1.000000000000000000, -0.000000000000000000 ) ) ;
#98456 = CARTESIAN_POINT ( 'NONE',  ( 194.5000000000000000, 0.000000000000000000, 0.000000000000000000 ) ) ;
#98457 = CARTESIAN_POINT ( 'NONE',  ( 0.1999999999999567124, 12.50000000000000000, -3.918623584224389056 ) ) ;
#98458 = ORIENTED_EDGE ( 'NONE', *, *, #22168, .F. ) ;
#98459 = CARTESIAN_POINT ( 'NONE',  ( 2.899999999999945732, 2.500000000000000000, -2.385244779468109755E-15 ) ) ;
#98460 = DIRECTION ( 'NONE',  ( 0.000000000000000000, 0.000000000000000000, -1.000000000000000000 ) ) ;
#98461 = ORIENTED_EDGE ( 'NONE', *, *, #72394, .T. ) ;
#98462 = ADVANCED_FACE ( 'NONE', ( #107758 ), #78320, .T. ) ;
#98463 = CARTESIAN_POINT ( 'NONE',  ( -4.350000000000023626, 2.500000000000000000, 6.148780366869520897 ) ) ;
#98464 = ORIENTED_EDGE ( 'NONE', *, *, #17150, .F. ) ;
#98465 = EDGE_LOOP ( 'NONE', ( #29425, #54374, #98389, #13997 ) ) ;
#98466 = DIRECTION ( 'NONE',  ( -0.000000000000000000, -1.000000000000000000, -0.000000000000000000 ) ) ;
#98468 = EDGE_CURVE ( 'NONE', #80552, #93103, #99649, .T. ) ;
#98467 = CONICAL_SURFACE ( 'NONE', #73441, 0.1000000000000002554, 0.003490658503988666988 ) ;
#98469 = AXIS2_PLACEMENT_3D ( 'NONE', #11184, #10535, #90379 ) ;
#98470 = EDGE_CURVE ( 'NONE', #67325, #124086, #99242, .T. ) ;
#98471 = CONICAL_SURFACE ( 'NONE', #115185, 0.1000000000000002554, 0.003490658503988666988 ) ;
#98472 = EDGE_LOOP ( 'NONE', ( #128418, #40909 ) ) ;
#98473 = DIRECTION ( 'NONE',  ( 0.000000000000000000, 1.000000000000000000, 0.000000000000000000 ) ) ;
#98475 = EDGE_CURVE ( 'NONE', #23121, #103499, #89277, .T. ) ;
#98474 = CARTESIAN_POINT ( 'NONE',  ( 1.849999999999951017, 2.500000000000000000, -6.148780366869526226 ) ) ;
#98476 = EDGE_CURVE ( 'NONE', #32813, #76857, #39131, .T. ) ;
#98477 = VERTEX_POINT ( 'NONE', #19360 ) ;
#98479 = DIRECTION ( 'NONE',  ( -0.000000000000000000, 1.000000000000000000, -0.000000000000000000 ) ) ;
#98478 = CIRCLE ( 'NONE', #115188, 0.06509327318403745899 ) ;
#98480 = EDGE_CURVE ( 'NONE', #35232, #13086, #49496, .T. ) ;
#98482 = ORIENTED_EDGE ( 'NONE', *, *, #39373, .F. ) ;
#98481 = CARTESIAN_POINT ( 'NONE',  ( -9.150000000000009237, 12.50000000000000000, 1.472243186433545459 ) ) ;
#98483 = VECTOR ( 'NONE', #68308, 1000.000000000000000 ) ;
#98484 = DIRECTION ( 'NONE',  ( 0.000000000000000000, 0.000000000000000000, 1.000000000000000000 ) ) ;
#98485 = CARTESIAN_POINT ( 'NONE',  ( 7.899999999999924860, 12.50000000000000000, 4.265033745738159077 ) ) ;
#98486 = ORIENTED_EDGE ( 'NONE', *, *, #32015, .T. ) ;
#98487 = EDGE_CURVE ( 'NONE', #88341, #19578, #20677, .T. ) ;
#98488 = EDGE_CURVE ( 'NONE', #76546, #102801, #48855, .T. ) ;
#98489 = VERTEX_POINT ( 'NONE', #118868 ) ;
#98490 = ORIENTED_EDGE ( 'NONE', *, *, #28422, .F. ) ;
#98491 = DIRECTION ( 'NONE',  ( 0.000000000000000000, -0.000000000000000000, 1.000000000000000000 ) ) ;
#98492 = CARTESIAN_POINT ( 'NONE',  ( 13.09999999999990195, 2.500000000000000000, 3.983716857408420076 ) ) ;
#98493 = DIRECTION ( 'NONE',  ( -0.000000000000000000, 1.000000000000000000, -0.000000000000000000 ) ) ;
#98494 = FACE_BOUND ( 'NONE', #10263, .T. ) ;
#98495 = EDGE_LOOP ( 'NONE', ( #17531, #8912, #54067, #107761 ) ) ;
#98496 = FACE_OUTER_BOUND ( 'NONE', #96354, .T. ) ;
#98497 = LINE ( 'NONE', #10141, #119242 ) ;
#98498 = ORIENTED_EDGE ( 'NONE', *, *, #102441, .F. ) ;
#98499 = DIRECTION ( 'NONE',  ( 0.8660254037844390407, 0.000000000000000000, -0.4999999999999991673 ) ) ;
#98500 = CARTESIAN_POINT ( 'NONE',  ( 5.849999999999933920, 12.50000000000000000, 6.560283801567334372 ) ) ;
#98501 = DIRECTION ( 'NONE',  ( 0.000000000000000000, 1.000000000000000000, 0.000000000000000000 ) ) ;
#98502 = CARTESIAN_POINT ( 'NONE',  ( -13.14999999999999147, 2.500000000000000000, 2.611473670974877148 ) ) ;
#98503 = CARTESIAN_POINT ( 'NONE',  ( -12.29999999999999538, 2.500000000000000000, 4.676537180435972552 ) ) ;
#98504 = CARTESIAN_POINT ( 'NONE',  ( 12.04999999999990834, 12.50000000000000000, 6.430097255199259010 ) ) ;
#98505 = CARTESIAN_POINT ( 'NONE',  ( -9.550000000000007816, 2.500000000000000000, -6.495190528383297135 ) ) ;
#98506 = VECTOR ( 'NONE', #102785, 1000.000000000000000 ) ;
#98507 = ORIENTED_EDGE ( 'NONE', *, *, #57298, .T. ) ;
#98508 = VERTEX_POINT ( 'NONE', #58668 ) ;
#98509 = ORIENTED_EDGE ( 'NONE', *, *, #104536, .T. ) ;
#98510 = EDGE_LOOP ( 'NONE', ( #10538, #20903, #81722, #97449, #12682 ) ) ;
#98511 = EDGE_LOOP ( 'NONE', ( #32496, #93974, #117631, #46767 ) ) ;
#98512 = DIRECTION ( 'NONE',  ( 0.000000000000000000, 1.000000000000000000, 0.000000000000000000 ) ) ;
#98513 = FACE_OUTER_BOUND ( 'NONE', #1186, .T. ) ;
#98514 = EDGE_LOOP ( 'NONE', ( #44890, #128454 ) ) ;
#98515 = FACE_BOUND ( 'NONE', #90376, .T. ) ;
#98516 = AXIS2_PLACEMENT_3D ( 'NONE', #8480, #48421, #88322 ) ;
#98517 = FACE_OUTER_BOUND ( 'NONE', #57379, .T. ) ;
#98518 = CIRCLE ( 'NONE', #108984, 0.09999999999999982514 ) ;
#98519 = DIRECTION ( 'NONE',  ( 0.000000000000000000, -0.9999939076577903929, 0.003490651415223739937 ) ) ;
#98520 = DIRECTION ( 'NONE',  ( 0.000000000000000000, 1.000000000000000000, 0.000000000000000000 ) ) ;
#98521 = CARTESIAN_POINT ( 'NONE',  ( 8.349999999999919709, 2.500000000000000000, 6.495190528383297135 ) ) ;
#98522 = FACE_OUTER_BOUND ( 'NONE', #100512, .T. ) ;
#98523 = ORIENTED_EDGE ( 'NONE', *, *, #33005, .F. ) ;
#98524 = AXIS2_PLACEMENT_3D ( 'NONE', #80951, #120228, #22040 ) ;
#98525 = ORIENTED_EDGE ( 'NONE', *, *, #126524, .T. ) ;
#98526 = EDGE_CURVE ( 'NONE', #34747, #50067, #79592, .T. ) ;
#98527 = ORIENTED_EDGE ( 'NONE', *, *, #90607, .T. ) ;
#98528 = VERTEX_POINT ( 'NONE', #8897 ) ;
#98529 = VECTOR ( 'NONE', #60024, 1000.000000000000000 ) ;
#98530 = DIRECTION ( 'NONE',  ( 0.000000000000000000, -0.000000000000000000, 1.000000000000000000 ) ) ;
#98531 = CARTESIAN_POINT ( 'NONE',  ( 8.340322510150830482, 2.500000000000000000, 8.517653998215561018 ) ) ;
#98532 = DIRECTION ( 'NONE',  ( 0.000000000000000000, 0.000000000000000000, 1.000000000000000000 ) ) ;
#98533 = EDGE_LOOP ( 'NONE', ( #11361, #75752, #70086, #115181 ) ) ;
#98534 = DIRECTION ( 'NONE',  ( 0.000000000000000000, 1.000000000000000000, 0.000000000000000000 ) ) ;
#98535 = CIRCLE ( 'NONE', #123584, 0.1000000000000002554 ) ;
#98536 = PLANE ( 'NONE',  #105490 ) ;
#98537 = DIRECTION ( 'NONE',  ( -0.000000000000000000, -1.000000000000000000, -0.000000000000000000 ) ) ;
#98538 = AXIS2_PLACEMENT_3D ( 'NONE', #19821, #27679, #68256 ) ;
#98539 = AXIS2_PLACEMENT_3D ( 'NONE', #126775, #36478, #128061 ) ;
#98540 = CARTESIAN_POINT ( 'NONE',  ( 186.0260416670080588, -6.551208109652273848, -3.782341765625003571 ) ) ;
#98541 = DIRECTION ( 'NONE',  ( 0.000000000000000000, 0.000000000000000000, -1.000000000000000000 ) ) ;
#98542 = CARTESIAN_POINT ( 'NONE',  ( 13.29999999999990301, 12.50000000000000000, 4.265033745738159077 ) ) ;
#98543 = DIRECTION ( 'NONE',  ( 0.000000000000000000, 1.000000000000000000, 0.000000000000000000 ) ) ;
#98544 = ORIENTED_EDGE ( 'NONE', *, *, #14729, .T. ) ;
#98545 = DIRECTION ( 'NONE',  ( -4.274815082592931898E-19, -0.9999939076577903929, -0.003490651415223739937 ) ) ;
#98546 = VERTEX_POINT ( 'NONE', #8257 ) ;
#98547 = ORIENTED_EDGE ( 'NONE', *, *, #105933, .T. ) ;
#98548 = CARTESIAN_POINT ( 'NONE',  ( 5.399999999999935518, 12.50000000000000000, -4.330127018922201643 ) ) ;
#98549 = LINE ( 'NONE', #88758, #69867 ) ;
#98550 = CARTESIAN_POINT ( 'NONE',  ( -2.100000000000033396, 2.500000000000000000, -0.7928203230275543412 ) ) ;
#98551 = EDGE_CURVE ( 'NONE', #82416, #64406, #48194, .T. ) ;
#98552 = ORIENTED_EDGE ( 'NONE', *, *, #126260, .T. ) ;
#98553 = EDGE_LOOP ( 'NONE', ( #68235, #67510, #23648, #84562 ) ) ;
#98554 = DIRECTION ( 'NONE',  ( -0.000000000000000000, -1.000000000000000000, -0.000000000000000000 ) ) ;
#98555 = CARTESIAN_POINT ( 'NONE',  ( 139.9358549477330200, 2.500000000000000000, -3.576063159858998475 ) ) ;
#98557 = DIRECTION ( 'NONE',  ( -0.000000000000000000, 1.000000000000000000, -0.000000000000000000 ) ) ;
#98556 = CIRCLE ( 'NONE', #61012, 0.06509327318403745899 ) ;
#98558 = ORIENTED_EDGE ( 'NONE', *, *, #31260, .F. ) ;
#98559 = ORIENTED_EDGE ( 'NONE', *, *, #63505, .T. ) ;
#98560 = AXIS2_PLACEMENT_3D ( 'NONE', #880, #10058, #12616 ) ;
#98561 = DIRECTION ( 'NONE',  ( 0.000000000000000000, 0.000000000000000000, 1.000000000000000000 ) ) ;
#98562 = EDGE_CURVE ( 'NONE', #29366, #48393, #3507, .T. ) ;
#98563 = VERTEX_POINT ( 'NONE', #20033 ) ;
#98564 = DIRECTION ( 'NONE',  ( -0.000000000000000000, -1.000000000000000000, -0.000000000000000000 ) ) ;
#98565 = EDGE_CURVE ( 'NONE', #92934, #128018, #72565, .T. ) ;
#98566 = CIRCLE ( 'NONE', #27559, 0.06509327318403745899 ) ;
#98567 = EDGE_LOOP ( 'NONE', ( #13681, #114723, #121173, #19670 ) ) ;
#98568 = DIRECTION ( 'NONE',  ( -4.274815082592931898E-19, -0.9999939076577903929, -0.003490651415223739937 ) ) ;
#98569 = CIRCLE ( 'NONE', #44203, 0.06509327318403745899 ) ;
#98570 = DIRECTION ( 'NONE',  ( 0.000000000000000000, 0.000000000000000000, 1.000000000000000000 ) ) ;
#98571 = CARTESIAN_POINT ( 'NONE',  ( -2.900000000000029221, 12.50000000000000000, -4.330127018922201643 ) ) ;
#98572 = VECTOR ( 'NONE', #44292, 1000.000000000000000 ) ;
#98573 = ADVANCED_FACE ( 'NONE', ( #50145 ), #16088, .T. ) ;
#98574 = DIRECTION ( 'NONE',  ( 0.000000000000000000, 0.000000000000000000, 1.000000000000000000 ) ) ;
#98575 = EDGE_CURVE ( 'NONE', #118566, #83964, #70405, .T. ) ;
#98576 = VERTEX_POINT ( 'NONE', #71060 ) ;
#98577 = AXIS2_PLACEMENT_3D ( 'NONE', #108347, #79546, #116868 ) ;
#98578 = DIRECTION ( 'NONE',  ( 0.000000000000000000, 1.000000000000000000, 0.000000000000000000 ) ) ;
#98579 = EDGE_CURVE ( 'NONE', #100174, #15903, #97584, .T. ) ;
#98580 = VERTEX_POINT ( 'NONE', #63823 ) ;
#98581 = ADVANCED_FACE ( 'NONE', ( #33092 ), #122099, .T. ) ;
#98582 = ORIENTED_EDGE ( 'NONE', *, *, #237, .T. ) ;
#98583 = EDGE_CURVE ( 'NONE', #115200, #76721, #62102, .T. ) ;
#98584 = LINE ( 'NONE', #60000, #85214 ) ;
#98585 = FACE_OUTER_BOUND ( 'NONE', #30258, .T. ) ;
#98586 = CARTESIAN_POINT ( 'NONE',  ( 17.50000000000000000, 2.500000000000000000, 2.922290670087886344 ) ) ;
#98587 = ADVANCED_FACE ( 'NONE', ( #52700 ), #103857, .T. ) ;
#98588 = DIRECTION ( 'NONE',  ( 0.000000000000000000, 0.000000000000000000, 1.000000000000000000 ) ) ;
#98589 = LINE ( 'NONE', #90065, #113897 ) ;
#98590 = DIRECTION ( 'NONE',  ( 0.000000000000000000, 0.000000000000000000, 1.000000000000000000 ) ) ;
#98591 = CARTESIAN_POINT ( 'NONE',  ( -13.94999999999998863, 2.500000000000000000, -1.818653347947323917 ) ) ;
#98592 = DIRECTION ( 'NONE',  ( 0.000000000000000000, 0.000000000000000000, 1.000000000000000000 ) ) ;
#98593 = CARTESIAN_POINT ( 'NONE',  ( 6.849999999999929479, 2.500000000000000000, -2.411473670974877859 ) ) ;
#98594 = EDGE_CURVE ( 'NONE', #125908, #109519, #13955, .T. ) ;
#98595 = DIRECTION ( 'NONE',  ( 0.000000000000000000, -0.000000000000000000, 1.000000000000000000 ) ) ;
#98596 = CONICAL_SURFACE ( 'NONE', #106923, 0.1000000000000002554, 0.003490658503988666988 ) ;
#98597 = AXIS2_PLACEMENT_3D ( 'NONE', #104241, #76714, #84606 ) ;
#98598 = VERTEX_POINT ( 'NONE', #31154 ) ;
#98599 = DIRECTION ( 'NONE',  ( 0.000000000000000000, 1.000000000000000000, 0.000000000000000000 ) ) ;
#98600 = CARTESIAN_POINT ( 'NONE',  ( 14.34999999999989662, 2.500000000000000000, 1.818653347947321475 ) ) ;
#98601 = CARTESIAN_POINT ( 'NONE',  ( 0.8499999999999536815, 12.50000000000000000, 5.802370205355744659 ) ) ;
#98602 = DIRECTION ( 'NONE',  ( 0.000000000000000000, 1.000000000000000000, 0.000000000000000000 ) ) ;
#98603 = CARTESIAN_POINT ( 'NONE',  ( 1.449999999999950440, 12.50000000000000000, 6.213873640053558134 ) ) ;
#98604 = CONICAL_SURFACE ( 'NONE', #90290, 0.1000000000000000472, 0.003490658503988666988 ) ;
#98605 = AXIS2_PLACEMENT_3D ( 'NONE', #33706, #44167, #85384 ) ;
#98606 = VERTEX_POINT ( 'NONE', #53360 ) ;
#98607 = CARTESIAN_POINT ( 'NONE',  ( -12.09999999999999432, 2.500000000000000000, 5.122947341949749323 ) ) ;
#98608 = AXIS2_PLACEMENT_3D ( 'NONE', #67238, #126852, #35256 ) ;
#98609 = CIRCLE ( 'NONE', #52659, 0.1000000000000000472 ) ;
#98610 = DIRECTION ( 'NONE',  ( 0.000000000000000000, 1.000000000000000000, 0.000000000000000000 ) ) ;
#98612 = ORIENTED_EDGE ( 'NONE', *, *, #120509, .F. ) ;
#98611 = FACE_OUTER_BOUND ( 'NONE', #65865, .T. ) ;
#98613 = EDGE_CURVE ( 'NONE', #38111, #21644, #120572, .T. ) ;
#98614 = AXIS2_PLACEMENT_3D ( 'NONE', #98474, #107003, #57936 ) ;
#98615 = ORIENTED_EDGE ( 'NONE', *, *, #70273, .T. ) ;
#98617 = AXIS2_PLACEMENT_3D ( 'NONE', #106867, #38826, #78071 ) ;
#98616 = CARTESIAN_POINT ( 'NONE',  ( -6.650000000000019007, 12.50000000000000000, -5.802370205355749988 ) ) ;
#98618 = ORIENTED_EDGE ( 'NONE', *, *, #42360, .T. ) ;
#98619 = ORIENTED_EDGE ( 'NONE', *, *, #26506, .F. ) ;
#98620 = AXIS2_PLACEMENT_3D ( 'NONE', #5454, #6723, #95784 ) ;
#98621 = EDGE_LOOP ( 'NONE', ( #63809, #27151, #81707, #37541 ) ) ;
#98622 = AXIS2_PLACEMENT_3D ( 'NONE', #24021, #103869, #54119 ) ;
#98623 = DIRECTION ( 'NONE',  ( 0.000000000000000000, 0.000000000000000000, -1.000000000000000000 ) ) ;
#98624 = EDGE_CURVE ( 'NONE', #30477, #106999, #24432, .T. ) ;
#98625 = AXIS2_PLACEMENT_3D ( 'NONE', #26554, #66466, #56629 ) ;
#98626 = CARTESIAN_POINT ( 'NONE',  ( -5.000000000000022204, 2.500000000000000000, -0.5928203230275541635 ) ) ;
#98628 = ADVANCED_FACE ( 'NONE', ( #113557 ), #33708, .T. ) ;
#98627 = DIRECTION ( 'NONE',  ( 0.000000000000000000, -0.9999939076577903929, 0.003490651415223739937 ) ) ;
#98629 = CARTESIAN_POINT ( 'NONE',  ( 9.999999999999911182, 2.500000000000000000, 5.022947341949748790 ) ) ;
#98630 = ORIENTED_EDGE ( 'NONE', *, *, #121060, .T. ) ;
#98631 = EDGE_CURVE ( 'NONE', #77225, #27, #93277, .T. ) ;
#98632 = CIRCLE ( 'NONE', #121631, 0.06509327318403745899 ) ;
#98633 = DIRECTION ( 'NONE',  ( 0.000000000000000000, 0.000000000000000000, 1.000000000000000000 ) ) ;
#98634 = ORIENTED_EDGE ( 'NONE', *, *, #91687, .F. ) ;
#98635 = DIRECTION ( 'NONE',  ( -0.000000000000000000, 1.000000000000000000, -0.000000000000000000 ) ) ;
#98636 = CARTESIAN_POINT ( 'NONE',  ( 18.20334136263913294, -2.532871263996626432, -4.817802756305527900 ) ) ;
#98637 = CARTESIAN_POINT ( 'NONE',  ( 18.09676523922516367, 2.526776815559057532, 2.684906793684505022 ) ) ;
#98638 = DIRECTION ( 'NONE',  ( -0.000000000000000000, 1.000000000000000000, -0.000000000000000000 ) ) ;
#98639 = ADVANCED_FACE ( 'NONE', ( #103092 ), #32456, .T. ) ;
#98640 = DIRECTION ( 'NONE',  ( 0.000000000000000000, 0.000000000000000000, 1.000000000000000000 ) ) ;
#98641 = EDGE_CURVE ( 'NONE', #125586, #45052, #11493, .T. ) ;
#98642 = EDGE_LOOP ( 'NONE', ( #28357, #129222 ) ) ;
#98643 = EDGE_CURVE ( 'NONE', #10889, #126164, #108139, .T. ) ;
#98644 = EDGE_CURVE ( 'NONE', #8444, #79920, #129105, .T. ) ;
#98645 = ORIENTED_EDGE ( 'NONE', *, *, #125952, .F. ) ;
#98646 = ORIENTED_EDGE ( 'NONE', *, *, #40992, .T. ) ;
#98647 = ORIENTED_EDGE ( 'NONE', *, *, #72240, .F. ) ;
#98648 = ORIENTED_EDGE ( 'NONE', *, *, #19400, .F. ) ;
#98649 = DIRECTION ( 'NONE',  ( 0.000000000000000000, 1.000000000000000000, 0.000000000000000000 ) ) ;
#98650 = CARTESIAN_POINT ( 'NONE',  ( 1.249999999999953815, 2.500000000000000000, -2.857883832488653741 ) ) ;
#98651 = CARTESIAN_POINT ( 'NONE',  ( -13.54999999999998828, 2.500000000000000000, -2.511473670974875727 ) ) ;
#98652 = FACE_BOUND ( 'NONE', #109833, .T. ) ;
#98653 = CARTESIAN_POINT ( 'NONE',  ( -11.89999999999999680, 12.50000000000000000, -4.741630453620013341 ) ) ;
#98654 = DIRECTION ( 'NONE',  ( 0.000000000000000000, 0.000000000000000000, -1.000000000000000000 ) ) ;
#98655 = EDGE_CURVE ( 'NONE', #11709, #58497, #42917, .T. ) ;
#98656 = DIRECTION ( 'NONE',  ( 0.000000000000000000, 1.000000000000000000, 0.000000000000000000 ) ) ;
#98657 = DIRECTION ( 'NONE',  ( 0.000000000000000000, 1.000000000000000000, 0.000000000000000000 ) ) ;
#98658 = AXIS2_PLACEMENT_3D ( 'NONE', #31875, #39145, #8993 ) ;
#98659 = VECTOR ( 'NONE', #78620, 1000.000000000000000 ) ;
#98661 = AXIS2_PLACEMENT_3D ( 'NONE', #110039, #61596, #10527 ) ;
#98660 = CARTESIAN_POINT ( 'NONE',  ( 186.4218750003414016, 0.000000000000000000, 7.564683531250000925 ) ) ;
#98662 = CARTESIAN_POINT ( 'NONE',  ( -1.450000000000035039, 12.50000000000000000, -2.446380397790840266 ) ) ;
#98663 = LINE ( 'NONE', #79057, #70029 ) ;
#98664 = AXIS2_PLACEMENT_3D ( 'NONE', #103663, #2881, #32997 ) ;
#98666 = DIRECTION ( 'NONE',  ( -0.000000000000000000, 1.000000000000000000, -0.000000000000000000 ) ) ;
#98665 = CIRCLE ( 'NONE', #40202, 0.06509327318403745899 ) ;
#98667 = AXIS2_PLACEMENT_3D ( 'NONE', #91972, #121421, #50134 ) ;
#98668 = VERTEX_POINT ( 'NONE', #92630 ) ;
#98669 = ORIENTED_EDGE ( 'NONE', *, *, #81028, .T. ) ;
#98670 = ORIENTED_EDGE ( 'NONE', *, *, #113076, .T. ) ;
#98671 = ORIENTED_EDGE ( 'NONE', *, *, #3738, .F. ) ;
#98672 = CIRCLE ( 'NONE', #52716, 0.09999999999999982514 ) ;
#98673 = LINE ( 'NONE', #78432, #117023 ) ;
#98674 = CIRCLE ( 'NONE', #77739, 0.06509327318403745899 ) ;
#98675 = DIRECTION ( 'NONE',  ( -0.000000000000000000, 1.000000000000000000, -0.000000000000000000 ) ) ;
#98676 = FACE_BOUND ( 'NONE', #82194, .T. ) ;
#98677 = CARTESIAN_POINT ( 'NONE',  ( 11.24999999999994316, 2.500000000000000000, 2.165063509461097713 ) ) ;
#98678 = ORIENTED_EDGE ( 'NONE', *, *, #17928, .T. ) ;
#98679 = CARTESIAN_POINT ( 'NONE',  ( 4.399999999999940847, 2.500000000000000000, -4.676537180435977881 ) ) ;
#98680 = DIRECTION ( 'NONE',  ( -0.000000000000000000, 1.000000000000000000, -0.000000000000000000 ) ) ;
#98681 = DIRECTION ( 'NONE',  ( 0.000000000000000000, 0.000000000000000000, 1.000000000000000000 ) ) ;
#98682 = DIRECTION ( 'NONE',  ( -0.000000000000000000, 1.000000000000000000, -0.000000000000000000 ) ) ;
#98683 = VERTEX_POINT ( 'NONE', #72360 ) ;
#98684 = DIRECTION ( 'NONE',  ( 1.000000000000000000, -0.000000000000000000, -0.000000000000000000 ) ) ;
#98685 = ADVANCED_FACE ( 'NONE', ( #2297 ), #30802, .T. ) ;
#98686 = ORIENTED_EDGE ( 'NONE', *, *, #27946, .F. ) ;
#98687 = EDGE_LOOP ( 'NONE', ( #104457, #84426 ) ) ;
#98688 = CARTESIAN_POINT ( 'NONE',  ( -8.749999999999976907, 12.50000000000000000, -6.495190528383297135 ) ) ;
#98689 = CARTESIAN_POINT ( 'NONE',  ( -3.350000000000028511, 12.50000000000000000, -1.472243186433550122 ) ) ;
#98690 = EDGE_LOOP ( 'NONE', ( #824, #22762 ) ) ;
#98691 = AXIS2_PLACEMENT_3D ( 'NONE', #80288, #91381, #48903 ) ;
#98692 = CARTESIAN_POINT ( 'NONE',  ( 3.749999999999942268, 2.500000000000000000, -5.702370205355749455 ) ) ;
#98693 = CARTESIAN_POINT ( 'NONE',  ( -2.100000000000033840, 2.500000000000000000, 5.022947341949748790 ) ) ;
#98694 = ORIENTED_EDGE ( 'NONE', *, *, #79850, .F. ) ;
#98695 = DIRECTION ( 'NONE',  ( 0.000000000000000000, 1.000000000000000000, 0.000000000000000000 ) ) ;
#98696 = ORIENTED_EDGE ( 'NONE', *, *, #33768, .F. ) ;
#98697 = ADVANCED_FACE ( 'NONE', ( #122735 ), #101887, .T. ) ;
#98698 = DIRECTION ( 'NONE',  ( -0.000000000000000000, -1.000000000000000000, -0.000000000000000000 ) ) ;
#98699 = CONICAL_SURFACE ( 'NONE', #94504, 0.1000000000000002554, 0.003490658503988666988 ) ;
#98700 = ORIENTED_EDGE ( 'NONE', *, *, #100692, .F. ) ;
#98701 = CARTESIAN_POINT ( 'NONE',  ( 1.449999999999952216, 12.50000000000000000, -2.446380397790840266 ) ) ;
#98702 = AXIS2_PLACEMENT_3D ( 'NONE', #126611, #7455, #88610 ) ;
#98703 = FACE_BOUND ( 'NONE', #59777, .T. ) ;
#98704 = AXIS2_PLACEMENT_3D ( 'NONE', #42113, #92489, #33589 ) ;
#98705 = VERTEX_POINT ( 'NONE', #36307 ) ;
#98706 = CIRCLE ( 'NONE', #84044, 0.06509327318403743123 ) ;
#98707 = CARTESIAN_POINT ( 'NONE',  ( 112.9640574409401808, 7.676535526101522677, -0.6848668807478225373 ) ) ;
#98708 = EDGE_LOOP ( 'NONE', ( #52486, #106932 ) ) ;
#98709 = CARTESIAN_POINT ( 'NONE',  ( -3.350000000000028511, 2.500000000000000000, -2.957883832488653830 ) ) ;
#98710 = FACE_OUTER_BOUND ( 'NONE', #114041, .T. ) ;
#98711 = DIRECTION ( 'NONE',  ( -0.000000000000000000, -1.000000000000000000, -0.000000000000000000 ) ) ;
#98712 = CARTESIAN_POINT ( 'NONE',  ( -7.499999999999980460, 2.500000000000000000, -4.330127018922201643 ) ) ;
#98713 = DIRECTION ( 'NONE',  ( 0.000000000000000000, -0.000000000000000000, 1.000000000000000000 ) ) ;
#98714 = VECTOR ( 'NONE', #97206, 1000.000000000000000 ) ;
#98715 = ORIENTED_EDGE ( 'NONE', *, *, #4292, .T. ) ;
#98716 = ORIENTED_EDGE ( 'NONE', *, *, #104221, .T. ) ;
#98717 = CIRCLE ( 'NONE', #40164, 0.06509327318403745899 ) ;
#98718 = ORIENTED_EDGE ( 'NONE', *, *, #111179, .F. ) ;
#98719 = DIRECTION ( 'NONE',  ( 0.000000000000000000, 0.000000000000000000, 1.000000000000000000 ) ) ;
#98721 = AXIS2_PLACEMENT_3D ( 'NONE', #95537, #66060, #25483 ) ;
#98720 = CARTESIAN_POINT ( 'NONE',  ( 2.099999999999948574, 2.500000000000000000, 4.330127018922196314 ) ) ;
#98722 = CIRCLE ( 'NONE', #90403, 0.09999999999999982514 ) ;
#98723 = CIRCLE ( 'NONE', #25557, 0.1000000000000002554 ) ;
#98724 = CARTESIAN_POINT ( 'NONE',  ( 12.89999999999990266, 2.500000000000000000, -3.737306695894649700 ) ) ;
#98726 = VERTEX_POINT ( 'NONE', #15335 ) ;
#98725 = VERTEX_POINT ( 'NONE', #34373 ) ;
#98727 = EDGE_LOOP ( 'NONE', ( #11722, #112279, #82884, #12432 ) ) ;
#98728 = CARTESIAN_POINT ( 'NONE',  ( 1.649999999999951061, 12.50000000000000000, -6.495190528383302464 ) ) ;
#98729 = AXIS2_PLACEMENT_3D ( 'NONE', #56963, #6549, #66788 ) ;
#98730 = FACE_OUTER_BOUND ( 'NONE', #45917, .T. ) ;
#98731 = EDGE_CURVE ( 'NONE', #4941, #32170, #125940, .T. ) ;
#98732 = APPLICATION_PROTOCOL_DEFINITION ( 'draft international standard', 'automotive_design', 1998, #37995 ) ;
#98733 = DIRECTION ( 'NONE',  ( 0.000000000000000000, 0.000000000000000000, 1.000000000000000000 ) ) ;
#98734 = DIRECTION ( 'NONE',  ( -0.000000000000000000, 1.000000000000000000, -0.000000000000000000 ) ) ;
#98735 = DIRECTION ( 'NONE',  ( -0.000000000000000000, -1.000000000000000000, -0.000000000000000000 ) ) ;
#98736 = DIRECTION ( 'NONE',  ( 0.000000000000000000, 0.000000000000000000, 1.000000000000000000 ) ) ;
#98737 = DIRECTION ( 'NONE',  ( -4.274815082592931898E-19, -0.9999939076577903929, -0.003490651415223739937 ) ) ;
#98738 = DIRECTION ( 'NONE',  ( 0.000000000000000000, 0.000000000000000000, -1.000000000000000000 ) ) ;
#98739 = EDGE_CURVE ( 'NONE', #59330, #103763, #54623, .T. ) ;
#98740 = VERTEX_POINT ( 'NONE', #105009 ) ;
#98741 = ORIENTED_EDGE ( 'NONE', *, *, #6656, .F. ) ;
#98742 = FACE_OUTER_BOUND ( 'NONE', #92700, .T. ) ;
#98743 = CARTESIAN_POINT ( 'NONE',  ( 179.5000000000000000, -0.6250000000000003331, 6.000000000000000000 ) ) ;
#98744 = EDGE_CURVE ( 'NONE', #81857, #26026, #78922, .T. ) ;
#98745 = ORIENTED_EDGE ( 'NONE', *, *, #121797, .T. ) ;
#98746 = EDGE_CURVE ( 'NONE', #81852, #51338, #37057, .T. ) ;
#98747 = VERTEX_POINT ( 'NONE', #36941 ) ;
#98748 = ADVANCED_FACE ( 'NONE', ( #26474 ), #24526, .T. ) ;
#98749 = CARTESIAN_POINT ( 'NONE',  ( 185.6927083336747160, 6.551208109652275624, -3.782341765624998686 ) ) ;
#98751 = ADVANCED_FACE ( 'NONE', ( #44169 ), #115460, .F. ) ;
#98750 = CARTESIAN_POINT ( 'NONE',  ( 3.349999999999943689, 12.50000000000000000, 2.099970236277060032 ) ) ;
#98752 = DIRECTION ( 'NONE',  ( -0.000000000000000000, 1.000000000000000000, -0.000000000000000000 ) ) ;
#98753 = LINE ( 'NONE', #9093, #52721 ) ;
#98754 = DIRECTION ( 'NONE',  ( -0.000000000000000000, 1.000000000000000000, -0.000000000000000000 ) ) ;
#98755 = VECTOR ( 'NONE', #89352, 1000.000000000000000 ) ;
#98756 = CARTESIAN_POINT ( 'NONE',  ( 6.049999999999934097, 2.500000000000000000, 6.048780366869521252 ) ) ;
#98757 = CARTESIAN_POINT ( 'NONE',  ( -4.400000000000028777, 2.500000000000000000, -4.083716857408426826 ) ) ;
#98758 = AXIS2_PLACEMENT_3D ( 'NONE', #101466, #64107, #63474 ) ;
#98759 = CIRCLE ( 'NONE', #92504, 0.06509327318403745899 ) ;
#98760 = ADVANCED_FACE ( 'NONE', ( #6789 ), #24535, .T. ) ;
#98762 = ADVANCED_FACE ( 'NONE', ( #15981 ), #85151, .T. ) ;
#98761 = PLANE ( 'NONE',  #102286 ) ;
#98764 = ADVANCED_FACE ( 'NONE', ( #44831 ), #62193, .T. ) ;
#98763 = CIRCLE ( 'NONE', #42346, 0.06509327318403743123 ) ;
#98765 = VERTEX_POINT ( 'NONE', #126613 ) ;
#98766 = VECTOR ( 'NONE', #68677, 1000.000000000000000 ) ;
#98767 = AXIS2_PLACEMENT_3D ( 'NONE', #104681, #105346, #6456 ) ;
#98768 = EDGE_LOOP ( 'NONE', ( #70101, #58030 ) ) ;
#98769 = AXIS2_PLACEMENT_3D ( 'NONE', #29362, #39832, #128200 ) ;
#98770 = CIRCLE ( 'NONE', #48611, 0.06509327318403743123 ) ;
#98771 = PRODUCT_DEFINITION ( 'UNKNOWN', '', #19100, #66367 ) ;
#98772 = EDGE_LOOP ( 'NONE', ( #87962, #67881, #65496, #19472 ) ) ;
#98773 = ORIENTED_EDGE ( 'NONE', *, *, #104424, .T. ) ;
#98774 = FACE_OUTER_BOUND ( 'NONE', #108271, .T. ) ;
#98775 = DIRECTION ( 'NONE',  ( 0.000000000000000000, -0.000000000000000000, 1.000000000000000000 ) ) ;
#98776 = CONICAL_SURFACE ( 'NONE', #38254, 0.1000000000000002554, 0.003490658503988666988 ) ;
#98777 = VERTEX_POINT ( 'NONE', #94550 ) ;
#98778 = CARTESIAN_POINT ( 'NONE',  ( -7.300000000000016698, 2.500000000000000000, -0.2464101615137783419 ) ) ;
#98779 = DIRECTION ( 'NONE',  ( 0.000000000000000000, -0.9999939076577903929, 0.003490651415223739937 ) ) ;
#98780 = DIRECTION ( 'NONE',  ( -0.000000000000000000, 1.000000000000000000, -0.000000000000000000 ) ) ;
#98782 = EDGE_LOOP ( 'NONE', ( #83442, #129017 ) ) ;
#98781 = DIRECTION ( 'NONE',  ( 0.000000000000000000, 1.000000000000000000, 0.000000000000000000 ) ) ;
#98783 = DIRECTION ( 'NONE',  ( -0.000000000000000000, -1.000000000000000000, -0.000000000000000000 ) ) ;
#98784 = DIRECTION ( 'NONE',  ( -0.000000000000000000, -1.000000000000000000, -0.000000000000000000 ) ) ;
#98785 = ORIENTED_EDGE ( 'NONE', *, *, #89517, .F. ) ;
#98786 = VERTEX_POINT ( 'NONE', #76221 ) ;
#98787 = EDGE_LOOP ( 'NONE', ( #50169, #15806, #118668, #66029 ) ) ;
#98788 = ORIENTED_EDGE ( 'NONE', *, *, #93266, .F. ) ;
#98789 = CARTESIAN_POINT ( 'NONE',  ( -3.749999999999991118, 12.50000000000000000, -2.099970236277064473 ) ) ;
#98790 = AXIS2_PLACEMENT_3D ( 'NONE', #6838, #118107, #76902 ) ;
#98791 = CARTESIAN_POINT ( 'NONE',  ( 5.399999999999934630, 2.500000000000000000, 0.7928203230275495672 ) ) ;
#98792 = AXIS2_PLACEMENT_3D ( 'NONE', #128663, #17362, #38997 ) ;
#98793 = VECTOR ( 'NONE', #66173, 1000.000000000000000 ) ;
#98794 = VERTEX_POINT ( 'NONE', #14687 ) ;
#98795 = CARTESIAN_POINT ( 'NONE',  ( -9.550000000000007816, 2.500000000000000000, -6.595190528383296780 ) ) ;
#98796 = FACE_OUTER_BOUND ( 'NONE', #128307, .T. ) ;
#98797 = CARTESIAN_POINT ( 'NONE',  ( 1.649999999999951505, 12.50000000000000000, 2.922977105672686982 ) ) ;
#98798 = LINE ( 'NONE', #47785, #81795 ) ;
#98799 = ADVANCED_FACE ( 'NONE', ( #124675 ), #126938, .T. ) ;
#98800 = AXIS2_PLACEMENT_3D ( 'NONE', #54685, #59894, #129279 ) ;
#98801 = AXIS2_PLACEMENT_3D ( 'NONE', #71890, #93448, #33264 ) ;
#98802 = EDGE_CURVE ( 'NONE', #40796, #10550, #22494, .T. ) ;
#98803 = VECTOR ( 'NONE', #29021, 1000.000000000000000 ) ;
#98804 = VERTEX_POINT ( 'NONE', #25168 ) ;
#98805 = LINE ( 'NONE', #9145, #41620 ) ;
#98806 = AXIS2_PLACEMENT_3D ( 'NONE', #42130, #4752, #82714 ) ;
#98807 = EDGE_CURVE ( 'NONE', #120378, #896, #20322, .T. ) ;
#98808 = ORIENTED_EDGE ( 'NONE', *, *, #122057, .T. ) ;
#98809 = ORIENTED_EDGE ( 'NONE', *, *, #25524, .T. ) ;
#98810 = DIRECTION ( 'NONE',  ( 0.000000000000000000, 0.000000000000000000, -1.000000000000000000 ) ) ;
#98811 = CARTESIAN_POINT ( 'NONE',  ( 3.349999999999941025, 2.500000000000000000, 7.188010851410848723 ) ) ;
#98812 = FACE_BOUND ( 'NONE', #105179, .T. ) ;
#98813 = DIRECTION ( 'NONE',  ( 0.000000000000000000, 1.000000000000000000, 0.000000000000000000 ) ) ;
#98815 = AXIS2_PLACEMENT_3D ( 'NONE', #98814, #30108, #70020 ) ;
#98814 = CARTESIAN_POINT ( 'NONE',  ( -1.850000000000033840, 2.500000000000000000, 6.841600689897072485 ) ) ;
#98816 = EDGE_CURVE ( 'NONE', #71034, #91607, #124877, .T. ) ;
#98818 = CARTESIAN_POINT ( 'NONE',  ( 115.5000000000000000, -5.000000000000000000, 2.000000000000003553 ) ) ;
#98817 = CIRCLE ( 'NONE', #25660, 0.06509327318403745899 ) ;
#98819 = AXIS2_PLACEMENT_3D ( 'NONE', #119050, #59513, #99423 ) ;
#98820 = AXIS2_PLACEMENT_3D ( 'NONE', #72657, #41274, #53013 ) ;
#98821 = VERTEX_POINT ( 'NONE', #45482 ) ;
#98822 = DIRECTION ( 'NONE',  ( 0.000000000000000000, -0.000000000000000000, 1.000000000000000000 ) ) ;
#98823 = CARTESIAN_POINT ( 'NONE',  ( -9.800000000000006040, 12.50000000000000000, 4.676537180435972552 ) ) ;
#98824 = CARTESIAN_POINT ( 'NONE',  ( 6.649999999999931077, 2.500000000000000000, -6.395190528383301931 ) ) ;
#98825 = DIRECTION ( 'NONE',  ( 0.000000000000000000, 0.000000000000000000, -1.000000000000000000 ) ) ;
#98826 = EDGE_LOOP ( 'NONE', ( #127842, #29501 ) ) ;
#98827 = DIRECTION ( 'NONE',  ( -0.000000000000000000, 1.000000000000000000, -0.000000000000000000 ) ) ;
#98828 = DIRECTION ( 'NONE',  ( 0.000000000000000000, 0.000000000000000000, 1.000000000000000000 ) ) ;
#98829 = VERTEX_POINT ( 'NONE', #103744 ) ;
#98830 = ORIENTED_EDGE ( 'NONE', *, *, #19491, .T. ) ;
#98831 = CARTESIAN_POINT ( 'NONE',  ( 6.899999999999926636, 2.500000000000000000, 0.3464101615137736845 ) ) ;
#98832 = DIRECTION ( 'NONE',  ( 0.000000000000000000, 0.000000000000000000, 1.000000000000000000 ) ) ;
#98833 = EDGE_CURVE ( 'NONE', #112209, #36772, #27114, .T. ) ;
#98834 = FACE_BOUND ( 'NONE', #88842, .T. ) ;
#98835 = CARTESIAN_POINT ( 'NONE',  ( 9.599999999999914380, 2.500000000000000000, -4.230127018922201998 ) ) ;
#98836 = EDGE_LOOP ( 'NONE', ( #93229, #42940 ) ) ;
#98837 = CARTESIAN_POINT ( 'NONE',  ( 10.64999999999990976, 2.500000000000000000, -6.841600689897077814 ) ) ;
#98839 = ORIENTED_EDGE ( 'NONE', *, *, #87402, .F. ) ;
#98838 = CIRCLE ( 'NONE', #90530, 0.06509327318403745899 ) ;
#98841 = CIRCLE ( 'NONE', #103050, 0.09999999999999982514 ) ;
#98840 = CARTESIAN_POINT ( 'NONE',  ( 7.899999999999924860, 2.500000000000000000, -5.122947341949753763 ) ) ;
#98842 = CARTESIAN_POINT ( 'NONE',  ( 187.1250000000000284, -8.891194145520236347, -1.633285867636356693E-15 ) ) ;
#98843 = ORIENTED_EDGE ( 'NONE', *, *, #2018, .T. ) ;
#98844 = DIRECTION ( 'NONE',  ( 0.000000000000000000, -0.9999939076577903929, 0.003490651415223739937 ) ) ;
#98845 = DIRECTION ( 'NONE',  ( -4.274815082592931898E-19, -0.9999939076577903929, -0.003490651415223739937 ) ) ;
#98846 = AXIS2_PLACEMENT_3D ( 'NONE', #88152, #128110, #106525 ) ;
#98847 = EDGE_CURVE ( 'NONE', #76584, #103548, #9855, .T. ) ;
#98848 = AXIS2_PLACEMENT_3D ( 'NONE', #121577, #22769, #41120 ) ;
#98849 = AXIS2_PLACEMENT_3D ( 'NONE', #14712, #35043, #54642 ) ;
#98850 = FACE_OUTER_BOUND ( 'NONE', #40624, .T. ) ;
#98851 = DIRECTION ( 'NONE',  ( 0.000000000000000000, 0.000000000000000000, 1.000000000000000000 ) ) ;
#98852 = AXIS2_PLACEMENT_3D ( 'NONE', #21035, #83195, #62268 ) ;
#98854 = ORIENTED_EDGE ( 'NONE', *, *, #114715, .F. ) ;
#98853 = CIRCLE ( 'NONE', #4856, 0.06509327318403745899 ) ;
#98855 = VECTOR ( 'NONE', #25862, 1000.000000000000000 ) ;
#98856 = DIRECTION ( 'NONE',  ( 0.000000000000000000, 0.000000000000000000, 1.000000000000000000 ) ) ;
#98857 = FACE_OUTER_BOUND ( 'NONE', #26134, .T. ) ;
#98858 = DIRECTION ( 'NONE',  ( 0.000000000000000000, -0.9999939076577903929, 0.003490651415223739937 ) ) ;
#98859 = AXIS2_PLACEMENT_3D ( 'NONE', #56058, #114976, #96003 ) ;
#98860 = DIRECTION ( 'NONE',  ( -4.274815082592931898E-19, -0.9999939076577903929, -0.003490651415223739937 ) ) ;
#98862 = EDGE_LOOP ( 'NONE', ( #129153, #25818, #92745, #13423 ) ) ;
#98861 = CIRCLE ( 'NONE', #82156, 0.06509327318403745899 ) ;
#98863 = ORIENTED_EDGE ( 'NONE', *, *, #91246, .T. ) ;
#98864 = EDGE_CURVE ( 'NONE', #113013, #24462, #119351, .T. ) ;
#98865 = CARTESIAN_POINT ( 'NONE',  ( 16.56576425165006938, 1.499999999999999112, 6.084390597445819004 ) ) ;
#98866 = CIRCLE ( 'NONE', #80106, 0.06509327318403741736 ) ;
#98867 = ORIENTED_EDGE ( 'NONE', *, *, #119490, .F. ) ;
#98868 = FACE_OUTER_BOUND ( 'NONE', #1680, .T. ) ;
#98869 = CARTESIAN_POINT ( 'NONE',  ( 179.5000000000000000, -0.6250000000000000000, 7.634788798650553154 ) ) ;
#98870 = CARTESIAN_POINT ( 'NONE',  ( -6.250000000000015987, 12.50000000000000000, 1.472243186433545459 ) ) ;
#98871 = DIRECTION ( 'NONE',  ( 0.000000000000000000, 0.000000000000000000, -1.000000000000000000 ) ) ;
#98872 = ORIENTED_EDGE ( 'NONE', *, *, #104454, .T. ) ;
#98873 = DIRECTION ( 'NONE',  ( 0.000000000000000000, 0.000000000000000000, 1.000000000000000000 ) ) ;
#98874 = CARTESIAN_POINT ( 'NONE',  ( -12.89999999999999325, 2.500000000000000000, -3.737306695894647035 ) ) ;
#98875 = LINE ( 'NONE', #20328, #98659 ) ;
#98876 = EDGE_CURVE ( 'NONE', #73152, #97131, #51720, .T. ) ;
#98877 = CARTESIAN_POINT ( 'NONE',  ( 185.4427083336747160, -6.551208109652278289, 3.782341765624995134 ) ) ;
#98878 = DIRECTION ( 'NONE',  ( 0.000000000000000000, 0.000000000000000000, 1.000000000000000000 ) ) ;
#98879 = DIRECTION ( 'NONE',  ( 0.000000000000000000, 0.000000000000000000, -1.000000000000000000 ) ) ;
#98880 = CONICAL_SURFACE ( 'NONE', #126064, 0.1000000000000002554, 0.003490658503988666988 ) ;
#98881 = ORIENTED_EDGE ( 'NONE', *, *, #92835, .F. ) ;
#98882 = ORIENTED_EDGE ( 'NONE', *, *, #57527, .T. ) ;
#98883 = CARTESIAN_POINT ( 'NONE',  ( 4.399999999999937295, 12.50000000000000000, 3.983716857408420964 ) ) ;
#98884 = ORIENTED_EDGE ( 'NONE', *, *, #96476, .T. ) ;
#98885 = CARTESIAN_POINT ( 'NONE',  ( -4.600000000000024514, 2.500000000000000000, 4.922947341949748257 ) ) ;
#98887 = ORIENTED_EDGE ( 'NONE', *, *, #78435, .F. ) ;
#98886 = ORIENTED_EDGE ( 'NONE', *, *, #80240, .F. ) ;
#98888 = VERTEX_POINT ( 'NONE', #68967 ) ;
#98889 = CARTESIAN_POINT ( 'NONE',  ( 17.50000000000000000, -1.666666666666663632, -3.999999999999997335 ) ) ;
#98890 = CIRCLE ( 'NONE', #19467, 0.1000000000000002554 ) ;
#98891 = CIRCLE ( 'NONE', #689, 0.06509327318403745899 ) ;
#98892 = DIRECTION ( 'NONE',  ( 0.000000000000000000, 0.000000000000000000, -1.000000000000000000 ) ) ;
#98893 = AXIS2_PLACEMENT_3D ( 'NONE', #49144, #47196, #30144 ) ;
#98894 = DIRECTION ( 'NONE',  ( -0.000000000000000000, 1.000000000000000000, -0.000000000000000000 ) ) ;
#98895 = EDGE_CURVE ( 'NONE', #55057, #40266, #47517, .T. ) ;
#98896 = FILL_AREA_STYLE_COLOUR ( '', #116695 ) ;
#98897 = CARTESIAN_POINT ( 'NONE',  ( 5.849999999999931255, 2.500000000000000000, 2.957883832488649389 ) ) ;
#98898 = LINE ( 'NONE', #94234, #113406 ) ;
#98899 = LINE ( 'NONE', #39369, #114525 ) ;
#98900 = DIRECTION ( 'NONE',  ( 0.000000000000000000, 0.000000000000000000, 1.000000000000000000 ) ) ;
#98901 = AXIS2_PLACEMENT_3D ( 'NONE', #106704, #56316, #126361 ) ;
#98902 = AXIS2_PLACEMENT_3D ( 'NONE', #6323, #84260, #24069 ) ;
#98903 = DIRECTION ( 'NONE',  ( -4.274815082592931898E-19, -0.9999939076577903929, -0.003490651415223739937 ) ) ;
#98904 = EDGE_LOOP ( 'NONE', ( #23309, #4238, #48703, #126842 ) ) ;
#98906 = ADVANCED_FACE ( 'NONE', ( #59831 ), #68318, .T. ) ;
#98905 = CIRCLE ( 'NONE', #128161, 0.06509327318403745899 ) ;
#98907 = VERTEX_POINT ( 'NONE', #87308 ) ;
#98908 = AXIS2_PLACEMENT_3D ( 'NONE', #35543, #66906, #27004 ) ;
#98909 = CARTESIAN_POINT ( 'NONE',  ( -8.150000000000012790, 2.500000000000000000, -1.818653347947326138 ) ) ;
#98910 = EDGE_CURVE ( 'NONE', #125538, #80531, #3593, .T. ) ;
#98911 = ORIENTED_EDGE ( 'NONE', *, *, #78420, .T. ) ;
#98912 = ADVANCED_FACE ( 'NONE', ( #10055 ), #66286, .T. ) ;
#98913 = EDGE_LOOP ( 'NONE', ( #21299, #78218, #72967, #32021 ) ) ;
#98914 = EDGE_CURVE ( 'NONE', #21836, #3798, #93487, .T. ) ;
#98915 = CARTESIAN_POINT ( 'NONE',  ( 5.799999999999931433, 2.500000000000000000, 4.330127018922196314 ) ) ;
#98916 = EDGE_CURVE ( 'NONE', #73210, #4103, #18583, .T. ) ;
#98917 = CONICAL_SURFACE ( 'NONE', #42501, 0.1000000000000002554, 0.003490658503988666988 ) ;
#98918 = CARTESIAN_POINT ( 'NONE',  ( -5.600000000000023626, 2.500000000000000000, -4.776537180435977525 ) ) ;
#98919 = DIRECTION ( 'NONE',  ( -0.000000000000000000, 1.000000000000000000, -0.000000000000000000 ) ) ;
#98920 = CIRCLE ( 'NONE', #46691, 0.06509327318403745899 ) ;
#98921 = CARTESIAN_POINT ( 'NONE',  ( 4.149999999999941735, 12.50000000000000000, -7.253104124594891289 ) ) ;
#98922 = AXIS2_PLACEMENT_3D ( 'NONE', #65097, #106335, #125962 ) ;
#98923 = CONICAL_SURFACE ( 'NONE', #55000, 0.1000000000000002554, 0.003490658503988666988 ) ;
#98924 = EDGE_CURVE ( 'NONE', #107468, #62993, #80961, .T. ) ;
#98925 = DIRECTION ( 'NONE',  ( 0.000000000000000000, 0.000000000000000000, 1.000000000000000000 ) ) ;
#98926 = ORIENTED_EDGE ( 'NONE', *, *, #3150, .F. ) ;
#98927 = EDGE_CURVE ( 'NONE', #34370, #29668, #114398, .T. ) ;
#98928 = CONICAL_SURFACE ( 'NONE', #11078, 0.09999999999999982514, 0.003490658503988666988 ) ;
#98929 = ADVANCED_FACE ( 'NONE', ( #8109 ), #122727, .T. ) ;
#98930 = EDGE_CURVE ( 'NONE', #106895, #122432, #59165, .T. ) ;
#98931 = VERTEX_POINT ( 'NONE', #19204 ) ;
#98932 = CARTESIAN_POINT ( 'NONE',  ( -12.04999999999999538, 2.500000000000000000, 6.495190528383297135 ) ) ;
#98933 = EDGE_CURVE ( 'NONE', #105604, #48799, #28741, .T. ) ;
#98934 = VERTEX_POINT ( 'NONE', #78159 ) ;
#98935 = AXIS2_PLACEMENT_3D ( 'NONE', #67124, #70874, #16099 ) ;
#98936 = LINE ( 'NONE', #9267, #42070 ) ;
#98937 = ORIENTED_EDGE ( 'NONE', *, *, #16899, .T. ) ;
#98938 = ORIENTED_EDGE ( 'NONE', *, *, #37041, .F. ) ;
#98939 = EDGE_CURVE ( 'NONE', #117692, #122978, #79015, .T. ) ;
#98940 = DIRECTION ( 'NONE',  ( -4.274815082592931898E-19, -0.9999939076577903929, -0.003490651415223739937 ) ) ;
#98941 = LINE ( 'NONE', #68830, #127963 ) ;
#98942 = DIRECTION ( 'NONE',  ( 0.000000000000000000, 0.000000000000000000, 1.000000000000000000 ) ) ;
#98943 = CARTESIAN_POINT ( 'NONE',  ( 0.1999999999999571565, 2.500000000000000000, 4.083716857408420609 ) ) ;
#98944 = CARTESIAN_POINT ( 'NONE',  ( 4.999999999999971578, 2.500000000000000000, -0.1000000000000022815 ) ) ;
#98945 = EDGE_LOOP ( 'NONE', ( #51623, #9681 ) ) ;
#98946 = CARTESIAN_POINT ( 'NONE',  ( -8.550000000000013145, 12.50000000000000000, -6.906693963081110610 ) ) ;
#98947 = CARTESIAN_POINT ( 'NONE',  ( 11.64999999999990443, 2.500000000000000000, -7.188010851410854052 ) ) ;
#98948 = AXIS2_PLACEMENT_3D ( 'NONE', #122383, #10472, #123023 ) ;
#98949 = CARTESIAN_POINT ( 'NONE',  ( 13.14999999999990088, 12.50000000000000000, 2.446380397790835826 ) ) ;
#98950 = CARTESIAN_POINT ( 'NONE',  ( -11.64999999999999680, 12.50000000000000000, 1.407149913249508000 ) ) ;
#98951 = CARTESIAN_POINT ( 'NONE',  ( -1.250000000000037970, 2.500000000000000000, 2.957883832488649389 ) ) ;
#98952 = ORIENTED_EDGE ( 'NONE', *, *, #89888, .T. ) ;
#98953 = AXIS2_PLACEMENT_3D ( 'NONE', #42311, #82233, #50838 ) ;
#98954 = VERTEX_POINT ( 'NONE', #50001 ) ;
#98955 = AXIS2_PLACEMENT_3D ( 'NONE', #114341, #34521, #124163 ) ;
#98956 = CARTESIAN_POINT ( 'NONE',  ( -2.900000000000029221, 12.50000000000000000, -0.06509327318403970719 ) ) ;
#98957 = EDGE_LOOP ( 'NONE', ( #64243, #104555, #7836, #32217 ) ) ;
#98958 = CARTESIAN_POINT ( 'NONE',  ( 6.649999999999929301, 2.500000000000000000, 6.395190528383296602 ) ) ;
#98959 = CARTESIAN_POINT ( 'NONE',  ( -3.150000000000032330, 2.500000000000000000, -6.248780366869526759 ) ) ;
#98960 = AXIS2_PLACEMENT_3D ( 'NONE', #128547, #11319, #38214 ) ;
#98961 = CIRCLE ( 'NONE', #38335, 0.1000000000000000472 ) ;
#98962 = VECTOR ( 'NONE', #16122, 1000.000000000000000 ) ;
#98963 = CIRCLE ( 'NONE', #661, 0.1000000000000002554 ) ;
#98964 = VERTEX_POINT ( 'NONE', #89894 ) ;
#98965 = LINE ( 'NONE', #49240, #82881 ) ;
#98966 = CARTESIAN_POINT ( 'NONE',  ( -9.800000000000006040, 2.500000000000000000, -4.776537180435973973 ) ) ;
#98967 = CARTESIAN_POINT ( 'NONE',  ( -12.49999999999999467, 2.500000000000000000, 0.6928203230275535862 ) ) ;
#98968 = DIRECTION ( 'NONE',  ( 0.000000000000000000, -0.000000000000000000, 1.000000000000000000 ) ) ;
#98969 = ORIENTED_EDGE ( 'NONE', *, *, #52508, .T. ) ;
#98970 = CIRCLE ( 'NONE', #69427, 0.06509327318403745899 ) ;
#98971 = EDGE_CURVE ( 'NONE', #93899, #119348, #89457, .T. ) ;
#98972 = CARTESIAN_POINT ( 'NONE',  ( 2.899999999999945732, 2.500000000000000000, -0.1000000000000023925 ) ) ;
#98973 = EDGE_CURVE ( 'NONE', #25372, #99497, #104037, .T. ) ;
#98974 = ORIENTED_EDGE ( 'NONE', *, *, #125597, .F. ) ;
#98975 = CARTESIAN_POINT ( 'NONE',  ( -4.350000000000027178, 2.500000000000000000, -6.741600689897077281 ) ) ;
#98976 = LINE ( 'NONE', #30260, #97853 ) ;
#98977 = DIRECTION ( 'NONE',  ( 0.000000000000000000, 0.000000000000000000, -1.000000000000000000 ) ) ;
#98978 = VECTOR ( 'NONE', #70175, 1000.000000000000000 ) ;
#98979 = EDGE_CURVE ( 'NONE', #35537, #83674, #43423, .T. ) ;
#98980 = ORIENTED_EDGE ( 'NONE', *, *, #34484, .F. ) ;
#98981 = CARTESIAN_POINT ( 'NONE',  ( 5.849999999999932143, 2.500000000000000000, 2.165063509461097713 ) ) ;
#98982 = VERTEX_POINT ( 'NONE', #48694 ) ;
#98983 = CARTESIAN_POINT ( 'NONE',  ( 5.649999999999936406, 12.50000000000000000, -6.841600689897077814 ) ) ;
#98984 = DIRECTION ( 'NONE',  ( 0.000000000000000000, 0.000000000000000000, 1.000000000000000000 ) ) ;
#98985 = DIRECTION ( 'NONE',  ( -0.000000000000000000, -1.000000000000000000, -0.000000000000000000 ) ) ;
#98986 = CONICAL_SURFACE ( 'NONE', #86364, 0.09999999999999999167, 0.003490658503988666988 ) ;
#98987 = ORIENTED_EDGE ( 'NONE', *, *, #15566, .T. ) ;
#98988 = AXIS2_PLACEMENT_3D ( 'NONE', #38162, #78753, #76802 ) ;
#98989 = AXIS2_PLACEMENT_3D ( 'NONE', #23304, #22694, #21380 ) ;
#98990 = CARTESIAN_POINT ( 'NONE',  ( -0.8500000000000386136, 12.50000000000000000, 2.857883832488649301 ) ) ;
#98991 = CARTESIAN_POINT ( 'NONE',  ( -11.84999999999999787, 2.500000000000000000, -6.741600689897073728 ) ) ;
#98992 = ORIENTED_EDGE ( 'NONE', *, *, #116899, .T. ) ;
#98993 = FACE_OUTER_BOUND ( 'NONE', #124027, .T. ) ;
#98994 = AXIS2_PLACEMENT_3D ( 'NONE', #83073, #12378, #93525 ) ;
#98995 = EDGE_LOOP ( 'NONE', ( #82782, #102005, #86764, #107556 ) ) ;
#98996 = CIRCLE ( 'NONE', #111613, 0.1000000000000002554 ) ;
#98997 = DIRECTION ( 'NONE',  ( -0.000000000000000000, 1.000000000000000000, -0.000000000000000000 ) ) ;
#98998 = AXIS2_PLACEMENT_3D ( 'NONE', #36447, #66514, #127390 ) ;
#98999 = ORIENTED_EDGE ( 'NONE', *, *, #65640, .T. ) ;
#99000 = CARTESIAN_POINT ( 'NONE',  ( 108.0000000000000142, 8.500000000000000000, -0.2500000000000000000 ) ) ;
#99001 = DIRECTION ( 'NONE',  ( 0.000000000000000000, 0.000000000000000000, 1.000000000000000000 ) ) ;
#99002 = ORIENTED_EDGE ( 'NONE', *, *, #1060, .T. ) ;
#99003 = ORIENTED_EDGE ( 'NONE', *, *, #57740, .F. ) ;
#99004 = CIRCLE ( 'NONE', #73970, 0.09999999999999982514 ) ;
#99005 = LINE ( 'NONE', #37522, #76041 ) ;
#99006 = DIRECTION ( 'NONE',  ( 0.000000000000000000, 0.000000000000000000, 1.000000000000000000 ) ) ;
#99007 = EDGE_LOOP ( 'NONE', ( #74495, #99600 ) ) ;
#99009 = ADVANCED_FACE ( 'NONE', ( #88611 ), #33047, .T. ) ;
#99008 = DIRECTION ( 'NONE',  ( 0.000000000000000000, 1.000000000000000000, 0.000000000000000000 ) ) ;
#99010 = CARTESIAN_POINT ( 'NONE',  ( 186.8177083336747160, 4.367472073101515306, 7.564683531250000925 ) ) ;
#99011 = CONICAL_SURFACE ( 'NONE', #44737, 0.09999999999999982514, 0.003490658503988666988 ) ;
#99013 = CIRCLE ( 'NONE', #96950, 0.06509327318403741736 ) ;
#99012 = DIRECTION ( 'NONE',  ( -0.000000000000000000, -1.000000000000000000, -0.000000000000000000 ) ) ;
#99014 = CONICAL_SURFACE ( 'NONE', #92763, 0.09999999999999999167, 0.003490658503988666988 ) ;
#99015 = CARTESIAN_POINT ( 'NONE',  ( 102.9998079663853900, 8.700110364096246940, -0.1627839287194029205 ) ) ;
#99016 = DIRECTION ( 'NONE',  ( 0.000000000000000000, -0.9999939076577903929, 0.003490651415223739937 ) ) ;
#99017 = CARTESIAN_POINT ( 'NONE',  ( 8.349999999999919709, 2.500000000000000000, 7.188010851410848723 ) ) ;
#99018 = AXIS2_PLACEMENT_3D ( 'NONE', #40270, #8211, #70365 ) ;
#99019 = CARTESIAN_POINT ( 'NONE',  ( -5.800000000000022027, 2.500000000000000000, -4.330127018922201643 ) ) ;
#99020 = AXIS2_PLACEMENT_3D ( 'NONE', #25103, #65007, #53297 ) ;
#99021 = ORIENTED_EDGE ( 'NONE', *, *, #121783, .F. ) ;
#99022 = ORIENTED_EDGE ( 'NONE', *, *, #97501, .F. ) ;
#99023 = ORIENTED_EDGE ( 'NONE', *, *, #24263, .T. ) ;
#99024 = ORIENTED_EDGE ( 'NONE', *, *, #15713, .F. ) ;
#99025 = CARTESIAN_POINT ( 'NONE',  ( -10.65000000000000391, 2.500000000000000000, -6.148780366869522673 ) ) ;
#99026 = CARTESIAN_POINT ( 'NONE',  ( 87.50000000000001421, 0.000000000000000000, 0.000000000000000000 ) ) ;
#99027 = ADVANCED_FACE ( 'NONE', ( #22474 ), #102309, .T. ) ;
#99028 = DIRECTION ( 'NONE',  ( 0.000000000000000000, 0.000000000000000000, -1.000000000000000000 ) ) ;
#99029 = ORIENTED_EDGE ( 'NONE', *, *, #52108, .T. ) ;
#99030 = FACE_BOUND ( 'NONE', #128256, .T. ) ;
#99031 = EDGE_LOOP ( 'NONE', ( #29796, #113418 ) ) ;
#99032 = ADVANCED_FACE ( 'NONE', ( #42097 ), #47610, .T. ) ;
#99033 = DIRECTION ( 'NONE',  ( -4.274815082592931898E-19, -0.9999939076577903929, -0.003490651415223739937 ) ) ;
#99034 = DIRECTION ( 'NONE',  ( -0.000000000000000000, -1.000000000000000000, -0.000000000000000000 ) ) ;
#99035 = DIRECTION ( 'NONE',  ( 0.000000000000000000, -0.9999939076577903929, 0.003490651415223739937 ) ) ;
#99036 = DIRECTION ( 'NONE',  ( 0.000000000000000000, 0.000000000000000000, -1.000000000000000000 ) ) ;
#99037 = CARTESIAN_POINT ( 'NONE',  ( 4.149999999999941735, 12.50000000000000000, -5.802370205355749988 ) ) ;
#99038 = CARTESIAN_POINT ( 'NONE',  ( 11.04999999999991189, 2.500000000000000000, -2.511473670974877948 ) ) ;
#99039 = DIRECTION ( 'NONE',  ( 0.000000000000000000, 1.000000000000000000, 0.000000000000000000 ) ) ;
#99040 = DIRECTION ( 'NONE',  ( 0.000000000000000000, 1.000000000000000000, 0.000000000000000000 ) ) ;
#99041 = VECTOR ( 'NONE', #96020, 1000.000000000000000 ) ;
#99042 = CIRCLE ( 'NONE', #34302, 0.1000000000000000472 ) ;
#99043 = EDGE_CURVE ( 'NONE', #98765, #23160, #53866, .T. ) ;
#99044 = PLANE ( 'NONE',  #47687 ) ;
#99045 = CARTESIAN_POINT ( 'NONE',  ( -4.600000000000028955, 12.50000000000000000, -4.330127018922201643 ) ) ;
#99047 = ORIENTED_EDGE ( 'NONE', *, *, #52692, .T. ) ;
#99046 = CIRCLE ( 'NONE', #117801, 0.09999999999999982514 ) ;
#99048 = ORIENTED_EDGE ( 'NONE', *, *, #90423, .T. ) ;
#99049 = ORIENTED_EDGE ( 'NONE', *, *, #94660, .F. ) ;
#99050 = AXIS2_PLACEMENT_3D ( 'NONE', #112166, #99770, #100412 ) ;
#99051 = ORIENTED_EDGE ( 'NONE', *, *, #101021, .T. ) ;
#99052 = MANIFOLD_SOLID_BREP ( 'Cut-Extrude-Thin1', #68669 ) ;
#99054 = AXIS2_PLACEMENT_3D ( 'NONE', #69107, #39045, #108390 ) ;
#99053 = DIRECTION ( 'NONE',  ( -4.274815082592931898E-19, -0.9999939076577903929, -0.003490651415223739937 ) ) ;
#99055 = CONICAL_SURFACE ( 'NONE', #92799, 0.09999999999999982514, 0.003490658503988666988 ) ;
#99056 = DIRECTION ( 'NONE',  ( 0.000000000000000000, 1.000000000000000000, 0.000000000000000000 ) ) ;
#99057 = UNCERTAINTY_MEASURE_WITH_UNIT (LENGTH_MEASURE( 1.000000000000000082E-05 ), #67478, 'distance_accuracy_value', 'NONE');
#99059 = EDGE_LOOP ( 'NONE', ( #51626, #24026 ) ) ;
#99058 = EDGE_LOOP ( 'NONE', ( #102721, #8142 ) ) ;
#99060 = EDGE_LOOP ( 'NONE', ( #127357, #3802, #121388, #49304 ) ) ;
#99061 = CARTESIAN_POINT ( 'NONE',  ( 3.949999999999940670, 12.50000000000000000, 1.818653347947321475 ) ) ;
#99062 = AXIS2_PLACEMENT_3D ( 'NONE', #52927, #91561, #62113 ) ;
#99063 = VECTOR ( 'NONE', #36644, 1000.000000000000000 ) ;
#99064 = DIRECTION ( 'NONE',  ( 0.000000000000000000, 1.000000000000000000, 0.000000000000000000 ) ) ;
#99065 = DIRECTION ( 'NONE',  ( -0.000000000000000000, -1.000000000000000000, -0.000000000000000000 ) ) ;
#99066 = PLANE ( 'NONE',  #87649 ) ;
#99067 = CARTESIAN_POINT ( 'NONE',  ( 4.399999999999939071, 2.500000000000000000, -0.2464101615137782308 ) ) ;
#99068 = DIRECTION ( 'NONE',  ( 0.000000000000000000, -0.000000000000000000, 1.000000000000000000 ) ) ;
#99069 = CIRCLE ( 'NONE', #73920, 0.09999999999999982514 ) ;
#99070 = FACE_OUTER_BOUND ( 'NONE', #3852, .T. ) ;
#99071 = ORIENTED_EDGE ( 'NONE', *, *, #37457, .T. ) ;
#99072 = DIRECTION ( 'NONE',  ( 0.000000000000000000, 1.000000000000000000, 0.000000000000000000 ) ) ;
#99073 = ORIENTED_EDGE ( 'NONE', *, *, #9112, .T. ) ;
#99074 = EDGE_CURVE ( 'NONE', #70902, #77506, #20415, .T. ) ;
#99075 = EDGE_LOOP ( 'NONE', ( #89067, #1310, #29031 ) ) ;
#99076 = ORIENTED_EDGE ( 'NONE', *, *, #16163, .F. ) ;
#99077 = CARTESIAN_POINT ( 'NONE',  ( 0.3999999999999568345, 12.50000000000000000, -3.637306695894650055 ) ) ;
#99078 = ORIENTED_EDGE ( 'NONE', *, *, #77039, .F. ) ;
#99079 = EDGE_CURVE ( 'NONE', #112495, #84287, #5810, .T. ) ;
#99080 = VERTEX_POINT ( 'NONE', #23095 ) ;
#99081 = EDGE_CURVE ( 'NONE', #9996, #77958, #12088, .T. ) ;
#99082 = AXIS2_PLACEMENT_3D ( 'NONE', #58274, #28161, #49105 ) ;
#99083 = DIRECTION ( 'NONE',  ( 0.000000000000000000, 1.000000000000000000, 0.000000000000000000 ) ) ;
#99084 = CARTESIAN_POINT ( 'NONE',  ( 6.049999999999930544, 12.50000000000000000, 2.511473670974873507 ) ) ;
#99085 = DIRECTION ( 'NONE',  ( 0.000000000000000000, 0.000000000000000000, 1.000000000000000000 ) ) ;
#99086 = DIRECTION ( 'NONE',  ( 0.000000000000000000, 0.000000000000000000, 1.000000000000000000 ) ) ;
#99087 = EDGE_CURVE ( 'NONE', #106434, #59553, #31631, .T. ) ;
#99088 = ADVANCED_FACE ( 'NONE', ( #111463 ), #66459, .T. ) ;
#99089 = CARTESIAN_POINT ( 'NONE',  ( -12.89999999999999147, 12.50000000000000000, -4.330127018922198978 ) ) ;
#99090 = EDGE_CURVE ( 'NONE', #73842, #102428, #50611, .T. ) ;
#99091 = ORIENTED_EDGE ( 'NONE', *, *, #37719, .F. ) ;
#99092 = CARTESIAN_POINT ( 'NONE',  ( -13.54999999999999005, 12.50000000000000000, -1.818653347947323917 ) ) ;
#99093 = CIRCLE ( 'NONE', #82376, 0.09999999999999982514 ) ;
#99094 = AXIS2_PLACEMENT_3D ( 'NONE', #17682, #78572, #118464 ) ;
#99095 = ORIENTED_EDGE ( 'NONE', *, *, #19721, .T. ) ;
#99096 = CARTESIAN_POINT ( 'NONE',  ( -2.700000000000030820, 12.50000000000000000, 0.3464101615137735735 ) ) ;
#99097 = ADVANCED_FACE ( 'NONE', ( #120650 ), #53212, .T. ) ;
#99098 = ORIENTED_EDGE ( 'NONE', *, *, #33435, .F. ) ;
#99099 = CARTESIAN_POINT ( 'NONE',  ( 112.9585346383515230, 8.676224923738738326, 0.6641129214945534764 ) ) ;
#99100 = DIRECTION ( 'NONE',  ( 0.000000000000000000, 1.000000000000000000, 0.000000000000000000 ) ) ;
#99101 = ORIENTED_EDGE ( 'NONE', *, *, #116547, .T. ) ;
#99102 = CARTESIAN_POINT ( 'NONE',  ( 9.599999999999914380, 2.500000000000000000, -4.430127018922202176 ) ) ;
#99104 = CONICAL_SURFACE ( 'NONE', #42679, 0.09999999999999982514, 0.003490658503988666988 ) ;
#99103 = DIRECTION ( 'NONE',  ( -4.274815082592931898E-19, -0.9999939076577903929, -0.003490651415223739937 ) ) ;
#99105 = ORIENTED_EDGE ( 'NONE', *, *, #19711, .T. ) ;
#99106 = EDGE_CURVE ( 'NONE', #63978, #90160, #7876, .T. ) ;
#99107 = AXIS2_PLACEMENT_3D ( 'NONE', #113613, #54053, #124722 ) ;
#99108 = CARTESIAN_POINT ( 'NONE',  ( 7.899999999999924860, 2.500000000000000000, 4.330127018922196314 ) ) ;
#99109 = EDGE_LOOP ( 'NONE', ( #57038, #87468, #44360, #98093 ) ) ;
#99110 = VERTEX_POINT ( 'NONE', #61749 ) ;
#99111 = DIRECTION ( 'NONE',  ( -0.000000000000000000, 1.000000000000000000, -0.000000000000000000 ) ) ;
#99112 = LINE ( 'NONE', #1534, #15875 ) ;
#99113 = CARTESIAN_POINT ( 'NONE',  ( 184.4635416670080588, -4.367472073101519747, 7.564683531249999149 ) ) ;
#99114 = CARTESIAN_POINT ( 'NONE',  ( 1.649999999999951505, 12.50000000000000000, -2.857883832488653741 ) ) ;
#99115 = FACE_OUTER_BOUND ( 'NONE', #90178, .T. ) ;
#99116 = ORIENTED_EDGE ( 'NONE', *, *, #84747, .F. ) ;
#99117 = AXIS2_PLACEMENT_3D ( 'NONE', #42673, #71447, #101572 ) ;
#99118 = AXIS2_PLACEMENT_3D ( 'NONE', #112560, #22895, #62812 ) ;
#99119 = CONICAL_SURFACE ( 'NONE', #80335, 0.1000000000000000472, 0.003490658503988666988 ) ;
#99120 = CARTESIAN_POINT ( 'NONE',  ( -11.05000000000000249, 2.500000000000000000, -6.148780366869522673 ) ) ;
#99121 = CIRCLE ( 'NONE', #46798, 0.1000000000000002554 ) ;
#99122 = VERTEX_POINT ( 'NONE', #51922 ) ;
#99123 = AXIS2_PLACEMENT_3D ( 'NONE', #21393, #103184, #91430 ) ;
#99124 = CARTESIAN_POINT ( 'NONE',  ( 187.5000000000000000, 0.000000000000000000, 7.700000000000000178 ) ) ;
#99125 = CARTESIAN_POINT ( 'NONE',  ( 187.5000000000000000, -1.000000000000025535, -7.634788798650553154 ) ) ;
#99126 = DIRECTION ( 'NONE',  ( 0.000000000000000000, 0.000000000000000000, -1.000000000000000000 ) ) ;
#99127 = CARTESIAN_POINT ( 'NONE',  ( -13.74999999999998757, 2.500000000000000000, -2.857883832488651521 ) ) ;
#99128 = CARTESIAN_POINT ( 'NONE',  ( -4.550000000000026468, 2.500000000000000000, -6.495190528383302464 ) ) ;
#99129 = FACE_OUTER_BOUND ( 'NONE', #60965, .T. ) ;
#99130 = CARTESIAN_POINT ( 'NONE',  ( 0.4499999999999569344, 2.500000000000000000, 2.065063509461097624 ) ) ;
#99131 = EDGE_LOOP ( 'NONE', ( #123137, #69276 ) ) ;
#99133 = ADVANCED_FACE ( 'NONE', ( #91839 ), #81063, .T. ) ;
#99132 = DIRECTION ( 'NONE',  ( 0.000000000000000000, -0.9999939076577903929, 0.003490651415223739937 ) ) ;
#99134 = CARTESIAN_POINT ( 'NONE',  ( -9.400000000000007461, 12.50000000000000000, 4.676537180435972552 ) ) ;
#99135 = PLANE ( 'NONE',  #129089 ) ;
#99136 = AXIS2_PLACEMENT_3D ( 'NONE', #31798, #42264, #110972 ) ;
#99137 = AXIS2_PLACEMENT_3D ( 'NONE', #5010, #84216, #35777 ) ;
#99138 = ORIENTED_EDGE ( 'NONE', *, *, #35672, .F. ) ;
#99139 = DIRECTION ( 'NONE',  ( 0.000000000000000000, -0.000000000000000000, 1.000000000000000000 ) ) ;
#99140 = EDGE_CURVE ( 'NONE', #28690, #86599, #62280, .T. ) ;
#99141 = VECTOR ( 'NONE', #122343, 1000.000000000000000 ) ;
#99142 = CIRCLE ( 'NONE', #44767, 0.09999999999999982514 ) ;
#99143 = VERTEX_POINT ( 'NONE', #124526 ) ;
#99144 = CIRCLE ( 'NONE', #42737, 0.06509327318403741736 ) ;
#99145 = VERTEX_POINT ( 'NONE', #115302 ) ;
#99146 = CARTESIAN_POINT ( 'NONE',  ( 13.34999999999990017, 2.500000000000000000, 1.472243186433545459 ) ) ;
#99147 = VECTOR ( 'NONE', #91025, 1000.000000000000000 ) ;
#99148 = ORIENTED_EDGE ( 'NONE', *, *, #127000, .F. ) ;
#99149 = DIRECTION ( 'NONE',  ( 0.000000000000000000, 1.000000000000000000, 0.000000000000000000 ) ) ;
#99150 = CARTESIAN_POINT ( 'NONE',  ( -4.076600168545496672E-14, 2.500000000000000000, -5.022947341949754119 ) ) ;
#99152 = ORIENTED_EDGE ( 'NONE', *, *, #125351, .T. ) ;
#99151 = AXIS2_PLACEMENT_3D ( 'NONE', #112336, #120224, #30573 ) ;
#99153 = CIRCLE ( 'NONE', #92902, 0.1000000000000002554 ) ;
#99154 = CIRCLE ( 'NONE', #32276, 0.06509327318403745899 ) ;
#99155 = DIRECTION ( 'NONE',  ( 0.000000000000000000, 1.000000000000000000, 0.000000000000000000 ) ) ;
#99157 = ORIENTED_EDGE ( 'NONE', *, *, #40565, .F. ) ;
#99156 = DIRECTION ( 'NONE',  ( 0.000000000000000000, 0.000000000000000000, 1.000000000000000000 ) ) ;
#99158 = VECTOR ( 'NONE', #107295, 1000.000000000000000 ) ;
#99159 = LINE ( 'NONE', #46839, #23498 ) ;
#99160 = CARTESIAN_POINT ( 'NONE',  ( 12.49999999999990585, 12.50000000000000000, 3.637306695894644726 ) ) ;
#99161 = EDGE_LOOP ( 'NONE', ( #8703, #23315 ) ) ;
#99162 = ORIENTED_EDGE ( 'NONE', *, *, #16648, .T. ) ;
#99163 = VERTEX_POINT ( 'NONE', #94397 ) ;
#99164 = DIRECTION ( 'NONE',  ( 0.000000000000000000, 1.000000000000000000, 0.000000000000000000 ) ) ;
#99165 = CARTESIAN_POINT ( 'NONE',  ( -12.49999999999995914, 12.50000000000000000, -4.330127018922198978 ) ) ;
#99166 = DIRECTION ( 'NONE',  ( 0.000000000000000000, -0.000000000000000000, 1.000000000000000000 ) ) ;
#99167 = FACE_BOUND ( 'NONE', #60663, .T. ) ;
#99168 = ORIENTED_EDGE ( 'NONE', *, *, #57268, .F. ) ;
#99169 = DIRECTION ( 'NONE',  ( 0.000000000000000000, 0.000000000000000000, 1.000000000000000000 ) ) ;
#99170 = FACE_OUTER_BOUND ( 'NONE', #91489, .T. ) ;
#99171 = CONICAL_SURFACE ( 'NONE', #97106, 0.1000000000000002554, 0.003490658503988666988 ) ;
#99172 = VERTEX_POINT ( 'NONE', #105525 ) ;
#99174 = EDGE_CURVE ( 'NONE', #69479, #85617, #66228, .T. ) ;
#99173 = LINE ( 'NONE', #109637, #105123 ) ;
#99175 = DIRECTION ( 'NONE',  ( 0.000000000000000000, 0.000000000000000000, 1.000000000000000000 ) ) ;
#99176 = CARTESIAN_POINT ( 'NONE',  ( 0.1999999999999636513, 12.50000000000000000, -0.4115034346978134749 ) ) ;
#99177 = CARTESIAN_POINT ( 'NONE',  ( -12.89999999999999147, 2.500000000000000000, 4.430127018922196847 ) ) ;
#99178 = DIRECTION ( 'NONE',  ( 0.000000000000000000, -0.9999939076577903929, 0.003490651415223739937 ) ) ;
#99179 = DIRECTION ( 'NONE',  ( -0.000000000000000000, 1.000000000000000000, -0.000000000000000000 ) ) ;
#99180 = FACE_OUTER_BOUND ( 'NONE', #14216, .T. ) ;
#99181 = VECTOR ( 'NONE', #12236, 1000.000000000000000 ) ;
#99182 = EDGE_CURVE ( 'NONE', #19500, #87143, #10046, .T. ) ;
#99183 = CIRCLE ( 'NONE', #101335, 0.1000000000000002554 ) ;
#99184 = ORIENTED_EDGE ( 'NONE', *, *, #794, .F. ) ;
#99185 = ORIENTED_EDGE ( 'NONE', *, *, #47803, .F. ) ;
#99186 = ORIENTED_EDGE ( 'NONE', *, *, #58314, .T. ) ;
#99187 = ORIENTED_EDGE ( 'NONE', *, *, #551, .F. ) ;
#99188 = ORIENTED_EDGE ( 'NONE', *, *, #5528, .F. ) ;
#99189 = DIRECTION ( 'NONE',  ( 0.000000000000000000, 0.000000000000000000, -1.000000000000000000 ) ) ;
#99190 = EDGE_CURVE ( 'NONE', #22979, #110935, #108237, .T. ) ;
#99191 = CARTESIAN_POINT ( 'NONE',  ( 6.699999999999930012, 2.500000000000000000, 4.230127018922196669 ) ) ;
#99192 = ORIENTED_EDGE ( 'NONE', *, *, #99412, .F. ) ;
#99193 = FACE_BOUND ( 'NONE', #128645, .T. ) ;
#99194 = EDGE_CURVE ( 'NONE', #15146, #43992, #63675, .T. ) ;
#99195 = CARTESIAN_POINT ( 'NONE',  ( 7.499999999999927169, 2.500000000000000000, -5.022947341949754119 ) ) ;
#99196 = CIRCLE ( 'NONE', #57330, 0.06509327318403745899 ) ;
#99197 = EDGE_CURVE ( 'NONE', #92369, #15915, #83206, .T. ) ;
#99198 = CARTESIAN_POINT ( 'NONE',  ( -4.550000000000022915, 2.500000000000000000, -2.165063509461101710 ) ) ;
#99199 = CIRCLE ( 'NONE', #80422, 0.1000000000000002554 ) ;
#99200 = CARTESIAN_POINT ( 'NONE',  ( -9.200000000000009948, 12.50000000000000000, -4.265033745738159965 ) ) ;
#99201 = FACE_OUTER_BOUND ( 'NONE', #4948, .T. ) ;
#99202 = CARTESIAN_POINT ( 'NONE',  ( -1.900000000000034550, 12.50000000000000000, 4.676537180435972552 ) ) ;
#99203 = EDGE_CURVE ( 'NONE', #79720, #9937, #95726, .T. ) ;
#99204 = DIRECTION ( 'NONE',  ( -0.000000000000000000, -1.000000000000000000, -0.000000000000000000 ) ) ;
#99205 = VERTEX_POINT ( 'NONE', #55771 ) ;
#99206 = ORIENTED_EDGE ( 'NONE', *, *, #121214, .F. ) ;
#99207 = CONICAL_SURFACE ( 'NONE', #42799, 0.1000000000000002554, 0.003490658503988666988 ) ;
#99208 = AXIS2_PLACEMENT_3D ( 'NONE', #90443, #72758, #51836 ) ;
#99209 = EDGE_LOOP ( 'NONE', ( #49922, #104626 ) ) ;
#99210 = ORIENTED_EDGE ( 'NONE', *, *, #5543, .T. ) ;
#99211 = CARTESIAN_POINT ( 'NONE',  ( -9.350000000000008527, 12.50000000000000000, -6.841600689897072485 ) ) ;
#99213 = AXIS2_PLACEMENT_3D ( 'NONE', #42045, #90474, #11280 ) ;
#99212 = DIRECTION ( 'NONE',  ( 0.000000000000000000, 0.000000000000000000, -1.000000000000000000 ) ) ;
#99214 = ORIENTED_EDGE ( 'NONE', *, *, #29805, .T. ) ;
#99215 = DIRECTION ( 'NONE',  ( -0.000000000000000000, -1.000000000000000000, -0.000000000000000000 ) ) ;
#99216 = AXIS2_PLACEMENT_3D ( 'NONE', #127972, #78896, #86755 ) ;
#99217 = DIRECTION ( 'NONE',  ( 0.000000000000000000, 0.000000000000000000, -1.000000000000000000 ) ) ;
#99218 = DIRECTION ( 'NONE',  ( 0.000000000000000000, 0.000000000000000000, 1.000000000000000000 ) ) ;
#99219 = CARTESIAN_POINT ( 'NONE',  ( 184.0260416670080588, -6.551208109652273848, -3.782341765625003571 ) ) ;
#99220 = CARTESIAN_POINT ( 'NONE',  ( -3.950000000000028155, 2.500000000000000000, -6.841600689897077814 ) ) ;
#99221 = DIRECTION ( 'NONE',  ( 0.000000000000000000, -0.000000000000000000, 1.000000000000000000 ) ) ;
#99222 = CARTESIAN_POINT ( 'NONE',  ( 5.649999999999932854, 12.50000000000000000, 2.511473670974873507 ) ) ;
#99223 = ORIENTED_EDGE ( 'NONE', *, *, #89206, .T. ) ;
#99224 = CARTESIAN_POINT ( 'NONE',  ( -5.800000000000022027, 2.500000000000000000, -4.330127018922201643 ) ) ;
#99225 = ORIENTED_EDGE ( 'NONE', *, *, #93730, .F. ) ;
#99226 = EDGE_CURVE ( 'NONE', #38808, #76595, #28830, .T. ) ;
#99228 = ORIENTED_EDGE ( 'NONE', *, *, #77240, .T. ) ;
#99227 = AXIS2_PLACEMENT_3D ( 'NONE', #86356, #7802, #127588 ) ;
#99229 = DIRECTION ( 'NONE',  ( -0.000000000000000000, 1.000000000000000000, -0.000000000000000000 ) ) ;
#99230 = CONICAL_SURFACE ( 'NONE', #65756, 0.1000000000000002554, 0.003490658503988666988 ) ;
#99231 = CONICAL_SURFACE ( 'NONE', #36545, 0.1000000000000002554, 0.003490658503988666988 ) ;
#99232 = DIRECTION ( 'NONE',  ( 0.000000000000000000, 1.000000000000000000, 0.000000000000000000 ) ) ;
#99233 = CONICAL_SURFACE ( 'NONE', #72044, 0.09999999999999982514, 0.003490658503988666988 ) ;
#99234 = DIRECTION ( 'NONE',  ( 0.000000000000000000, 0.000000000000000000, 1.000000000000000000 ) ) ;
#99235 = ORIENTED_EDGE ( 'NONE', *, *, #82832, .F. ) ;
#99237 = EDGE_CURVE ( 'NONE', #113231, #2251, #83117, .T. ) ;
#99236 = ORIENTED_EDGE ( 'NONE', *, *, #33728, .T. ) ;
#99238 = DIRECTION ( 'NONE',  ( 0.000000000000000000, 0.000000000000000000, -1.000000000000000000 ) ) ;
#99239 = CONICAL_SURFACE ( 'NONE', #84559, 0.09999999999999982514, 0.003490658503988666988 ) ;
#99240 = AXIS2_PLACEMENT_3D ( 'NONE', #15630, #126899, #73926 ) ;
#99241 = CIRCLE ( 'NONE', #67922, 0.09999999999999982514 ) ;
#99242 = LINE ( 'NONE', #69766, #1433 ) ;
#99243 = CARTESIAN_POINT ( 'NONE',  ( 12.93920187831609603, -1.500000000000000000, -9.999999999999998224 ) ) ;
#99244 = VERTEX_POINT ( 'NONE', #106168 ) ;
#99245 = EDGE_CURVE ( 'NONE', #33099, #96862, #55991, .T. ) ;
#99246 = AXIS2_PLACEMENT_3D ( 'NONE', #110539, #41825, #40540 ) ;
#99247 = DIRECTION ( 'NONE',  ( 0.000000000000000000, -0.9999939076577903929, 0.003490651415223739937 ) ) ;
#99248 = EDGE_CURVE ( 'NONE', #38209, #58662, #16269, .T. ) ;
#99249 = ADVANCED_FACE ( 'NONE', ( #15837 ), #104127, .T. ) ;
#99250 = ORIENTED_EDGE ( 'NONE', *, *, #114857, .T. ) ;
#99251 = DIRECTION ( 'NONE',  ( 0.000000000000000000, 0.000000000000000000, -1.000000000000000000 ) ) ;
#99252 = AXIS2_PLACEMENT_3D ( 'NONE', #41008, #80910, #21330 ) ;
#99253 = CIRCLE ( 'NONE', #17656, 0.06509327318403745899 ) ;
#99254 = EDGE_LOOP ( 'NONE', ( #76995, #49333, #117212, #33996 ) ) ;
#99255 = CARTESIAN_POINT ( 'NONE',  ( 186.2916666666666288, 4.445597072760091528, -7.700000000000049916 ) ) ;
#99256 = ADVANCED_FACE ( 'NONE', ( #95707 ), #129284, .T. ) ;
#99257 = CARTESIAN_POINT ( 'NONE',  ( -11.84999999999999609, 12.50000000000000000, 6.148780366869520897 ) ) ;
#99258 = DIRECTION ( 'NONE',  ( -0.000000000000000000, -1.000000000000000000, -0.000000000000000000 ) ) ;
#99259 = CIRCLE ( 'NONE', #101306, 0.09999999999999982514 ) ;
#99260 = DIRECTION ( 'NONE',  ( 0.000000000000000000, 0.000000000000000000, -1.000000000000000000 ) ) ;
#99261 = ORIENTED_EDGE ( 'NONE', *, *, #6555, .T. ) ;
#99262 = EDGE_CURVE ( 'NONE', #48101, #61538, #5897, .T. ) ;
#99263 = CARTESIAN_POINT ( 'NONE',  ( -13.09999999999999254, 2.500000000000000000, -4.083716857408424161 ) ) ;
#99264 = EDGE_CURVE ( 'NONE', #113868, #8077, #56409, .T. ) ;
#99265 = ORIENTED_EDGE ( 'NONE', *, *, #65847, .T. ) ;
#99266 = ORIENTED_EDGE ( 'NONE', *, *, #23169, .T. ) ;
#99267 = CARTESIAN_POINT ( 'NONE',  ( 1.249999999999952482, 2.500000000000000000, -5.702370205355749455 ) ) ;
#99268 = FACE_OUTER_BOUND ( 'NONE', #52819, .T. ) ;
#99269 = LINE ( 'NONE', #10846, #67856 ) ;
#99270 = DIRECTION ( 'NONE',  ( 0.000000000000000000, 0.000000000000000000, 1.000000000000000000 ) ) ;
#99271 = CONICAL_SURFACE ( 'NONE', #51153, 0.1000000000000002554, 0.003490658503988666988 ) ;
#99272 = DIRECTION ( 'NONE',  ( -0.000000000000000000, -1.000000000000000000, -0.000000000000000000 ) ) ;
#99273 = CARTESIAN_POINT ( 'NONE',  ( 7.699999999999923794, 12.50000000000000000, 4.676537180435972552 ) ) ;
#99274 = CARTESIAN_POINT ( 'NONE',  ( 5.849999999999933920, 2.500000000000000000, -2.265063509461101798 ) ) ;
#99275 = LINE ( 'NONE', #9596, #122333 ) ;
#99276 = LINE ( 'NONE', #60011, #4554 ) ;
#99277 = CIRCLE ( 'NONE', #9390, 0.06509327318403745899 ) ;
#99278 = VERTEX_POINT ( 'NONE', #104856 ) ;
#99279 = DIRECTION ( 'NONE',  ( 0.000000000000000000, 0.000000000000000000, 1.000000000000000000 ) ) ;
#99280 = DIRECTION ( 'NONE',  ( -4.274815082592931898E-19, -0.9999939076577903929, -0.003490651415223739937 ) ) ;
#99281 = DIRECTION ( 'NONE',  ( 0.000000000000000000, 0.000000000000000000, 1.000000000000000000 ) ) ;
#99282 = DIRECTION ( 'NONE',  ( 0.000000000000000000, 0.000000000000000000, -1.000000000000000000 ) ) ;
#99283 = DIRECTION ( 'NONE',  ( -0.000000000000000000, 1.000000000000000000, -0.000000000000000000 ) ) ;
#99284 = VERTEX_POINT ( 'NONE', #25029 ) ;
#99285 = CARTESIAN_POINT ( 'NONE',  ( -5.000000000000022204, 2.500000000000000000, -0.6928203230275541413 ) ) ;
#99286 = CIRCLE ( 'NONE', #51173, 0.06509327318403745899 ) ;
#99287 = EDGE_CURVE ( 'NONE', #77185, #89102, #72833, .T. ) ;
#99288 = CONICAL_SURFACE ( 'NONE', #109751, 0.09999999999999982514, 0.003490658503988666988 ) ;
#99289 = CARTESIAN_POINT ( 'NONE',  ( -9.350000000000008527, 12.50000000000000000, -6.148780366869520897 ) ) ;
#99291 = VERTEX_POINT ( 'NONE', #36140 ) ;
#99290 = FACE_OUTER_BOUND ( 'NONE', #6024, .T. ) ;
#99292 = EDGE_LOOP ( 'NONE', ( #53313, #108167 ) ) ;
#99293 = CARTESIAN_POINT ( 'NONE',  ( 9.149999999999915090, 12.50000000000000000, -2.165063509461101710 ) ) ;
#99294 = ADVANCED_FACE ( 'NONE', ( #6012 ), #114573, .T. ) ;
#99295 = CIRCLE ( 'NONE', #49136, 0.09999999999999982514 ) ;
#99296 = AXIS2_PLACEMENT_3D ( 'NONE', #46074, #125274, #124630 ) ;
#99297 = EDGE_LOOP ( 'NONE', ( #52572, #84663, #37563, #105134 ) ) ;
#99298 = EDGE_LOOP ( 'NONE', ( #108272, #80548 ) ) ;
#99299 = ORIENTED_EDGE ( 'NONE', *, *, #117361, .F. ) ;
#99300 = DIRECTION ( 'NONE',  ( 0.000000000000000000, 1.000000000000000000, 0.000000000000000000 ) ) ;
#99301 = CARTESIAN_POINT ( 'NONE',  ( 19.40342015654704610, 2.551666867760210788, -4.359384978532800936 ) ) ;
#99302 = LINE ( 'NONE', #20094, #102653 ) ;
#99303 = DIRECTION ( 'NONE',  ( 0.000000000000000000, 0.000000000000000000, -1.000000000000000000 ) ) ;
#99304 = ORIENTED_EDGE ( 'NONE', *, *, #26082, .T. ) ;
#99305 = CARTESIAN_POINT ( 'NONE',  ( 4.399999999999937295, 2.500000000000000000, 4.676537180435972552 ) ) ;
#99306 = EDGE_LOOP ( 'NONE', ( #93600, #117825, #25354, #88036 ) ) ;
#99307 = CARTESIAN_POINT ( 'NONE',  ( 3.549999999999941203, 12.50000000000000000, 6.148780366869520897 ) ) ;
#99308 = DIRECTION ( 'NONE',  ( 0.000000000000000000, 0.000000000000000000, 1.000000000000000000 ) ) ;
#99309 = LINE ( 'NONE', #37805, #63121 ) ;
#99310 = CARTESIAN_POINT ( 'NONE',  ( -5.850000000000018296, 2.500000000000000000, 2.857883832488649301 ) ) ;
#99311 = AXIS2_PLACEMENT_3D ( 'NONE', #60299, #51112, #121121 ) ;
#99312 = EDGE_LOOP ( 'NONE', ( #103606, #59642 ) ) ;
#99313 = AXIS2_PLACEMENT_3D ( 'NONE', #120764, #80204, #21264 ) ;
#99314 = ORIENTED_EDGE ( 'NONE', *, *, #16335, .T. ) ;
#99315 = ORIENTED_EDGE ( 'NONE', *, *, #107139, .F. ) ;
#99316 = AXIS2_PLACEMENT_3D ( 'NONE', #17960, #19235, #48083 ) ;
#99317 = VERTEX_POINT ( 'NONE', #58370 ) ;
#99318 = ORIENTED_EDGE ( 'NONE', *, *, #120762, .F. ) ;
#99319 = CARTESIAN_POINT ( 'NONE',  ( -0.2000000000000408673, 2.500000000000000000, -3.883716857408426648 ) ) ;
#99320 = CARTESIAN_POINT ( 'NONE',  ( -5.850000000000022737, 2.500000000000000000, -6.495190528383302464 ) ) ;
#99321 = VECTOR ( 'NONE', #85201, 1000.000000000000000 ) ;
#99322 = DIRECTION ( 'NONE',  ( -0.000000000000000000, 1.000000000000000000, -0.000000000000000000 ) ) ;
#99323 = FACE_BOUND ( 'NONE', #126902, .T. ) ;
#99324 = CARTESIAN_POINT ( 'NONE',  ( -10.85000000000000142, 2.500000000000000000, 6.395190528383296602 ) ) ;
#99325 = DIRECTION ( 'NONE',  ( 0.000000000000000000, -0.9999939076577903929, 0.003490651415223739937 ) ) ;
#99326 = PLANE ( 'NONE',  #30176 ) ;
#99327 = DIRECTION ( 'NONE',  ( -0.000000000000000000, -1.000000000000000000, -0.000000000000000000 ) ) ;
#99328 = AXIS2_PLACEMENT_3D ( 'NONE', #97308, #114992, #104547 ) ;
#99329 = CIRCLE ( 'NONE', #42824, 0.09999999999999982514 ) ;
#99330 = VECTOR ( 'NONE', #67019, 1000.000000000000000 ) ;
#99331 = DIRECTION ( 'NONE',  ( 0.000000000000000000, 0.000000000000000000, 1.000000000000000000 ) ) ;
#99332 = AXIS2_PLACEMENT_3D ( 'NONE', #80293, #79016, #31202 ) ;
#99333 = DIRECTION ( 'NONE',  ( 0.000000000000000000, 1.000000000000000000, 0.000000000000000000 ) ) ;
#99334 = DIRECTION ( 'NONE',  ( -0.000000000000000000, -1.000000000000000000, -0.000000000000000000 ) ) ;
#99335 = CIRCLE ( 'NONE', #93077, 0.06509327318403745899 ) ;
#99337 = EDGE_CURVE ( 'NONE', #11600, #97446, #87382, .T. ) ;
#99336 = VECTOR ( 'NONE', #106580, 1000.000000000000000 ) ;
#99338 = CARTESIAN_POINT ( 'NONE',  ( -10.40000000000000213, 2.500000000000000000, -4.230127018922197557 ) ) ;
#99339 = ORIENTED_EDGE ( 'NONE', *, *, #128407, .F. ) ;
#99340 = ORIENTED_EDGE ( 'NONE', *, *, #70021, .F. ) ;
#99341 = ORIENTED_EDGE ( 'NONE', *, *, #98017, .F. ) ;
#99342 = ORIENTED_EDGE ( 'NONE', *, *, #55661, .T. ) ;
#99343 = CIRCLE ( 'NONE', #42932, 0.06509327318403745899 ) ;
#99344 = CARTESIAN_POINT ( 'NONE',  ( -4.400000000000025224, 12.50000000000000000, 3.983716857408420076 ) ) ;
#99345 = EDGE_CURVE ( 'NONE', #59160, #28644, #47701, .T. ) ;
#99346 = DIRECTION ( 'NONE',  ( 0.000000000000000000, 0.000000000000000000, 1.000000000000000000 ) ) ;
#99347 = FACE_BOUND ( 'NONE', #73757, .T. ) ;
#99348 = EDGE_CURVE ( 'NONE', #93851, #37658, #116617, .T. ) ;
#99349 = FACE_OUTER_BOUND ( 'NONE', #101329, .T. ) ;
#99350 = EDGE_CURVE ( 'NONE', #121936, #64779, #62378, .T. ) ;
#99351 = EDGE_CURVE ( 'NONE', #126997, #79185, #3781, .T. ) ;
#99352 = ORIENTED_EDGE ( 'NONE', *, *, #72588, .F. ) ;
#99353 = CARTESIAN_POINT ( 'NONE',  ( -0.8500000000000390576, 2.500000000000000000, -6.395190528383301931 ) ) ;
#99354 = CARTESIAN_POINT ( 'NONE',  ( 187.5000000000000000, 1.500000000000000000, 6.000000000000000000 ) ) ;
#99355 = DIRECTION ( 'NONE',  ( 0.000000000000000000, 0.000000000000000000, -1.000000000000000000 ) ) ;
#99356 = ADVANCED_FACE ( 'NONE', ( #120979 ), #127730, .T. ) ;
#99357 = CARTESIAN_POINT ( 'NONE',  ( 11.69999999999990870, 2.500000000000000000, 4.330127018922196314 ) ) ;
#99359 = EDGE_LOOP ( 'NONE', ( #63371, #92742, #57307, #103038 ) ) ;
#99358 = VECTOR ( 'NONE', #90473, 1000.000000000000000 ) ;
#99360 = CARTESIAN_POINT ( 'NONE',  ( -10.00000000000000355, 2.500000000000000000, -0.6928203230275541413 ) ) ;
#99361 = EDGE_LOOP ( 'NONE', ( #119292, #56929, #28110, #125169 ) ) ;
#99362 = ORIENTED_EDGE ( 'NONE', *, *, #11478, .F. ) ;
#99363 = CARTESIAN_POINT ( 'NONE',  ( 10.44999999999991402, 12.50000000000000000, -2.099970236277064473 ) ) ;
#99364 = CARTESIAN_POINT ( 'NONE',  ( -6.050000000000017586, 2.500000000000000000, 6.248780366869520542 ) ) ;
#99365 = AXIS2_PLACEMENT_3D ( 'NONE', #15790, #95016, #43988 ) ;
#99366 = ORIENTED_EDGE ( 'NONE', *, *, #2360, .F. ) ;
#99367 = CIRCLE ( 'NONE', #3224, 0.06509327318403745899 ) ;
#99368 = AXIS2_PLACEMENT_3D ( 'NONE', #57316, #127353, #87400 ) ;
#99369 = LINE ( 'NONE', #69234, #78212 ) ;
#99370 = CARTESIAN_POINT ( 'NONE',  ( 8.349999999999923261, 2.500000000000000000, -7.288010851410854585 ) ) ;
#99371 = ORIENTED_EDGE ( 'NONE', *, *, #19046, .F. ) ;
#99372 = DIRECTION ( 'NONE',  ( 0.000000000000000000, -0.000000000000000000, 1.000000000000000000 ) ) ;
#99373 = ORIENTED_EDGE ( 'NONE', *, *, #100518, .T. ) ;
#99374 = CARTESIAN_POINT ( 'NONE',  ( 11.84999999999990727, 12.50000000000000000, 6.841600689897072485 ) ) ;
#99375 = EDGE_LOOP ( 'NONE', ( #14035, #59386 ) ) ;
#99376 = CARTESIAN_POINT ( 'NONE',  ( 7.949999999999922018, 12.50000000000000000, -2.165063509461101710 ) ) ;
#99377 = FACE_BOUND ( 'NONE', #63596, .T. ) ;
#99378 = CIRCLE ( 'NONE', #51278, 0.1000000000000000472 ) ;
#99379 = ORIENTED_EDGE ( 'NONE', *, *, #82059, .F. ) ;
#99381 = DIRECTION ( 'NONE',  ( 1.000000000000000000, 0.000000000000000000, 0.000000000000000000 ) ) ;
#99380 = AXIS2_PLACEMENT_3D ( 'NONE', #54114, #34495, #114320 ) ;
#99382 = ORIENTED_EDGE ( 'NONE', *, *, #86413, .F. ) ;
#99383 = DIRECTION ( 'NONE',  ( 1.000000000000000000, 0.000000000000000000, -1.445602896647339656E-16 ) ) ;
#99384 = CARTESIAN_POINT ( 'NONE',  ( -8.100000000000013856, 12.50000000000000000, 0.2813168883297362810 ) ) ;
#99385 = DIRECTION ( 'NONE',  ( 0.000000000000000000, -0.000000000000000000, 1.000000000000000000 ) ) ;
#99386 = CARTESIAN_POINT ( 'NONE',  ( 10.39999999999991154, 12.50000000000000000, 3.702399969078682407 ) ) ;
#99387 = CARTESIAN_POINT ( 'NONE',  ( -12.69999999999999396, 12.50000000000000000, 0.2813168883297402778 ) ) ;
#99388 = VERTEX_POINT ( 'NONE', #87155 ) ;
#99389 = VERTEX_POINT ( 'NONE', #76704 ) ;
#99390 = ORIENTED_EDGE ( 'NONE', *, *, #99174, .T. ) ;
#99391 = DIRECTION ( 'NONE',  ( 0.000000000000000000, 0.000000000000000000, 1.000000000000000000 ) ) ;
#99392 = VECTOR ( 'NONE', #9366, 1000.000000000000000 ) ;
#99393 = DIRECTION ( 'NONE',  ( 0.000000000000000000, 0.000000000000000000, -1.000000000000000000 ) ) ;
#99395 = EDGE_CURVE ( 'NONE', #15286, #31758, #1709, .T. ) ;
#99394 = DIRECTION ( 'NONE',  ( -0.000000000000000000, 1.000000000000000000, -0.000000000000000000 ) ) ;
#99397 = VERTEX_POINT ( 'NONE', #106791 ) ;
#99396 = ORIENTED_EDGE ( 'NONE', *, *, #5784, .T. ) ;
#99398 = VERTEX_POINT ( 'NONE', #71225 ) ;
#99399 = EDGE_CURVE ( 'NONE', #62733, #30373, #60237, .T. ) ;
#99400 = DIRECTION ( 'NONE',  ( 0.000000000000000000, -0.000000000000000000, 1.000000000000000000 ) ) ;
#99401 = EDGE_CURVE ( 'NONE', #64551, #23628, #20517, .T. ) ;
#99402 = DIRECTION ( 'NONE',  ( 0.000000000000000000, 0.000000000000000000, -1.000000000000000000 ) ) ;
#99403 = CONTEXT_DEPENDENT_SHAPE_REPRESENTATION ( #111590, #124580 ) ;
#99404 = DIRECTION ( 'NONE',  ( 0.000000000000000000, 0.000000000000000000, 1.000000000000000000 ) ) ;
#99405 = CARTESIAN_POINT ( 'NONE',  ( -6.900000000000019007, 2.500000000000000000, -4.776537180435978414 ) ) ;
#99406 = CIRCLE ( 'NONE', #53431, 0.09999999999999982514 ) ;
#99407 = DIRECTION ( 'NONE',  ( 0.000000000000000000, 1.000000000000000000, 0.000000000000000000 ) ) ;
#99409 = DIRECTION ( 'NONE',  ( -4.274815082592931898E-19, -0.9999939076577903929, -0.003490651415223739937 ) ) ;
#99408 = B_SPLINE_CURVE_WITH_KNOTS ( 'NONE', 3,
 ( #59298, #88735, #96599, #118196, #87434, #98531, #18697, #9536, #129333, #49477, #89386, #76983, #29820, #108370, #116885, #128016, #39663, #109672, #27228, #79567 ),
 .UNSPECIFIED., .F., .F.,
 ( 4, 2, 2, 2, 2, 2, 2, 2, 2, 4 ),
 ( 0.000000000000000000, 0.003515823931524271733, 0.005273735897286407383, 0.007031647863048543466, 0.008789559828810680417, 0.01054747179457281477, 0.01142642777745388021, 0.01230538376033494564, 0.01318433974321600935, 0.01406329572609707479 ),
 .UNSPECIFIED. ) ;
#99410 = LINE ( 'NONE', #20842, #61298 ) ;
#99411 = EDGE_CURVE ( 'NONE', #113868, #26724, #125048, .T. ) ;
#99412 = EDGE_CURVE ( 'NONE', #10651, #76320, #43507, .T. ) ;
#99413 = CONICAL_SURFACE ( 'NONE', #42992, 0.1000000000000002554, 0.003490658503988666988 ) ;
#99414 = CARTESIAN_POINT ( 'NONE',  ( 2.899999999999946620, 2.500000000000000000, -4.922947341949753586 ) ) ;
#99415 = EDGE_CURVE ( 'NONE', #49108, #127376, #95808, .T. ) ;
#99416 = ORIENTED_EDGE ( 'NONE', *, *, #112188, .T. ) ;
#99418 = EDGE_LOOP ( 'NONE', ( #4686, #93673, #116864, #20188 ) ) ;
#99417 = ADVANCED_FACE ( 'NONE', ( #120341 ), #14225, .T. ) ;
#99419 = DIRECTION ( 'NONE',  ( 0.000000000000000000, 0.000000000000000000, -1.000000000000000000 ) ) ;
#99420 = ADVANCED_FACE ( 'NONE', ( #1201 ), #106274, .T. ) ;
#99421 = VECTOR ( 'NONE', #98373, 1000.000000000000000 ) ;
#99422 = AXIS2_PLACEMENT_3D ( 'NONE', #66257, #68840, #127763 ) ;
#99423 = DIRECTION ( 'NONE',  ( 0.000000000000000000, 0.000000000000000000, 1.000000000000000000 ) ) ;
#99424 = ORIENTED_EDGE ( 'NONE', *, *, #24198, .T. ) ;
#99425 = ORIENTED_EDGE ( 'NONE', *, *, #36207, .T. ) ;
#99426 = CARTESIAN_POINT ( 'NONE',  ( 185.4427083336747160, -6.551208109652278289, 3.782341765624995134 ) ) ;
#99427 = DIRECTION ( 'NONE',  ( 0.000000000000000000, 0.000000000000000000, 1.000000000000000000 ) ) ;
#99428 = CARTESIAN_POINT ( 'NONE',  ( 2.500000000000002220, 2.500000000000000000, -9.261799387799149130 ) ) ;
#99429 = ADVANCED_FACE ( 'NONE', ( #60774 ), #112549, .T. ) ;
#99430 = AXIS2_PLACEMENT_3D ( 'NONE', #107453, #6632, #58373 ) ;
#99431 = DIRECTION ( 'NONE',  ( -4.274815082592931898E-19, -0.9999939076577903929, -0.003490651415223739937 ) ) ;
#99432 = DIRECTION ( 'NONE',  ( -0.000000000000000000, -1.000000000000000000, -0.000000000000000000 ) ) ;
#99433 = DIRECTION ( 'NONE',  ( 0.000000000000000000, -0.000000000000000000, 1.000000000000000000 ) ) ;
#99434 = CARTESIAN_POINT ( 'NONE',  ( -12.49999999999999467, 12.50000000000000000, -3.637306695894647390 ) ) ;
#99435 = CONICAL_SURFACE ( 'NONE', #84746, 0.1000000000000000056, 0.003490658503988666988 ) ;
#99436 = DIRECTION ( 'NONE',  ( 0.000000000000000000, 0.000000000000000000, 1.000000000000000000 ) ) ;
#99437 = AXIS2_PLACEMENT_3D ( 'NONE', #40854, #21179, #29093 ) ;
#99438 = AXIS2_PLACEMENT_3D ( 'NONE', #77456, #26432, #27701 ) ;
#99439 = ORIENTED_EDGE ( 'NONE', *, *, #86693, .T. ) ;
#99440 = CONICAL_SURFACE ( 'NONE', #59737, 0.1000000000000000472, 0.003490658503988666988 ) ;
#99441 = ORIENTED_EDGE ( 'NONE', *, *, #122929, .T. ) ;
#99442 = AXIS2_PLACEMENT_3D ( 'NONE', #65450, #123099, #64166 ) ;
#99443 = ORIENTED_EDGE ( 'NONE', *, *, #39975, .T. ) ;
#99444 = VERTEX_POINT ( 'NONE', #50965 ) ;
#99445 = CARTESIAN_POINT ( 'NONE',  ( 14.34999999999989306, 2.500000000000000000, -1.818653347947326138 ) ) ;
#99446 = LINE ( 'NONE', #47760, #1933 ) ;
#99447 = VERTEX_POINT ( 'NONE', #41150 ) ;
#99448 = LINE ( 'NONE', #573, #44485 ) ;
#99449 = DIRECTION ( 'NONE',  ( -0.000000000000000000, -1.000000000000000000, -0.000000000000000000 ) ) ;
#99450 = DIRECTION ( 'NONE',  ( -0.000000000000000000, 1.000000000000000000, -0.000000000000000000 ) ) ;
#99452 = ORIENTED_EDGE ( 'NONE', *, *, #22996, .F. ) ;
#99451 = CARTESIAN_POINT ( 'NONE',  ( 6.899999999999928413, 12.50000000000000000, -4.741630453620015118 ) ) ;
#99453 = DIRECTION ( 'NONE',  ( -4.274815082592931898E-19, -0.9999939076577903929, -0.003490651415223739937 ) ) ;
#99454 = VECTOR ( 'NONE', #106108, 1000.000000000000000 ) ;
#99455 = CARTESIAN_POINT ( 'NONE',  ( 6.249999999999930722, 2.500000000000000000, 1.572243186433545548 ) ) ;
#99456 = ORIENTED_EDGE ( 'NONE', *, *, #2414, .F. ) ;
#99457 = EDGE_CURVE ( 'NONE', #88690, #37178, #37241, .T. ) ;
#99458 = ORIENTED_EDGE ( 'NONE', *, *, #14249, .T. ) ;
#99459 = EDGE_LOOP ( 'NONE', ( #36827, #38171 ) ) ;
#99460 = ORIENTED_EDGE ( 'NONE', *, *, #37170, .F. ) ;
#99461 = FACE_OUTER_BOUND ( 'NONE', #34613, .T. ) ;
#99462 = AXIS2_PLACEMENT_3D ( 'NONE', #70060, #11118, #9848 ) ;
#99463 = AXIS2_PLACEMENT_3D ( 'NONE', #45413, #85321, #40098 ) ;
#99464 = DIRECTION ( 'NONE',  ( 0.000000000000000000, 0.000000000000000000, -1.000000000000000000 ) ) ;
#99465 = DIRECTION ( 'NONE',  ( 0.000000000000000000, 1.000000000000000000, 0.000000000000000000 ) ) ;
#99466 = CIRCLE ( 'NONE', #80678, 0.1000000000000002554 ) ;
#99467 = ORIENTED_EDGE ( 'NONE', *, *, #69369, .T. ) ;
#99468 = DIRECTION ( 'NONE',  ( 0.000000000000000000, -0.9999939076577903929, 0.003490651415223739937 ) ) ;
#99469 = CARTESIAN_POINT ( 'NONE',  ( -6.250000000000017764, 2.500000000000000000, 2.957883832488649389 ) ) ;
#99470 = ADVANCED_FACE ( 'NONE', ( #18426 ), #85344, .T. ) ;
#99471 = DIRECTION ( 'NONE',  ( 0.000000000000000000, 0.000000000000000000, 1.000000000000000000 ) ) ;
#99472 = FACE_OUTER_BOUND ( 'NONE', #60371, .T. ) ;
#99473 = CIRCLE ( 'NONE', #38857, 0.06509327318403745899 ) ;
#99474 = ORIENTED_EDGE ( 'NONE', *, *, #101444, .T. ) ;
#99475 = DIRECTION ( 'NONE',  ( 0.000000000000000000, 0.000000000000000000, 1.000000000000000000 ) ) ;
#99477 = CONICAL_SURFACE ( 'NONE', #89002, 0.09999999999999999167, 0.003490658503988666988 ) ;
#99476 = CIRCLE ( 'NONE', #91151, 0.06509327318403745899 ) ;
#99478 = ORIENTED_EDGE ( 'NONE', *, *, #93037, .T. ) ;
#99479 = ORIENTED_EDGE ( 'NONE', *, *, #91612, .F. ) ;
#99480 = DIRECTION ( 'NONE',  ( -0.000000000000000000, 1.000000000000000000, -0.000000000000000000 ) ) ;
#99481 = CARTESIAN_POINT ( 'NONE',  ( 5.599999999999933031, 2.500000000000000000, 0.4464101615137735513 ) ) ;
#99482 = FACE_BOUND ( 'NONE', #86419, .T. ) ;
#99483 = DIRECTION ( 'NONE',  ( 0.000000000000000000, -0.000000000000000000, 1.000000000000000000 ) ) ;
#99484 = DIRECTION ( 'NONE',  ( 0.000000000000000000, 0.000000000000000000, 1.000000000000000000 ) ) ;
#99485 = DIRECTION ( 'NONE',  ( -4.274815082592931898E-19, -0.9999939076577903929, -0.003490651415223739937 ) ) ;
#99486 = AXIS2_PLACEMENT_3D ( 'NONE', #19812, #67600, #59094 ) ;
#99487 = AXIS2_PLACEMENT_3D ( 'NONE', #64894, #104811, #55093 ) ;
#99488 = VERTEX_POINT ( 'NONE', #111813 ) ;
#99489 = CARTESIAN_POINT ( 'NONE',  ( 5.649999999999932854, 2.500000000000000000, 2.611473670974873151 ) ) ;
#99490 = DIRECTION ( 'NONE',  ( 0.000000000000000000, 1.000000000000000000, 0.000000000000000000 ) ) ;
#99491 = DIRECTION ( 'NONE',  ( -4.274815082592931898E-19, -0.9999939076577903929, -0.003490651415223739937 ) ) ;
#99492 = FACE_OUTER_BOUND ( 'NONE', #572, .T. ) ;
#99493 = ORIENTED_EDGE ( 'NONE', *, *, #114393, .T. ) ;
#99494 = DIRECTION ( 'NONE',  ( -0.000000000000000000, 1.000000000000000000, -0.000000000000000000 ) ) ;
#99495 = EDGE_CURVE ( 'NONE', #129161, #44450, #56089, .T. ) ;
#99496 = FACE_OUTER_BOUND ( 'NONE', #33369, .T. ) ;
#99497 = VERTEX_POINT ( 'NONE', #24715 ) ;
#99498 = VERTEX_POINT ( 'NONE', #121609 ) ;
#99499 = FACE_OUTER_BOUND ( 'NONE', #116767, .T. ) ;
#99500 = CARTESIAN_POINT ( 'NONE',  ( 2.499999999999983569, 12.50000000000000000, -0.06509327318403970719 ) ) ;
#99501 = FACE_BOUND ( 'NONE', #125032, .T. ) ;
#99502 = EDGE_CURVE ( 'NONE', #27192, #127834, #41459, .T. ) ;
#99503 = DIRECTION ( 'NONE',  ( 0.000000000000000000, 1.000000000000000000, 0.000000000000000000 ) ) ;
#99504 = AXIS2_PLACEMENT_3D ( 'NONE', #43363, #65556, #34838 ) ;
#99505 = DIRECTION ( 'NONE',  ( 0.000000000000000000, 1.000000000000000000, 0.000000000000000000 ) ) ;
#99506 = AXIS2_PLACEMENT_3D ( 'NONE', #22338, #92337, #79947 ) ;
#99507 = ADVANCED_FACE ( 'NONE', ( #104557 ), #82361, .T. ) ;
#99508 = EDGE_CURVE ( 'NONE', #41415, #95053, #127127, .T. ) ;
#99509 =( BOUNDED_CURVE ( )  B_SPLINE_CURVE ( 2, ( #66890, #17116, #3634, #107472, #57741, #16493, #43584 ),
 .UNSPECIFIED., .F., .F. ) 
 B_SPLINE_CURVE_WITH_KNOTS ( ( 3, 2, 2, 3 ),
 ( 0.3571428571428574283, 0.3809523809523812643, 0.4047619047619051003, 0.4285714285714289362 ),
 .UNSPECIFIED. ) 
 CURVE ( )  GEOMETRIC_REPRESENTATION_ITEM ( )  RATIONAL_B_SPLINE_CURVE ( ( 0.9999999999999984457, 0.8660254037844402619, 1.000000000000000000, 0.8660254037844387076, 1.000000000000000000, 0.8660254037844364872, 1.000000000000002220 ) ) 
 REPRESENTATION_ITEM ( '' )  );
#99510 = EDGE_LOOP ( 'NONE', ( #57106, #24944 ) ) ;
#99511 = DIRECTION ( 'NONE',  ( 0.000000000000000000, 0.000000000000000000, 1.000000000000000000 ) ) ;
#99512 = ADVANCED_FACE ( 'NONE', ( #22158 ), #58598, .T. ) ;
#99513 = EDGE_CURVE ( 'NONE', #116043, #85535, #10131, .T. ) ;
#99514 = CARTESIAN_POINT ( 'NONE',  ( 184.0416666666666572, -4.445597072760122614, 7.699999999999998401 ) ) ;
#99515 = EDGE_CURVE ( 'NONE', #54777, #66462, #94094, .T. ) ;
#99516 = EDGE_LOOP ( 'NONE', ( #17248, #70480, #82446, #91095 ) ) ;
#99517 = LINE ( 'NONE', #97560, #854 ) ;
#99518 = CARTESIAN_POINT ( 'NONE',  ( -11.44999999999999751, 2.500000000000000000, -2.611473670974873595 ) ) ;
#99519 = VECTOR ( 'NONE', #45088, 1000.000000000000000 ) ;
#99521 = EDGE_CURVE ( 'NONE', #84030, #74365, #5054, .T. ) ;
#99520 = CARTESIAN_POINT ( 'NONE',  ( 6.049999999999934097, 2.500000000000000000, -6.248780366869526759 ) ) ;
#99522 = CONICAL_SURFACE ( 'NONE', #74474, 0.1000000000000002554, 0.003490658503988666988 ) ;
#99523 = ADVANCED_FACE ( 'NONE', ( #86179 ), #26853, .T. ) ;
#99524 = ORIENTED_EDGE ( 'NONE', *, *, #41158, .T. ) ;
#99525 = CONICAL_SURFACE ( 'NONE', #97456, 0.09999999999999982514, 0.003490658503988666988 ) ;
#99526 = DIRECTION ( 'NONE',  ( 0.000000000000000000, 0.000000000000000000, 1.000000000000000000 ) ) ;
#99527 = CARTESIAN_POINT ( 'NONE',  ( -3.550000000000027356, 2.500000000000000000, 1.818653347947321475 ) ) ;
#99528 = CARTESIAN_POINT ( 'NONE',  ( -0.6000000000000383915, 12.50000000000000000, -3.983716857408426293 ) ) ;
#99529 = AXIS2_PLACEMENT_3D ( 'NONE', #17639, #57591, #48401 ) ;
#99530 = DIRECTION ( 'NONE',  ( 0.000000000000000000, 0.000000000000000000, 1.000000000000000000 ) ) ;
#99531 = ORIENTED_EDGE ( 'NONE', *, *, #120108, .F. ) ;
#99532 = ORIENTED_EDGE ( 'NONE', *, *, #2264, .F. ) ;
#99533 = DIRECTION ( 'NONE',  ( -0.000000000000000000, -1.000000000000000000, -0.000000000000000000 ) ) ;
#99534 = ORIENTED_EDGE ( 'NONE', *, *, #5049, .T. ) ;
#99535 = LINE ( 'NONE', #109990, #17940 ) ;
#99536 = FACE_OUTER_BOUND ( 'NONE', #21648, .T. ) ;
#99537 = DIRECTION ( 'NONE',  ( 0.000000000000000000, 1.000000000000000000, 0.000000000000000000 ) ) ;
#99538 = ORIENTED_EDGE ( 'NONE', *, *, #104849, .F. ) ;
#99539 = LINE ( 'NONE', #78618, #62168 ) ;
#99540 = CARTESIAN_POINT ( 'NONE',  ( 5.199999999999931788, 2.500000000000000000, 4.776537180435972196 ) ) ;
#99541 = DIRECTION ( 'NONE',  ( 0.000000000000000000, 0.000000000000000000, 1.000000000000000000 ) ) ;
#99542 = CARTESIAN_POINT ( 'NONE',  ( -0.6500000000000394351, 2.500000000000000000, 2.511473670974873507 ) ) ;
#99543 = CARTESIAN_POINT ( 'NONE',  ( 0.1999999999999636513, 12.50000000000000000, -0.2813168883297386680 ) ) ;
#99544 = CONICAL_SURFACE ( 'NONE', #57683, 0.1000000000000002554, 0.003490658503988666988 ) ;
#99545 = DIRECTION ( 'NONE',  ( 0.000000000000000000, 1.000000000000000000, 0.000000000000000000 ) ) ;
#99546 = ORIENTED_EDGE ( 'NONE', *, *, #45971, .T. ) ;
#99547 = ORIENTED_EDGE ( 'NONE', *, *, #56326, .F. ) ;
#99548 = DIRECTION ( 'NONE',  ( 0.000000000000000000, 0.000000000000000000, -1.000000000000000000 ) ) ;
#99549 = VERTEX_POINT ( 'NONE', #57394 ) ;
#99550 = CIRCLE ( 'NONE', #43128, 0.09999999999999982514 ) ;
#99551 = CARTESIAN_POINT ( 'NONE',  ( 105.4725005298439271, 6.373511028144405621, 4.325813758252836649 ) ) ;
#99553 = EDGE_LOOP ( 'NONE', ( #35045, #40404 ) ) ;
#99552 = EDGE_LOOP ( 'NONE', ( #74460, #107648, #105377, #54158 ) ) ;
#99554 = ORIENTED_EDGE ( 'NONE', *, *, #830, .T. ) ;
#99555 = CARTESIAN_POINT ( 'NONE',  ( -4.800000000000024691, 2.500000000000000000, 4.676537180435972552 ) ) ;
#99556 = ADVANCED_FACE ( 'NONE', ( #95385 ), #99931, .T. ) ;
#99557 = CIRCLE ( 'NONE', #78723, 0.06509327318403741736 ) ;
#99558 = CARTESIAN_POINT ( 'NONE',  ( -0.6000000000000383915, 12.50000000000000000, -3.918623584224389056 ) ) ;
#99559 = LINE ( 'NONE', #48514, #18425 ) ;
#99560 = CIRCLE ( 'NONE', #72371, 0.09999999999999982514 ) ;
#99561 = EDGE_CURVE ( 'NONE', #31765, #126580, #100017, .T. ) ;
#99562 = DIRECTION ( 'NONE',  ( 0.000000000000000000, 0.000000000000000000, 1.000000000000000000 ) ) ;
#99563 = CARTESIAN_POINT ( 'NONE',  ( 4.799999999999937650, 2.500000000000000000, -0.2464101615137782308 ) ) ;
#99564 = CARTESIAN_POINT ( 'NONE',  ( 11.24999999999990941, 2.500000000000000000, 7.088010851410848190 ) ) ;
#99565 = FACE_OUTER_BOUND ( 'NONE', #75044, .T. ) ;
#99566 = FACE_OUTER_BOUND ( 'NONE', #96393, .T. ) ;
#99567 = EDGE_CURVE ( 'NONE', #96734, #99163, #33229, .T. ) ;
#99568 = DIRECTION ( 'NONE',  ( -0.000000000000000000, -1.000000000000000000, -0.000000000000000000 ) ) ;
#99569 = ORIENTED_EDGE ( 'NONE', *, *, #80188, .F. ) ;
#99570 = CIRCLE ( 'NONE', #101621, 0.09999999999999982514 ) ;
#99571 = ADVANCED_FACE ( 'NONE', ( #56715 ), #43698, .T. ) ;
#99572 = ORIENTED_EDGE ( 'NONE', *, *, #32863, .F. ) ;
#99575 = ADVANCED_FACE ( 'NONE', ( #116936 ), #77029, .T. ) ;
#99574 = CONICAL_SURFACE ( 'NONE', #34832, 0.1000000000000002554, 0.003490658503988666988 ) ;
#99573 = AXIS2_PLACEMENT_3D ( 'NONE', #69260, #107910, #67978 ) ;
#99576 = CARTESIAN_POINT ( 'NONE',  ( 7.499999999999961808, 2.500000000000000000, 4.230127018922196669 ) ) ;
#99577 = ORIENTED_EDGE ( 'NONE', *, *, #93619, .T. ) ;
#99578 = ORIENTED_EDGE ( 'NONE', *, *, #38027, .T. ) ;
#99579 = CARTESIAN_POINT ( 'NONE',  ( 6.649999999999927525, 12.50000000000000000, 2.230156782645134950 ) ) ;
#99580 = EDGE_CURVE ( 'NONE', #125530, #50291, #36485, .T. ) ;
#99581 = DIRECTION ( 'NONE',  ( 0.000000000000000000, 0.000000000000000000, 1.000000000000000000 ) ) ;
#99582 = FACE_OUTER_BOUND ( 'NONE', #82626, .T. ) ;
#99583 = LINE ( 'NONE', #79298, #7456 ) ;
#99584 = CARTESIAN_POINT ( 'NONE',  ( -8.550000000000014921, 2.500000000000000000, -6.048780366869521252 ) ) ;
#99585 = ORIENTED_EDGE ( 'NONE', *, *, #65676, .T. ) ;
#99586 = VERTEX_POINT ( 'NONE', #115002 ) ;
#99587 = CARTESIAN_POINT ( 'NONE',  ( 1.699999999999951994, 2.500000000000000000, -2.276824562219559311E-15 ) ) ;
#99588 = ORIENTED_EDGE ( 'NONE', *, *, #117257, .T. ) ;
#99589 = CYLINDRICAL_SURFACE ( 'NONE', #117324, 8.699999999999999289 ) ;
#99590 = ORIENTED_EDGE ( 'NONE', *, *, #43053, .T. ) ;
#99591 = EDGE_CURVE ( 'NONE', #102898, #82416, #108415, .T. ) ;
#99592 = ORIENTED_EDGE ( 'NONE', *, *, #68965, .F. ) ;
#99593 = DIRECTION ( 'NONE',  ( 0.000000000000000000, -0.9999939076577903929, 0.003490651415223739937 ) ) ;
#99594 = DIRECTION ( 'NONE',  ( 0.000000000000000000, 0.000000000000000000, -1.000000000000000000 ) ) ;
#99595 = CIRCLE ( 'NONE', #49423, 0.1000000000000000472 ) ;
#99596 = DIRECTION ( 'NONE',  ( 0.000000000000000000, 0.000000000000000000, 1.000000000000000000 ) ) ;
#99598 = CARTESIAN_POINT ( 'NONE',  ( 10.19999999999991580, 2.500000000000000000, -0.3464101615137783474 ) ) ;
#99597 = CIRCLE ( 'NONE', #103789, 0.06509327318403745899 ) ;
#99599 = CARTESIAN_POINT ( 'NONE',  ( 87.50000000000002842, -0.7169905660283000248, 7.500000000000001776 ) ) ;
#99600 = ORIENTED_EDGE ( 'NONE', *, *, #37626, .T. ) ;
#99601 = CARTESIAN_POINT ( 'NONE',  ( 8.749999999999918288, 2.500000000000000000, 7.288010851410849256 ) ) ;
#99602 = DIRECTION ( 'NONE',  ( -0.000000000000000000, -1.000000000000000000, -0.000000000000000000 ) ) ;
#99603 = DIRECTION ( 'NONE',  ( 0.000000000000000000, 0.000000000000000000, 1.000000000000000000 ) ) ;
#99604 = DIRECTION ( 'NONE',  ( -0.000000000000000000, -1.000000000000000000, -0.000000000000000000 ) ) ;
#99606 = AXIS2_PLACEMENT_3D ( 'NONE', #44259, #43645, #114296 ) ;
#99605 = CIRCLE ( 'NONE', #62045, 0.06509327318403745899 ) ;
#99607 = CARTESIAN_POINT ( 'NONE',  ( 8.349999999999919709, 2.500000000000000000, 7.088010851410848190 ) ) ;
#99608 = ORIENTED_EDGE ( 'NONE', *, *, #111622, .F. ) ;
#99609 = ADVANCED_FACE ( 'NONE', ( #17443 ), #102165, .T. ) ;
#99610 = ORIENTED_EDGE ( 'NONE', *, *, #112050, .T. ) ;
#99611 = DIRECTION ( 'NONE',  ( 0.000000000000000000, 0.000000000000000000, 1.000000000000000000 ) ) ;
#99612 = ORIENTED_EDGE ( 'NONE', *, *, #47914, .F. ) ;
#99614 = CIRCLE ( 'NONE', #30672, 0.06509327318403745899 ) ;
#99613 = VECTOR ( 'NONE', #44532, 1000.000000000000000 ) ;
#99615 = CARTESIAN_POINT ( 'NONE',  ( 17.45053695044971676, -1.969637996572824568, 4.507340027902592361 ) ) ;
#99616 = FACE_OUTER_BOUND ( 'NONE', #30859, .T. ) ;
#99617 = AXIS2_PLACEMENT_3D ( 'NONE', #115805, #117719, #45793 ) ;
#99618 = EDGE_LOOP ( 'NONE', ( #4036, #8979 ) ) ;
#99619 = PLANE ( 'NONE',  #72412 ) ;
#99620 = CARTESIAN_POINT ( 'NONE',  ( 11.84999999999990372, 12.50000000000000000, 2.446380397790835826 ) ) ;
#99621 = ADVANCED_FACE ( 'NONE', ( #15517 ), #91699, .T. ) ;
#99622 = FACE_OUTER_BOUND ( 'NONE', #84443, .T. ) ;
#99623 = DIRECTION ( 'NONE',  ( -0.000000000000000000, -1.000000000000000000, -0.000000000000000000 ) ) ;
#99624 = FACE_OUTER_BOUND ( 'NONE', #111237, .T. ) ;
#99625 = EDGE_LOOP ( 'NONE', ( #126830, #58434 ) ) ;
#99626 = DIRECTION ( 'NONE',  ( 0.000000000000000000, 0.000000000000000000, 1.000000000000000000 ) ) ;
#99627 = DIRECTION ( 'NONE',  ( 0.000000000000000000, 1.000000000000000000, 0.000000000000000000 ) ) ;
#99628 = DIRECTION ( 'NONE',  ( -0.000000000000000000, 1.000000000000000000, -0.000000000000000000 ) ) ;
#99629 = VECTOR ( 'NONE', #85974, 1000.000000000000000 ) ;
#99630 = VERTEX_POINT ( 'NONE', #5696 ) ;
#99631 = CIRCLE ( 'NONE', #124677, 0.06509327318403745899 ) ;
#99632 = CARTESIAN_POINT ( 'NONE',  ( 0.6499999999999561684, 12.50000000000000000, 2.511473670974873507 ) ) ;
#99633 = CONICAL_SURFACE ( 'NONE', #42164, 0.1000000000000002554, 0.003490658503988666988 ) ;
#99634 = ORIENTED_EDGE ( 'NONE', *, *, #110876, .F. ) ;
#99635 = CARTESIAN_POINT ( 'NONE',  ( -7.700000000000016165, 2.500000000000000000, 0.3464101615137735735 ) ) ;
#99636 = CARTESIAN_POINT ( 'NONE',  ( 11.64999999999990443, 12.50000000000000000, -7.253104124594891289 ) ) ;
#99637 = VECTOR ( 'NONE', #128838, 1000.000000000000000 ) ;
#99638 = FACE_OUTER_BOUND ( 'NONE', #69050, .T. ) ;
#99639 = EDGE_LOOP ( 'NONE', ( #123651, #29776 ) ) ;
#99640 = DIRECTION ( 'NONE',  ( 0.000000000000000000, 1.000000000000000000, 0.000000000000000000 ) ) ;
#99641 = CIRCLE ( 'NONE', #101701, 0.06509327318403743123 ) ;
#99642 = EDGE_CURVE ( 'NONE', #99122, #34917, #96647, .T. ) ;
#99643 = DIRECTION ( 'NONE',  ( -0.000000000000000000, 1.000000000000000000, -0.000000000000000000 ) ) ;
#99644 = VERTEX_POINT ( 'NONE', #26643 ) ;
#99645 = CARTESIAN_POINT ( 'NONE',  ( 8.549999999999922551, 2.500000000000000000, 2.511473670974873507 ) ) ;
#99646 = VERTEX_POINT ( 'NONE', #66553 ) ;
#99647 = DIRECTION ( 'NONE',  ( -1.000000000000000000, 0.000000000000000000, 0.000000000000000000 ) ) ;
#99648 = EDGE_CURVE ( 'NONE', #6400, #67035, #35818, .T. ) ;
#99650 = AXIS2_PLACEMENT_3D ( 'NONE', #66669, #44464, #45121 ) ;
#99649 = CIRCLE ( 'NONE', #126838, 0.06509327318403745899 ) ;
#99651 = EDGE_LOOP ( 'NONE', ( #15500, #56404, #97707, #86083 ) ) ;
#99652 = CARTESIAN_POINT ( 'NONE',  ( -4.150000000000025224, 2.500000000000000000, 5.902370205355745192 ) ) ;
#99653 = CARTESIAN_POINT ( 'NONE',  ( 14.93814514904464197, 2.500000000000000000, -6.173787961026619087 ) ) ;
#99654 = EDGE_CURVE ( 'NONE', #46914, #92524, #31078, .T. ) ;
#99655 = EDGE_LOOP ( 'NONE', ( #111406, #27205, #96949, #31996 ) ) ;
#99656 = EDGE_CURVE ( 'NONE', #26594, #19417, #56091, .T. ) ;
#99657 = VERTEX_POINT ( 'NONE', #122052 ) ;
#99658 = EDGE_CURVE ( 'NONE', #1000, #83312, #87477, .T. ) ;
#99659 = EDGE_CURVE ( 'NONE', #27686, #6619, #123963, .T. ) ;
#99660 = DIRECTION ( 'NONE',  ( -0.000000000000000000, -1.000000000000000000, -0.000000000000000000 ) ) ;
#99661 = DIRECTION ( 'NONE',  ( 0.000000000000000000, 0.000000000000000000, 1.000000000000000000 ) ) ;
#99662 = ORIENTED_EDGE ( 'NONE', *, *, #12211, .F. ) ;
#99663 = DIRECTION ( 'NONE',  ( -4.274815082592931898E-19, -0.9999939076577903929, -0.003490651415223739937 ) ) ;
#99664 = DIRECTION ( 'NONE',  ( -0.000000000000000000, 1.000000000000000000, -0.000000000000000000 ) ) ;
#99665 = ADVANCED_FACE ( 'NONE', ( #23186 ), #42869, .T. ) ;
#99666 = FACE_OUTER_BOUND ( 'NONE', #40135, .T. ) ;
#99667 = EDGE_CURVE ( 'NONE', #3622, #20697, #102409, .T. ) ;
#99668 = CARTESIAN_POINT ( 'NONE',  ( 3.099999999999944134, 2.500000000000000000, 4.776537180435972196 ) ) ;
#99669 = CARTESIAN_POINT ( 'NONE',  ( -6.250000000000019540, 12.50000000000000000, -2.922977105672691422 ) ) ;
#99670 = CARTESIAN_POINT ( 'NONE',  ( 4.549999999999937650, 12.50000000000000000, 2.230156782645134950 ) ) ;
#99671 = CARTESIAN_POINT ( 'NONE',  ( -1.050000000000038680, 2.500000000000000000, 6.741600689897071952 ) ) ;
#99673 = ADVANCED_FACE ( 'NONE', ( #42200 ), #20595, .T. ) ;
#99672 = CIRCLE ( 'NONE', #28663, 0.06509327318403745899 ) ;
#99674 = EDGE_CURVE ( 'NONE', #67302, #98804, #104953, .T. ) ;
#99675 = EDGE_CURVE ( 'NONE', #112457, #65686, #63115, .T. ) ;
#99676 = ORIENTED_EDGE ( 'NONE', *, *, #67994, .T. ) ;
#99677 = ORIENTED_EDGE ( 'NONE', *, *, #72956, .F. ) ;
#99678 = ORIENTED_EDGE ( 'NONE', *, *, #13776, .F. ) ;
#99679 = ORIENTED_EDGE ( 'NONE', *, *, #67993, .F. ) ;
#99680 = CARTESIAN_POINT ( 'NONE',  ( -7.050000000000013145, 2.500000000000000000, 2.165063509461097713 ) ) ;
#99681 = FACE_OUTER_BOUND ( 'NONE', #52623, .T. ) ;
#99682 = DIRECTION ( 'NONE',  ( 0.000000000000000000, 0.000000000000000000, -1.000000000000000000 ) ) ;
#99683 = ORIENTED_EDGE ( 'NONE', *, *, #50647, .F. ) ;
#99684 = FACE_BOUND ( 'NONE', #91202, .T. ) ;
#99685 = ORIENTED_EDGE ( 'NONE', *, *, #15603, .F. ) ;
#99686 = ADVANCED_FACE ( 'NONE', ( #25122 ), #127217, .T. ) ;
#99687 = DIRECTION ( 'NONE',  ( 0.000000000000000000, 0.000000000000000000, 1.000000000000000000 ) ) ;
#99688 = DIRECTION ( 'NONE',  ( 0.000000000000000000, 0.000000000000000000, 1.000000000000000000 ) ) ;
#99689 = DIRECTION ( 'NONE',  ( 0.000000000000000000, 0.000000000000000000, -1.000000000000000000 ) ) ;
#99690 = VECTOR ( 'NONE', #75220, 1000.000000000000000 ) ;
#99691 = DIRECTION ( 'NONE',  ( -0.000000000000000000, -1.000000000000000000, -0.000000000000000000 ) ) ;
#99692 = CIRCLE ( 'NONE', #7717, 0.1000000000000002554 ) ;
#99693 = DIRECTION ( 'NONE',  ( 0.000000000000000000, 0.000000000000000000, -1.000000000000000000 ) ) ;
#99694 = DIRECTION ( 'NONE',  ( 0.000000000000000000, 0.000000000000000000, 1.000000000000000000 ) ) ;
#99695 = CARTESIAN_POINT ( 'NONE',  ( 0.8499999999999553468, 2.500000000000000000, 1.472243186433545459 ) ) ;
#99696 = CARTESIAN_POINT ( 'NONE',  ( -1.450000000000035039, 12.50000000000000000, -2.511473670974877948 ) ) ;
#99697 = DIRECTION ( 'NONE',  ( 0.000000000000000000, 1.000000000000000000, 0.000000000000000000 ) ) ;
#99699 = CIRCLE ( 'NONE', #3539, 0.06509327318403745899 ) ;
#99698 = VECTOR ( 'NONE', #118440, 1000.000000000000000 ) ;
#99700 = EDGE_LOOP ( 'NONE', ( #40569, #85362 ) ) ;
#99701 = VERTEX_POINT ( 'NONE', #23852 ) ;
#99702 = ORIENTED_EDGE ( 'NONE', *, *, #71387, .F. ) ;
#99703 = VERTEX_POINT ( 'NONE', #14640 ) ;
#99704 = LINE ( 'NONE', #119317, #87335 ) ;
#99705 = DIRECTION ( 'NONE',  ( -4.274815082592931898E-19, -0.9999939076577903929, -0.003490651415223739937 ) ) ;
#99707 = EDGE_LOOP ( 'NONE', ( #51238, #127526 ) ) ;
#99706 = EDGE_LOOP ( 'NONE', ( #81815, #87001, #17106, #54058 ) ) ;
#99708 = ORIENTED_EDGE ( 'NONE', *, *, #1132, .T. ) ;
#99709 = DIRECTION ( 'NONE',  ( -4.274815082592931898E-19, -0.9999939076577903929, -0.003490651415223739937 ) ) ;
#99710 = CIRCLE ( 'NONE', #80924, 0.1000000000000000472 ) ;
#99711 = AXIS2_PLACEMENT_3D ( 'NONE', #125262, #46065, #54569 ) ;
#99712 = DIRECTION ( 'NONE',  ( 0.000000000000000000, 0.000000000000000000, 1.000000000000000000 ) ) ;
#99713 = CARTESIAN_POINT ( 'NONE',  ( -1.850000000000033840, 2.500000000000000000, 1.718653347947321386 ) ) ;
#99714 = DIRECTION ( 'NONE',  ( 0.000000000000000000, 1.000000000000000000, 0.000000000000000000 ) ) ;
#99715 = DIRECTION ( 'NONE',  ( 0.000000000000000000, 0.000000000000000000, 1.000000000000000000 ) ) ;
#99716 = CARTESIAN_POINT ( 'NONE',  ( 2.500000000000001776, 2.021986658763283096, 9.892226903609811828 ) ) ;
#99717 = CARTESIAN_POINT ( 'NONE',  ( 6.449999999999931788, 2.500000000000000000, -6.148780366869526226 ) ) ;
#99718 = ORIENTED_EDGE ( 'NONE', *, *, #38361, .F. ) ;
#99719 = DIRECTION ( 'NONE',  ( 0.000000000000000000, 1.000000000000000000, 0.000000000000000000 ) ) ;
#99720 = VERTEX_POINT ( 'NONE', #55243 ) ;
#99721 = EDGE_CURVE ( 'NONE', #3084, #46462, #3864, .T. ) ;
#99722 = VERTEX_POINT ( 'NONE', #2248 ) ;
#99723 = ORIENTED_EDGE ( 'NONE', *, *, #116495, .T. ) ;
#99724 = EDGE_CURVE ( 'NONE', #69063, #86941, #16463, .T. ) ;
#99725 = DIRECTION ( 'NONE',  ( -0.000000000000000000, -1.000000000000000000, -0.000000000000000000 ) ) ;
#99726 = ORIENTED_EDGE ( 'NONE', *, *, #19611, .F. ) ;
#99727 = ORIENTED_EDGE ( 'NONE', *, *, #90389, .F. ) ;
#99728 = AXIS2_PLACEMENT_3D ( 'NONE', #11780, #51724, #91636 ) ;
#99730 = DIRECTION ( 'NONE',  ( 0.000000000000000000, 0.000000000000000000, 1.000000000000000000 ) ) ;
#99729 = AXIS2_PLACEMENT_3D ( 'NONE', #38707, #77310, #118516 ) ;
#99731 = EDGE_CURVE ( 'NONE', #72821, #32401, #51994, .T. ) ;
#99732 = DIRECTION ( 'NONE',  ( -4.274815082592931898E-19, -0.9999939076577903929, -0.003490651415223739937 ) ) ;
#99734 = AXIS2_PLACEMENT_3D ( 'NONE', #42838, #12047, #2887 ) ;
#99733 = CARTESIAN_POINT ( 'NONE',  ( 2.299999999999948752, 12.50000000000000000, -3.983716857408426293 ) ) ;
#99735 = CARTESIAN_POINT ( 'NONE',  ( 9.599999999999914380, 2.500000000000000000, 4.922947341949748257 ) ) ;
#99736 = DIRECTION ( 'NONE',  ( 0.000000000000000000, -0.9999939076577903929, 0.003490651415223739937 ) ) ;
#99737 = AXIS2_PLACEMENT_3D ( 'NONE', #44942, #22737, #103208 ) ;
#99738 = ORIENTED_EDGE ( 'NONE', *, *, #34591, .T. ) ;
#99740 = CIRCLE ( 'NONE', #39211, 0.06509327318403741736 ) ;
#99739 = DIRECTION ( 'NONE',  ( -0.000000000000000000, 1.000000000000000000, -0.000000000000000000 ) ) ;
#99741 = VERTEX_POINT ( 'NONE', #92584 ) ;
#99742 = AXIS2_PLACEMENT_3D ( 'NONE', #51169, #110706, #80626 ) ;
#99743 = LINE ( 'NONE', #78168, #4493 ) ;
#99744 = ORIENTED_EDGE ( 'NONE', *, *, #58323, .F. ) ;
#99745 = CARTESIAN_POINT ( 'NONE',  ( 112.8268375934096071, 8.601552705179036806, 1.314999179819271946 ) ) ;
#99746 = DIRECTION ( 'NONE',  ( 0.000000000000000000, 0.000000000000000000, 1.000000000000000000 ) ) ;
#99747 = ORIENTED_EDGE ( 'NONE', *, *, #5371, .F. ) ;
#99748 = FACE_OUTER_BOUND ( 'NONE', #105652, .T. ) ;
#99749 = CIRCLE ( 'NONE', #103851, 0.06509327318403745899 ) ;
#99750 = CARTESIAN_POINT ( 'NONE',  ( -11.64999999999999680, 2.500000000000000000, -2.165063509461097713 ) ) ;
#99751 = EDGE_LOOP ( 'NONE', ( #102745, #91383, #44301, #72521 ) ) ;
#99753 = VECTOR ( 'NONE', #73122, 1000.000000000000000 ) ;
#99752 = VECTOR ( 'NONE', #82169, 1000.000000000000000 ) ;
#99754 = DIRECTION ( 'NONE',  ( 0.000000000000000000, 0.000000000000000000, -1.000000000000000000 ) ) ;
#99755 = ORIENTED_EDGE ( 'NONE', *, *, #35698, .T. ) ;
#99756 = ORIENTED_EDGE ( 'NONE', *, *, #32016, .T. ) ;
#99757 = DIRECTION ( 'NONE',  ( 0.000000000000000000, 0.000000000000000000, 1.000000000000000000 ) ) ;
#99758 = DIRECTION ( 'NONE',  ( 0.000000000000000000, -0.9999939076577903929, 0.003490651415223739937 ) ) ;
#99759 = CARTESIAN_POINT ( 'NONE',  ( -15.19999999999998330, 12.50000000000000000, 0.2813168883297384459 ) ) ;
#99760 = CARTESIAN_POINT ( 'NONE',  ( -5.200000000000025935, 12.50000000000000000, -3.983716857408426293 ) ) ;
#99761 = DIRECTION ( 'NONE',  ( 0.000000000000000000, 0.000000000000000000, 1.000000000000000000 ) ) ;
#99762 = VERTEX_POINT ( 'NONE', #103036 ) ;
#99763 = CARTESIAN_POINT ( 'NONE',  ( -1.250000000000037526, 2.500000000000000000, -1.472243186433550122 ) ) ;
#99764 = CIRCLE ( 'NONE', #97605, 0.09999999999999982514 ) ;
#99765 = ORIENTED_EDGE ( 'NONE', *, *, #93907, .T. ) ;
#99766 = DIRECTION ( 'NONE',  ( -0.000000000000000000, 1.000000000000000000, -0.000000000000000000 ) ) ;
#99767 = DIRECTION ( 'NONE',  ( 0.000000000000000000, 0.000000000000000000, 1.000000000000000000 ) ) ;
#99768 = EDGE_CURVE ( 'NONE', #23165, #55407, #24801, .T. ) ;
#99769 = CARTESIAN_POINT ( 'NONE',  ( 186.9635416670080303, -4.367472073101519747, 7.564683531249999149 ) ) ;
#99770 = DIRECTION ( 'NONE',  ( 0.000000000000000000, 1.000000000000000000, 0.000000000000000000 ) ) ;
#99771 = DIRECTION ( 'NONE',  ( 0.000000000000000000, -0.000000000000000000, 1.000000000000000000 ) ) ;
#99772 = EDGE_CURVE ( 'NONE', #40007, #14402, #85432, .T. ) ;
#99773 = CARTESIAN_POINT ( 'NONE',  ( -8.750000000000008882, 2.500000000000000000, -2.857883832488653741 ) ) ;
#99774 = CYLINDRICAL_SURFACE ( 'NONE', #35042, 2.249999999999996891 ) ;
#99775 = ORIENTED_EDGE ( 'NONE', *, *, #29746, .T. ) ;
#99776 = FACE_OUTER_BOUND ( 'NONE', #94374, .T. ) ;
#99777 = CONICAL_SURFACE ( 'NONE', #72681, 0.09999999999999982514, 0.003490658503988666988 ) ;
#99778 = PLANE ( 'NONE',  #45140 ) ;
#99779 = CARTESIAN_POINT ( 'NONE',  ( -8.150000000000012790, 12.50000000000000000, 2.511473670974873507 ) ) ;
#99780 = EDGE_CURVE ( 'NONE', #34236, #109647, #1795, .T. ) ;
#99781 = ORIENTED_EDGE ( 'NONE', *, *, #78727, .T. ) ;
#99783 = CIRCLE ( 'NONE', #124826, 0.06509327318403745899 ) ;
#99782 = AXIS2_PLACEMENT_3D ( 'NONE', #32680, #66610, #37174 ) ;
#99784 = LINE ( 'NONE', #79501, #88720 ) ;
#99785 = AXIS2_PLACEMENT_3D ( 'NONE', #46570, #75383, #25007 ) ;
#99786 = ORIENTED_EDGE ( 'NONE', *, *, #66425, .F. ) ;
#99787 = EDGE_LOOP ( 'NONE', ( #123935, #2714 ) ) ;
#99788 = CARTESIAN_POINT ( 'NONE',  ( 2.949999999999945111, 2.500000000000000000, 2.165063509461097713 ) ) ;
#99789 = EDGE_LOOP ( 'NONE', ( #34571, #52750, #9779, #79704 ) ) ;
#99790 = FACE_OUTER_BOUND ( 'NONE', #39899, .T. ) ;
#99791 = LINE ( 'NONE', #63573, #75737 ) ;
#99793 = AXIS2_PLACEMENT_3D ( 'NONE', #1915, #32702, #22230 ) ;
#99792 = AXIS2_PLACEMENT_3D ( 'NONE', #126651, #78201, #127934 ) ;
#99794 = ORIENTED_EDGE ( 'NONE', *, *, #12659, .F. ) ;
#99795 = DIRECTION ( 'NONE',  ( 0.000000000000000000, 0.000000000000000000, -1.000000000000000000 ) ) ;
#99796 = ADVANCED_FACE ( 'NONE', ( #14002 ), #93871, .T. ) ;
#99797 = DIRECTION ( 'NONE',  ( 0.000000000000000000, 0.000000000000000000, 1.000000000000000000 ) ) ;
#99798 = DIRECTION ( 'NONE',  ( -0.000000000000000000, 1.000000000000000000, -0.000000000000000000 ) ) ;
#99799 = ORIENTED_EDGE ( 'NONE', *, *, #51542, .F. ) ;
#99800 = ADVANCED_FACE ( 'NONE', ( #104333 ), #79192, .T. ) ;
#99801 = AXIS2_PLACEMENT_3D ( 'NONE', #115423, #25779, #4189 ) ;
#99802 = VERTEX_POINT ( 'NONE', #62724 ) ;
#99803 = ORIENTED_EDGE ( 'NONE', *, *, #41924, .F. ) ;
#99804 = CONICAL_SURFACE ( 'NONE', #70549, 0.1000000000000000472, 0.003490658503988666988 ) ;
#99805 = DIRECTION ( 'NONE',  ( -0.000000000000000000, -1.000000000000000000, -0.000000000000000000 ) ) ;
#99806 = DIRECTION ( 'NONE',  ( -0.000000000000000000, 1.000000000000000000, -0.000000000000000000 ) ) ;
#99807 = CARTESIAN_POINT ( 'NONE',  ( 11.64999999999990798, 2.500000000000000000, 7.188010851410848723 ) ) ;
#99808 = EDGE_CURVE ( 'NONE', #43427, #122964, #62467, .T. ) ;
#99809 = EDGE_CURVE ( 'NONE', #88819, #99762, #79768, .T. ) ;
#99810 = FACE_BOUND ( 'NONE', #82115, .T. ) ;
#99811 = ORIENTED_EDGE ( 'NONE', *, *, #59636, .F. ) ;
#99812 = ADVANCED_FACE ( 'NONE', ( #90876 ), #30040, .T. ) ;
#99813 = CIRCLE ( 'NONE', #30874, 0.1000000000000002554 ) ;
#99814 = EDGE_CURVE ( 'NONE', #128968, #103425, #9742, .T. ) ;
#99815 = DIRECTION ( 'NONE',  ( 0.000000000000000000, 0.000000000000000000, -1.000000000000000000 ) ) ;
#99816 = DIRECTION ( 'NONE',  ( 0.000000000000000000, 1.000000000000000000, 0.000000000000000000 ) ) ;
#99817 = VECTOR ( 'NONE', #80545, 1000.000000000000000 ) ;
#99818 = ORIENTED_EDGE ( 'NONE', *, *, #33380, .T. ) ;
#99819 = DIRECTION ( 'NONE',  ( 0.000000000000000000, 0.000000000000000000, 1.000000000000000000 ) ) ;
#99820 = CARTESIAN_POINT ( 'NONE',  ( 3.949999999999942446, 2.500000000000000000, -6.841600689897078702 ) ) ;
#99821 = CIRCLE ( 'NONE', #124942, 0.06509327318403745899 ) ;
#99822 = ADVANCED_FACE ( 'NONE', ( #30691 ), #129383, .T. ) ;
#99823 = DIRECTION ( 'NONE',  ( 0.000000000000000000, 1.000000000000000000, 0.000000000000000000 ) ) ;
#99824 = PLANE ( 'NONE',  #48663 ) ;
#99825 = DIRECTION ( 'NONE',  ( 1.000000000000000000, 0.000000000000000000, 0.000000000000000000 ) ) ;
#99826 = EDGE_CURVE ( 'NONE', #49458, #51199, #22806, .T. ) ;
#99827 = CARTESIAN_POINT ( 'NONE',  ( 8.749999999999920064, 12.50000000000000000, 5.867463478539781896 ) ) ;
#99828 = AXIS2_PLACEMENT_3D ( 'NONE', #78925, #69075, #39654 ) ;
#99829 = DIRECTION ( 'NONE',  ( 0.000000000000000000, 1.000000000000000000, 0.000000000000000000 ) ) ;
#99830 = CIRCLE ( 'NONE', #108225, 0.06509327318403745899 ) ;
#99831 = CIRCLE ( 'NONE', #22484, 9.000000000000001776 ) ;
#99832 = CONICAL_SURFACE ( 'NONE', #28821, 0.1000000000000002554, 0.003490658503988666988 ) ;
#99833 = EDGE_CURVE ( 'NONE', #64891, #103728, #89645, .T. ) ;
#99834 = VERTEX_POINT ( 'NONE', #20210 ) ;
#99835 = ORIENTED_EDGE ( 'NONE', *, *, #60469, .T. ) ;
#99836 = ORIENTED_EDGE ( 'NONE', *, *, #35919, .F. ) ;
#99837 = ORIENTED_EDGE ( 'NONE', *, *, #59365, .T. ) ;
#99838 = DIRECTION ( 'NONE',  ( 0.000000000000000000, 0.000000000000000000, -1.000000000000000000 ) ) ;
#99839 = DIRECTION ( 'NONE',  ( -0.000000000000000000, 1.000000000000000000, -0.000000000000000000 ) ) ;
#99840 = EDGE_LOOP ( 'NONE', ( #68063, #65584, #86734, #104538 ) ) ;
#99841 = EDGE_CURVE ( 'NONE', #70779, #122261, #60423, .T. ) ;
#99842 = FACE_BOUND ( 'NONE', #25983, .T. ) ;
#99843 = EDGE_CURVE ( 'NONE', #64309, #127944, #37429, .T. ) ;
#99844 = CARTESIAN_POINT ( 'NONE',  ( -1.650000000000035660, 12.50000000000000000, 2.922977105672686982 ) ) ;
#99845 = CONICAL_SURFACE ( 'NONE', #89458, 0.1000000000000002554, 0.003490658503988666988 ) ;
#99846 = DIRECTION ( 'NONE',  ( -0.000000000000000000, -1.000000000000000000, -0.000000000000000000 ) ) ;
#99847 = DIRECTION ( 'NONE',  ( 0.000000000000000000, -0.000000000000000000, 1.000000000000000000 ) ) ;
#99848 = FACE_OUTER_BOUND ( 'NONE', #20862, .T. ) ;
#99849 = CARTESIAN_POINT ( 'NONE',  ( -6.650000000000014566, 2.500000000000000000, 5.702370205355745014 ) ) ;
#99850 = DIRECTION ( 'NONE',  ( 0.000000000000000000, 0.000000000000000000, -1.000000000000000000 ) ) ;
#99851 = ORIENTED_EDGE ( 'NONE', *, *, #97270, .T. ) ;
#99852 = VERTEX_POINT ( 'NONE', #41804 ) ;
#99853 = EDGE_LOOP ( 'NONE', ( #52906, #72653, #36275, #23453 ) ) ;
#99854 = ORIENTED_EDGE ( 'NONE', *, *, #22832, .T. ) ;
#99855 = EDGE_LOOP ( 'NONE', ( #103659, #114750, #59729, #74584 ) ) ;
#99856 = ORIENTED_EDGE ( 'NONE', *, *, #36573, .F. ) ;
#99857 = DIRECTION ( 'NONE',  ( 0.000000000000000000, 0.000000000000000000, 1.000000000000000000 ) ) ;
#99858 = CARTESIAN_POINT ( 'NONE',  ( 6.649999999999927525, 2.500000000000000000, 2.165063509461097713 ) ) ;
#99859 = ORIENTED_EDGE ( 'NONE', *, *, #19538, .F. ) ;
#99860 = AXIS2_PLACEMENT_3D ( 'NONE', #117298, #38134, #27643 ) ;
#99861 = CARTESIAN_POINT ( 'NONE',  ( -4.400000000000025224, 12.50000000000000000, 4.676537180435972552 ) ) ;
#99862 = CARTESIAN_POINT ( 'NONE',  ( -0.8500000000000386136, 2.500000000000000000, 2.857883832488649301 ) ) ;
#99863 = CARTESIAN_POINT ( 'NONE',  ( 4.149999999999938183, 12.50000000000000000, 2.165063509461097713 ) ) ;
#99864 = CARTESIAN_POINT ( 'NONE',  ( 185.5677083336747160, -4.367472073101514418, -7.564683531250002702 ) ) ;
#99865 = LINE ( 'NONE', #10190, #50037 ) ;
#99866 = DIRECTION ( 'NONE',  ( 0.000000000000000000, 0.000000000000000000, 1.000000000000000000 ) ) ;
#99867 = DIRECTION ( 'NONE',  ( -0.000000000000000000, -1.000000000000000000, -0.000000000000000000 ) ) ;
#99868 = ORIENTED_EDGE ( 'NONE', *, *, #58141, .F. ) ;
#99869 = DIRECTION ( 'NONE',  ( -0.000000000000000000, -1.000000000000000000, -0.000000000000000000 ) ) ;
#99870 = AXIS2_PLACEMENT_3D ( 'NONE', #23380, #63314, #103249 ) ;
#99871 = EDGE_LOOP ( 'NONE', ( #70821, #30613, #99425, #127700 ) ) ;
#99872 = EDGE_CURVE ( 'NONE', #82187, #105036, #91791, .T. ) ;
#99873 = VECTOR ( 'NONE', #72098, 1000.000000000000000 ) ;
#99874 = VERTEX_POINT ( 'NONE', #550 ) ;
#99875 = FACE_OUTER_BOUND ( 'NONE', #121160, .T. ) ;
#99876 = EDGE_CURVE ( 'NONE', #56688, #105502, #114760, .T. ) ;
#99877 = CARTESIAN_POINT ( 'NONE',  ( 12.69999999999990337, 2.500000000000000000, 3.983716857408420076 ) ) ;
#99878 = CARTESIAN_POINT ( 'NONE',  ( -0.2000000000000408673, 12.50000000000000000, -3.983716857408426293 ) ) ;
#99879 = EDGE_LOOP ( 'NONE', ( #56537, #14486, #16010, #13041 ) ) ;
#99881 = EDGE_LOOP ( 'NONE', ( #104531, #57932 ) ) ;
#99880 = CIRCLE ( 'NONE', #87333, 1.000000000000000000 ) ;
#99882 = DIRECTION ( 'NONE',  ( 0.000000000000000000, 0.000000000000000000, 1.000000000000000000 ) ) ;
#99883 = VECTOR ( 'NONE', #27565, 1000.000000000000000 ) ;
#99884 = AXIS2_PLACEMENT_3D ( 'NONE', #78128, #19852, #106917 ) ;
#99885 = CARTESIAN_POINT ( 'NONE',  ( 6.899999999999928413, 2.500000000000000000, -4.676537180435977881 ) ) ;
#99886 = DIRECTION ( 'NONE',  ( 0.000000000000000000, 1.000000000000000000, 0.000000000000000000 ) ) ;
#99887 = DIRECTION ( 'NONE',  ( 0.000000000000000000, 0.000000000000000000, 1.000000000000000000 ) ) ;
#99888 = VERTEX_POINT ( 'NONE', #40515 ) ;
#99889 = CARTESIAN_POINT ( 'NONE',  ( 3.149999999999944400, 12.50000000000000000, 2.576566944158910744 ) ) ;
#99890 = ORIENTED_EDGE ( 'NONE', *, *, #94648, .T. ) ;
#99891 = CARTESIAN_POINT ( 'NONE',  ( -4.119968255444916849E-14, 2.500000000000000000, 3.737306695894644371 ) ) ;
#99892 = ORIENTED_EDGE ( 'NONE', *, *, #128001, .T. ) ;
#99893 = FACE_OUTER_BOUND ( 'NONE', #70077, .T. ) ;
#99894 = FACE_OUTER_BOUND ( 'NONE', #90832, .T. ) ;
#99895 = CARTESIAN_POINT ( 'NONE',  ( 6.649999999999931966, 12.50000000000000000, -5.802370205355749988 ) ) ;
#99896 = AXIS2_PLACEMENT_3D ( 'NONE', #71567, #11362, #70292 ) ;
#99897 = CARTESIAN_POINT ( 'NONE',  ( 8.349999999999923261, 12.50000000000000000, -5.737276932171712751 ) ) ;
#99898 = EDGE_LOOP ( 'NONE', ( #60851, #69717, #43806, #6446 ) ) ;
#99900 = CONICAL_SURFACE ( 'NONE', #120821, 0.1000000000000002554, 0.003490658503988666988 ) ;
#99899 = CARTESIAN_POINT ( 'NONE',  ( -11.64999999999999680, 12.50000000000000000, 6.560283801567334372 ) ) ;
#99901 = AXIS2_PLACEMENT_3D ( 'NONE', #118690, #30339, #193 ) ;
#99902 = FACE_OUTER_BOUND ( 'NONE', #19190, .T. ) ;
#99903 = EDGE_LOOP ( 'NONE', ( #27400, #28124 ) ) ;
#99904 = ORIENTED_EDGE ( 'NONE', *, *, #99337, .F. ) ;
#99905 = DIRECTION ( 'NONE',  ( -0.000000000000000000, -1.000000000000000000, -0.000000000000000000 ) ) ;
#99906 = CARTESIAN_POINT ( 'NONE',  ( 8.549999999999918998, 2.500000000000000000, 6.741600689897071952 ) ) ;
#99907 = DIRECTION ( 'NONE',  ( -0.000000000000000000, -1.000000000000000000, -0.000000000000000000 ) ) ;
#99908 = CIRCLE ( 'NONE', #30968, 0.1000000000000002554 ) ;
#99910 = VECTOR ( 'NONE', #88423, 1000.000000000000000 ) ;
#99909 = FACE_OUTER_BOUND ( 'NONE', #461, .T. ) ;
#99911 = DIRECTION ( 'NONE',  ( 0.000000000000000000, -0.000000000000000000, 1.000000000000000000 ) ) ;
#99912 = EDGE_CURVE ( 'NONE', #56997, #123277, #87572, .T. ) ;
#99913 = AXIS2_PLACEMENT_3D ( 'NONE', #83981, #94448, #5424 ) ;
#99914 = CARTESIAN_POINT ( 'NONE',  ( 2.499999999999948930, 12.50000000000000000, -0.6928203230275541413 ) ) ;
#99915 = PLANE ( 'NONE',  #120177 ) ;
#99916 = CARTESIAN_POINT ( 'NONE',  ( 149.5981739382431783, 2.500000000000000000, -1.703575533167231537 ) ) ;
#99917 = CIRCLE ( 'NONE', #43489, 0.1000000000000002554 ) ;
#99918 = ADVANCED_FACE ( 'NONE', ( #80427 ), #45828, .T. ) ;
#99919 = VECTOR ( 'NONE', #14905, 1000.000000000000000 ) ;
#99920 = EDGE_LOOP ( 'NONE', ( #126469, #112052 ) ) ;
#99921 = CARTESIAN_POINT ( 'NONE',  ( 13.14999999999990088, 2.500000000000000000, 1.818653347947321475 ) ) ;
#99922 = EDGE_CURVE ( 'NONE', #16723, #82111, #101995, .T. ) ;
#99923 = CIRCLE ( 'NONE', #7871, 0.06509327318403745899 ) ;
#99924 = DIRECTION ( 'NONE',  ( 0.000000000000000000, 0.000000000000000000, -1.000000000000000000 ) ) ;
#99926 = EDGE_CURVE ( 'NONE', #17094, #34777, #50972, .T. ) ;
#99925 = CARTESIAN_POINT ( 'NONE',  ( -6.650000000000019007, 12.50000000000000000, -1.472243186433550122 ) ) ;
#99927 = CARTESIAN_POINT ( 'NONE',  ( -11.44999999999999929, 2.500000000000000000, -1.918653347947322230 ) ) ;
#99928 = FACE_OUTER_BOUND ( 'NONE', #97652, .T. ) ;
#99929 = VERTEX_POINT ( 'NONE', #71230 ) ;
#99930 = CARTESIAN_POINT ( 'NONE',  ( -7.900000000000014566, 12.50000000000000000, -4.265033745738164406 ) ) ;
#99932 = AXIS2_PLACEMENT_3D ( 'NONE', #339, #79571, #9541 ) ;
#99931 = CONICAL_SURFACE ( 'NONE', #47788, 0.1000000000000002554, 0.003490658503988666988 ) ;
#99933 = PLANE ( 'NONE',  #7275 ) ;
#99935 = VERTEX_POINT ( 'NONE', #111819 ) ;
#99934 = CARTESIAN_POINT ( 'NONE',  ( 8.749999999999957367, 12.50000000000000000, 2.165063509461097713 ) ) ;
#99936 = EDGE_CURVE ( 'NONE', #116685, #94318, #31172, .T. ) ;
#99937 = ORIENTED_EDGE ( 'NONE', *, *, #3504, .T. ) ;
#99938 = CARTESIAN_POINT ( 'NONE',  ( 7.099999999999927702, 2.500000000000000000, -3.637306695894650055 ) ) ;
#99939 = ORIENTED_EDGE ( 'NONE', *, *, #83551, .T. ) ;
#99940 = ORIENTED_EDGE ( 'NONE', *, *, #82505, .T. ) ;
#99941 = FACE_OUTER_BOUND ( 'NONE', #18693, .T. ) ;
#99942 = DIRECTION ( 'NONE',  ( 0.000000000000000000, 0.000000000000000000, 1.000000000000000000 ) ) ;
#99943 = DIRECTION ( 'NONE',  ( -0.000000000000000000, 1.000000000000000000, -0.000000000000000000 ) ) ;
#99944 = CARTESIAN_POINT ( 'NONE',  ( -3.750000000000025757, 2.500000000000000000, 1.372243186433545370 ) ) ;
#99945 = VERTEX_POINT ( 'NONE', #2477 ) ;
#99946 = AXIS2_PLACEMENT_3D ( 'NONE', #19682, #11782, #59630 ) ;
#99947 = CARTESIAN_POINT ( 'NONE',  ( 127.5000000000000000, -1.500000000000000000, -6.000000000000000000 ) ) ;
#99948 = ORIENTED_EDGE ( 'NONE', *, *, #68617, .T. ) ;
#99949 = DIRECTION ( 'NONE',  ( 0.000000000000000000, -0.000000000000000000, 1.000000000000000000 ) ) ;
#99950 = CIRCLE ( 'NONE', #60260, 0.06509327318403745899 ) ;
#99951 = DIRECTION ( 'NONE',  ( 0.000000000000000000, 1.000000000000000000, 0.000000000000000000 ) ) ;
#99952 = DIRECTION ( 'NONE',  ( 0.000000000000000000, 0.000000000000000000, 1.000000000000000000 ) ) ;
#99953 = ORIENTED_EDGE ( 'NONE', *, *, #18657, .F. ) ;
#99954 = CIRCLE ( 'NONE', #3806, 0.06509327318403745899 ) ;
#99955 = EDGE_CURVE ( 'NONE', #107304, #46456, #116904, .T. ) ;
#99956 = CIRCLE ( 'NONE', #106306, 0.06509327318403745899 ) ;
#99957 = ORIENTED_EDGE ( 'NONE', *, *, #80621, .F. ) ;
#99958 = EDGE_LOOP ( 'NONE', ( #115876, #72176, #36012, #48582 ) ) ;
#99959 = EDGE_LOOP ( 'NONE', ( #83119, #47212, #78885, #115391 ) ) ;
#99960 = VERTEX_POINT ( 'NONE', #72542 ) ;
#99961 = DIRECTION ( 'NONE',  ( 0.000000000000000000, 0.000000000000000000, 1.000000000000000000 ) ) ;
#99962 = CARTESIAN_POINT ( 'NONE',  ( 12.65326442612249735, 2.499999999999999112, 8.428886917614240915 ) ) ;
#99963 = DIRECTION ( 'NONE',  ( -0.000000000000000000, 1.000000000000000000, -0.000000000000000000 ) ) ;
#99964 = ADVANCED_FACE ( 'NONE', ( #105202 ), #41646, .T. ) ;
#99965 = FACE_BOUND ( 'NONE', #103087, .T. ) ;
#99966 = CARTESIAN_POINT ( 'NONE',  ( -2.500000000000032419, 2.500000000000000000, 0.7928203230275495672 ) ) ;
#99967 = CARTESIAN_POINT ( 'NONE',  ( 186.1979166673494603, 6.668395609140176816, 3.850000000000000977 ) ) ;
#99969 = EDGE_CURVE ( 'NONE', #39409, #45762, #22858, .T. ) ;
#99968 = CONICAL_SURFACE ( 'NONE', #110421, 0.1000000000000000472, 0.003490658503988666988 ) ;
#99970 = DIRECTION ( 'NONE',  ( -0.000000000000000000, -1.000000000000000000, -0.000000000000000000 ) ) ;
#99971 = CARTESIAN_POINT ( 'NONE',  ( 8.749999999999918288, 2.500000000000000000, -1.572243186433550211 ) ) ;
#99972 = CIRCLE ( 'NONE', #35143, 0.06509327318403745899 ) ;
#99973 = EDGE_CURVE ( 'NONE', #41348, #115380, #3952, .T. ) ;
#99974 = CARTESIAN_POINT ( 'NONE',  ( -4.350000000000027178, 12.50000000000000000, -6.841600689897077814 ) ) ;
#99975 = EDGE_CURVE ( 'NONE', #27857, #113935, #68806, .T. ) ;
#99976 = DIRECTION ( 'NONE',  ( 0.000000000000000000, 1.000000000000000000, 0.000000000000000000 ) ) ;
#99977 = EDGE_CURVE ( 'NONE', #35495, #99852, #127306, .T. ) ;
#99978 = CARTESIAN_POINT ( 'NONE',  ( 4.799999999999939426, 2.500000000000000000, -4.676537180435977881 ) ) ;
#99979 = EDGE_CURVE ( 'NONE', #93665, #37844, #12363, .T. ) ;
#99980 = VECTOR ( 'NONE', #64734, 1000.000000000000000 ) ;
#99981 = CARTESIAN_POINT ( 'NONE',  ( -6.700000000000019718, 2.500000000000000000, -4.330127018922201643 ) ) ;
#99982 = EDGE_CURVE ( 'NONE', #79044, #26093, #60510, .T. ) ;
#99983 = VERTEX_POINT ( 'NONE', #63354 ) ;
#99984 = VERTEX_POINT ( 'NONE', #93456 ) ;
#99985 = ORIENTED_EDGE ( 'NONE', *, *, #49763, .F. ) ;
#99986 = ORIENTED_EDGE ( 'NONE', *, *, #52681, .T. ) ;
#99987 = CONICAL_SURFACE ( 'NONE', #98001, 0.09999999999999982514, 0.003490658503988666988 ) ;
#99988 = CARTESIAN_POINT ( 'NONE',  ( 9.549999999999918998, 2.500000000000000000, -6.395190528383301931 ) ) ;
#99989 = LINE ( 'NONE', #18833, #103028 ) ;
#99990 = FACE_BOUND ( 'NONE', #83573, .T. ) ;
#99991 = ADVANCED_FACE ( 'NONE', ( #95391 ), #95997, .T. ) ;
#99992 = CARTESIAN_POINT ( 'NONE',  ( 1.449999999999952216, 2.500000000000000000, -2.411473670974877859 ) ) ;
#99993 = MECHANICAL_DESIGN_GEOMETRIC_PRESENTATION_REPRESENTATION (  '', ( #28984 ), #81215 ) ;
#99994 = ORIENTED_EDGE ( 'NONE', *, *, #111115, .F. ) ;
#99995 = DIRECTION ( 'NONE',  ( 0.000000000000000000, -0.9999939076577903929, 0.003490651415223739937 ) ) ;
#99996 = DIRECTION ( 'NONE',  ( 0.000000000000000000, 0.000000000000000000, 1.000000000000000000 ) ) ;
#99997 = DIRECTION ( 'NONE',  ( -0.000000000000000000, 1.000000000000000000, -0.000000000000000000 ) ) ;
#99998 = DIRECTION ( 'NONE',  ( -0.000000000000000000, -1.000000000000000000, -0.000000000000000000 ) ) ;
#99999 = VERTEX_POINT ( 'NONE', #43098 ) ;
#100000 = CONICAL_SURFACE ( 'NONE', #102147, 0.1000000000000000472, 0.003490658503988666988 ) ;
#100001 = DIRECTION ( 'NONE',  ( 0.000000000000000000, 0.000000000000000000, 1.000000000000000000 ) ) ;
#100002 = CIRCLE ( 'NONE', #125132, 0.06509327318403745899 ) ;
#100003 = ORIENTED_EDGE ( 'NONE', *, *, #43227, .T. ) ;
#100004 = VERTEX_POINT ( 'NONE', #125489 ) ;
#100005 = DIRECTION ( 'NONE',  ( 0.000000000000000000, 1.000000000000000000, 0.000000000000000000 ) ) ;
#100006 = DIRECTION ( 'NONE',  ( 0.000000000000000000, 1.000000000000000000, 0.000000000000000000 ) ) ;
#100007 = AXIS2_PLACEMENT_3D ( 'NONE', #93723, #121890, #61702 ) ;
#100008 = ORIENTED_EDGE ( 'NONE', *, *, #58298, .F. ) ;
#100009 = FACE_OUTER_BOUND ( 'NONE', #1648, .T. ) ;
#100010 = FACE_OUTER_BOUND ( 'NONE', #128279, .T. ) ;
#100011 = CARTESIAN_POINT ( 'NONE',  ( -2.500000000000030642, 12.50000000000000000, -0.6277270498435166823 ) ) ;
#100012 = ORIENTED_EDGE ( 'NONE', *, *, #78276, .F. ) ;
#100013 = CIRCLE ( 'NONE', #35186, 0.1000000000000002554 ) ;
#100014 = PLANE ( 'NONE',  #82915 ) ;
#100015 = ORIENTED_EDGE ( 'NONE', *, *, #5834, .F. ) ;
#100016 = CARTESIAN_POINT ( 'NONE',  ( -1.900000000000034106, 12.50000000000000000, 0.4115034346978109769 ) ) ;
#100018 = CONICAL_SURFACE ( 'NONE', #39405, 0.1000000000000000472, 0.003490658503988666988 ) ;
#100017 = CIRCLE ( 'NONE', #70767, 0.09999999999999982514 ) ;
#100019 = VERTEX_POINT ( 'NONE', #34561 ) ;
#100020 = ADVANCED_FACE ( 'NONE', ( #14234 ), #14408, .T. ) ;
#100021 = CARTESIAN_POINT ( 'NONE',  ( 110.5285083638605244, 6.373905227100763682, 4.325246220449017187 ) ) ;
#100022 = ORIENTED_EDGE ( 'NONE', *, *, #8198, .T. ) ;
#100023 = DIRECTION ( 'NONE',  ( 0.000000000000000000, 0.000000000000000000, -1.000000000000000000 ) ) ;
#100024 = CARTESIAN_POINT ( 'NONE',  ( -11.05000000000000249, 12.50000000000000000, -6.148780366869522673 ) ) ;
#100025 = DIRECTION ( 'NONE',  ( 0.000000000000000000, 0.000000000000000000, 1.000000000000000000 ) ) ;
#100026 = DIRECTION ( 'NONE',  ( -0.000000000000000000, -1.000000000000000000, -0.000000000000000000 ) ) ;
#100027 = DIRECTION ( 'NONE',  ( 0.000000000000000000, 0.000000000000000000, 1.000000000000000000 ) ) ;
#100028 = ORIENTED_EDGE ( 'NONE', *, *, #106869, .F. ) ;
#100029 = ORIENTED_EDGE ( 'NONE', *, *, #90922, .T. ) ;
#100030 = EDGE_CURVE ( 'NONE', #19145, #66592, #39593, .T. ) ;
#100031 = ORIENTED_EDGE ( 'NONE', *, *, #123322, .F. ) ;
#100032 = CARTESIAN_POINT ( 'NONE',  ( 15.59999999999988951, 2.500000000000000000, -0.3464101615137783474 ) ) ;
#100033 = CARTESIAN_POINT ( 'NONE',  ( -12.09999999999999609, 12.50000000000000000, 0.6928203230275535862 ) ) ;
#100034 = LINE ( 'NONE', #48348, #106620 ) ;
#100037 = ORIENTED_EDGE ( 'NONE', *, *, #94826, .T. ) ;
#100036 = EDGE_LOOP ( 'NONE', ( #88476, #108995 ) ) ;
#100035 = CONICAL_SURFACE ( 'NONE', #68628, 0.1000000000000000472, 0.003490658503988666988 ) ;
#100038 = ORIENTED_EDGE ( 'NONE', *, *, #11507, .F. ) ;
#100039 = DIRECTION ( 'NONE',  ( 0.000000000000000000, 0.000000000000000000, 1.000000000000000000 ) ) ;
#100040 = ORIENTED_EDGE ( 'NONE', *, *, #40074, .F. ) ;
#100041 = CARTESIAN_POINT ( 'NONE',  ( 195.0000000000000000, 0.000000000000000000, 0.000000000000000000 ) ) ;
#100042 = VECTOR ( 'NONE', #49229, 1000.000000000000000 ) ;
#100043 = DIRECTION ( 'NONE',  ( -0.000000000000000000, 1.000000000000000000, -0.000000000000000000 ) ) ;
#100044 = CARTESIAN_POINT ( 'NONE',  ( 4.799999999999934097, 2.500000000000000000, 4.576537180435972019 ) ) ;
#100045 = DIRECTION ( 'NONE',  ( -0.000000000000000000, -1.000000000000000000, -0.000000000000000000 ) ) ;
#100046 = DIRECTION ( 'NONE',  ( 0.000000000000000000, -1.000000000000000000, 0.000000000000000000 ) ) ;
#100047 = DIRECTION ( 'NONE',  ( -0.000000000000000000, -1.000000000000000000, -0.000000000000000000 ) ) ;
#100048 = DIRECTION ( 'NONE',  ( 0.000000000000000000, 0.000000000000000000, 1.000000000000000000 ) ) ;
#100049 = CIRCLE ( 'NONE', #112571, 0.1000000000000002554 ) ;
#100050 = ORIENTED_EDGE ( 'NONE', *, *, #35991, .T. ) ;
#100052 = ORIENTED_EDGE ( 'NONE', *, *, #38032, .F. ) ;
#100051 = AXIS2_PLACEMENT_3D ( 'NONE', #127717, #108074, #38061 ) ;
#100054 = DIRECTION ( 'NONE',  ( 0.000000000000000000, 0.000000000000000000, 1.000000000000000000 ) ) ;
#100053 = CONICAL_SURFACE ( 'NONE', #125184, 0.09999999999999982514, 0.003490658503988666988 ) ;
#100055 = AXIS2_PLACEMENT_3D ( 'NONE', #100334, #51251, #81341 ) ;
#100056 = ORIENTED_EDGE ( 'NONE', *, *, #68777, .T. ) ;
#100057 = VERTEX_POINT ( 'NONE', #103285 ) ;
#100058 = CARTESIAN_POINT ( 'NONE',  ( 185.3177083336747160, 4.367472073101515306, 7.564683531250000925 ) ) ;
#100059 = CARTESIAN_POINT ( 'NONE',  ( 10.39999999999991331, 12.50000000000000000, -0.06509327318403980434 ) ) ;
#100060 = CARTESIAN_POINT ( 'NONE',  ( -8.550000000000013145, 12.50000000000000000, -6.841600689897073373 ) ) ;
#100061 = CIRCLE ( 'NONE', #47837, 0.09999999999999999167 ) ;
#100062 = DIRECTION ( 'NONE',  ( 0.000000000000000000, 0.000000000000000000, 1.000000000000000000 ) ) ;
#100064 = EDGE_CURVE ( 'NONE', #114427, #82484, #74463, .T. ) ;
#100063 = AXIS2_PLACEMENT_3D ( 'NONE', #77215, #8448, #69306 ) ;
#100065 = LINE ( 'NONE', #20855, #86695 ) ;
#100066 = DIRECTION ( 'NONE',  ( 0.000000000000000000, 0.000000000000000000, 1.000000000000000000 ) ) ;
#100067 = CARTESIAN_POINT ( 'NONE',  ( -2.500000000000031086, 2.500000000000000000, 3.737306695894644371 ) ) ;
#100068 = CARTESIAN_POINT ( 'NONE',  ( 12.49999999999993960, 2.500000000000000000, 4.430127018922196847 ) ) ;
#100070 = EDGE_CURVE ( 'NONE', #5075, #38783, #1897, .T. ) ;
#100069 = AXIS2_PLACEMENT_3D ( 'NONE', #6767, #101942, #75523 ) ;
#100071 = ORIENTED_EDGE ( 'NONE', *, *, #81186, .F. ) ;
#100072 = ORIENTED_EDGE ( 'NONE', *, *, #116237, .T. ) ;
#100073 = CIRCLE ( 'NONE', #3922, 0.1000000000000000056 ) ;
#100074 = EDGE_CURVE ( 'NONE', #77073, #10639, #64634, .T. ) ;
#100075 = ORIENTED_EDGE ( 'NONE', *, *, #10204, .F. ) ;
#100076 = ORIENTED_EDGE ( 'NONE', *, *, #31960, .F. ) ;
#100077 = EDGE_CURVE ( 'NONE', #96401, #35080, #10314, .T. ) ;
#100078 = CARTESIAN_POINT ( 'NONE',  ( 1.849999999999949685, 12.50000000000000000, -2.511473670974877948 ) ) ;
#100079 = CARTESIAN_POINT ( 'NONE',  ( 0.8499999999999553468, 2.500000000000000000, 2.165063509461097713 ) ) ;
#100080 = EDGE_LOOP ( 'NONE', ( #94016, #11641, #102403, #91873 ) ) ;
#100081 = LINE ( 'NONE', #29413, #86233 ) ;
#100082 = FACE_OUTER_BOUND ( 'NONE', #51568, .T. ) ;
#100083 = AXIS2_PLACEMENT_3D ( 'NONE', #44859, #95883, #115496 ) ;
#100084 = ADVANCED_FACE ( 'NONE', ( #75108 ), #121034, .T. ) ;
#100085 = DIRECTION ( 'NONE',  ( 0.000000000000000000, -0.000000000000000000, 1.000000000000000000 ) ) ;
#100087 = ORIENTED_EDGE ( 'NONE', *, *, #71402, .F. ) ;
#100086 = DIRECTION ( 'NONE',  ( 0.000000000000000000, 1.000000000000000000, 0.000000000000000000 ) ) ;
#100088 = EDGE_CURVE ( 'NONE', #6835, #38646, #85526, .T. ) ;
#100089 = DIRECTION ( 'NONE',  ( -0.000000000000000000, 1.000000000000000000, -0.000000000000000000 ) ) ;
#100091 = VECTOR ( 'NONE', #53329, 1000.000000000000000 ) ;
#100090 = AXIS2_PLACEMENT_3D ( 'NONE', #211, #19881, #8739 ) ;
#100092 = DIRECTION ( 'NONE',  ( 0.000000000000000000, 1.000000000000000000, 0.000000000000000000 ) ) ;
#100093 = ORIENTED_EDGE ( 'NONE', *, *, #70663, .F. ) ;
#100094 = CIRCLE ( 'NONE', #31153, 0.1000000000000002554 ) ;
#100095 = EDGE_LOOP ( 'NONE', ( #36413, #98390, #127348, #77144 ) ) ;
#100096 = EDGE_LOOP ( 'NONE', ( #123232, #19054 ) ) ;
#100097 = ORIENTED_EDGE ( 'NONE', *, *, #41922, .T. ) ;
#100098 = CARTESIAN_POINT ( 'NONE',  ( 0.1999999999999627909, 2.500000000000000000, 0.2464101615137758439 ) ) ;
#100099 = AXIS2_PLACEMENT_3D ( 'NONE', #24520, #93909, #46096 ) ;
#100100 = CARTESIAN_POINT ( 'NONE',  ( -1.445602896647332014E-16, 5.000000000000000000, -1.999999999999989120 ) ) ;
#100101 = DIRECTION ( 'NONE',  ( -0.000000000000000000, -1.000000000000000000, -0.000000000000000000 ) ) ;
#100103 = CIRCLE ( 'NONE', #43690, 7.699999999999999289 ) ;
#100102 = CIRCLE ( 'NONE', #54401, 0.1000000000000002554 ) ;
#100104 = CARTESIAN_POINT ( 'NONE',  ( -2.900000000000030109, 2.500000000000000000, 0.5928203230275495006 ) ) ;
#100105 = EDGE_LOOP ( 'NONE', ( #100660, #83313 ) ) ;
#100106 = DIRECTION ( 'NONE',  ( -0.000000000000000000, 1.000000000000000000, -0.000000000000000000 ) ) ;
#100108 = AXIS2_PLACEMENT_3D ( 'NONE', #470, #91446, #80352 ) ;
#100107 = CARTESIAN_POINT ( 'NONE',  ( -9.600000000000008527, 12.50000000000000000, -2.385244779468109755E-15 ) ) ;
#100109 = DIRECTION ( 'NONE',  ( 0.000000000000000000, 0.000000000000000000, 1.000000000000000000 ) ) ;
#100110 = CARTESIAN_POINT ( 'NONE',  ( -7.300000000000013145, 2.500000000000000000, 3.983716857408420076 ) ) ;
#100111 = ORIENTED_EDGE ( 'NONE', *, *, #108820, .F. ) ;
#100113 = CONICAL_SURFACE ( 'NONE', #16464, 0.09999999999999982514, 0.003490658503988666988 ) ;
#100112 = AXIS2_PLACEMENT_3D ( 'NONE', #61439, #119682, #100682 ) ;
#100114 = CARTESIAN_POINT ( 'NONE',  ( 187.2916666666666572, 4.445597072760113733, -7.700000000000009948 ) ) ;
#100115 = ORIENTED_EDGE ( 'NONE', *, *, #116236, .F. ) ;
#100116 = EDGE_LOOP ( 'NONE', ( #54096, #6937, #77625, #4526 ) ) ;
#100117 = PLANE ( 'NONE',  #74833 ) ;
#100118 = LINE ( 'NONE', #11066, #18852 ) ;
#100119 = FACE_BOUND ( 'NONE', #5549, .T. ) ;
#100120 = CARTESIAN_POINT ( 'NONE',  ( -6.250000000000019540, 2.500000000000000000, -7.188010851410854052 ) ) ;
#100121 = CARTESIAN_POINT ( 'NONE',  ( 11.24999999999990585, 12.50000000000000000, -5.802370205355749988 ) ) ;
#100122 = CARTESIAN_POINT ( 'NONE',  ( 5.649999999999934630, 12.50000000000000000, 6.906693963081109722 ) ) ;
#100123 = EDGE_CURVE ( 'NONE', #55074, #64406, #81335, .T. ) ;
#100124 = CONICAL_SURFACE ( 'NONE', #116828, 0.1000000000000002554, 0.003490658503988666988 ) ;
#100125 = EDGE_CURVE ( 'NONE', #93392, #110307, #112728, .T. ) ;
#100126 = CARTESIAN_POINT ( 'NONE',  ( 9.599999999999917932, 2.500000000000000000, 0.09999999999999772959 ) ) ;
#100127 = DIRECTION ( 'NONE',  ( 0.000000000000000000, 0.000000000000000000, 1.000000000000000000 ) ) ;
#100128 = CARTESIAN_POINT ( 'NONE',  ( -0.4000000000000392131, 12.50000000000000000, -4.330127018922201643 ) ) ;
#100129 = ADVANCED_FACE ( 'NONE', ( #56097 ), #129475, .T. ) ;
#100130 = CARTESIAN_POINT ( 'NONE',  ( 186.4895833340161460, -4.445597072760135937, -7.699999999999966427 ) ) ;
#100131 = ORIENTED_EDGE ( 'NONE', *, *, #113142, .T. ) ;
#100132 = ADVANCED_FACE ( 'NONE', ( #36492 ), #93844, .T. ) ;
#100133 = DIRECTION ( 'NONE',  ( 0.000000000000000000, 0.000000000000000000, 1.000000000000000000 ) ) ;
#100134 = CIRCLE ( 'NONE', #18557, 0.06509327318403745899 ) ;
#100135 = AXIS2_PLACEMENT_3D ( 'NONE', #52903, #39875, #100695 ) ;
#100136 = CARTESIAN_POINT ( 'NONE',  ( 9.999999999999912959, 2.500000000000000000, -5.122947341949753763 ) ) ;
#100137 = EDGE_CURVE ( 'NONE', #4249, #93494, #27040, .T. ) ;
#100138 = ORIENTED_EDGE ( 'NONE', *, *, #118111, .T. ) ;
#100139 = VERTEX_POINT ( 'NONE', #7638 ) ;
#100140 = CARTESIAN_POINT ( 'NONE',  ( 187.5000000000000000, -1.500000000000000000, -6.000000000000000000 ) ) ;
#100141 = CARTESIAN_POINT ( 'NONE',  ( 195.0000000000000000, 0.000000000000000000, 0.000000000000000000 ) ) ;
#100142 = FACE_BOUND ( 'NONE', #111810, .T. ) ;
#100143 = CARTESIAN_POINT ( 'NONE',  ( 10.61495711629423155, -2.500000000000001332, -8.020491763388223561 ) ) ;
#100144 = AXIS2_PLACEMENT_3D ( 'NONE', #107641, #106972, #67042 ) ;
#100146 = EDGE_CURVE ( 'NONE', #60649, #15598, #77042, .T. ) ;
#100145 = CIRCLE ( 'NONE', #35306, 0.06509327318403745899 ) ;
#100147 = AXIS2_PLACEMENT_3D ( 'NONE', #19366, #88094, #78327 ) ;
#100148 = ADVANCED_FACE ( 'NONE', ( #86188 ), #60602, .T. ) ;
#100149 = DIRECTION ( 'NONE',  ( -0.000000000000000000, -1.000000000000000000, -0.000000000000000000 ) ) ;
#100150 = ORIENTED_EDGE ( 'NONE', *, *, #43814, .F. ) ;
#100151 = DIRECTION ( 'NONE',  ( 0.000000000000000000, 0.000000000000000000, 1.000000000000000000 ) ) ;
#100152 = CARTESIAN_POINT ( 'NONE',  ( -4.076600168545496672E-14, 2.500000000000000000, -5.022947341949754119 ) ) ;
#100153 = CIRCLE ( 'NONE', #60464, 0.06509327318403745899 ) ;
#100154 = ORIENTED_EDGE ( 'NONE', *, *, #21341, .F. ) ;
#100155 = CARTESIAN_POINT ( 'NONE',  ( 179.5000000000000000, 0.000000000000000000, -6.000000000000000000 ) ) ;
#100156 = DIRECTION ( 'NONE',  ( 0.000000000000000000, 0.000000000000000000, 1.000000000000000000 ) ) ;
#100157 = AXIS2_PLACEMENT_3D ( 'NONE', #51630, #111834, #62098 ) ;
#100158 = CARTESIAN_POINT ( 'NONE',  ( 0.8499999999999553468, 12.50000000000000000, 2.165063509461097713 ) ) ;
#100159 = FACE_OUTER_BOUND ( 'NONE', #25293, .T. ) ;
#100160 = ORIENTED_EDGE ( 'NONE', *, *, #6502, .T. ) ;
#100161 = LINE ( 'NONE', #41254, #121935 ) ;
#100162 = CARTESIAN_POINT ( 'NONE',  ( -3.749999999999991562, 2.500000000000000000, 6.495190528383297135 ) ) ;
#100163 = DIRECTION ( 'NONE',  ( 0.000000000000000000, -0.000000000000000000, 1.000000000000000000 ) ) ;
#100164 = AXIS2_PLACEMENT_3D ( 'NONE', #65720, #116745, #95833 ) ;
#100165 = DIRECTION ( 'NONE',  ( 0.000000000000000000, 0.000000000000000000, 1.000000000000000000 ) ) ;
#100166 = ORIENTED_EDGE ( 'NONE', *, *, #111453, .F. ) ;
#100167 = ORIENTED_EDGE ( 'NONE', *, *, #62722, .T. ) ;
#100168 = ADVANCED_FACE ( 'NONE', ( #108423 ), #24981, .T. ) ;
#100169 = DIRECTION ( 'NONE',  ( 0.000000000000000000, -0.000000000000000000, 1.000000000000000000 ) ) ;
#100170 = VERTEX_POINT ( 'NONE', #128746 ) ;
#100171 = DIRECTION ( 'NONE',  ( 0.000000000000000000, -0.9999939076577903929, 0.003490651415223739937 ) ) ;
#100172 = DIRECTION ( 'NONE',  ( -4.274815082592931898E-19, -0.9999939076577903929, -0.003490651415223739937 ) ) ;
#100173 = CARTESIAN_POINT ( 'NONE',  ( -14.59999999999998366, 2.500000000000000000, 0.5928203230275517210 ) ) ;
#100174 = VERTEX_POINT ( 'NONE', #18107 ) ;
#100175 = DIRECTION ( 'NONE',  ( -4.274815082592931898E-19, -0.9999939076577903929, -0.003490651415223739937 ) ) ;
#100176 = CARTESIAN_POINT ( 'NONE',  ( -15.79999999999998117, 12.50000000000000000, 0.000000000000000000 ) ) ;
#100177 = DIRECTION ( 'NONE',  ( -0.000000000000000000, -1.000000000000000000, -0.000000000000000000 ) ) ;
#100178 = DIRECTION ( 'NONE',  ( 0.000000000000000000, 1.000000000000000000, 0.000000000000000000 ) ) ;
#100179 = LINE ( 'NONE', #28217, #31943 ) ;
#100180 = CIRCLE ( 'NONE', #31237, 0.1000000000000002554 ) ;
#100181 = FACE_OUTER_BOUND ( 'NONE', #10915, .T. ) ;
#100183 = VERTEX_POINT ( 'NONE', #58054 ) ;
#100182 = CIRCLE ( 'NONE', #33299, 0.06509327318403745899 ) ;
#100184 = ADVANCED_FACE ( 'NONE', ( #57403 ), #76401, .F. ) ;
#100185 = ORIENTED_EDGE ( 'NONE', *, *, #42610, .F. ) ;
#100186 = DIRECTION ( 'NONE',  ( 0.000000000000000000, 0.000000000000000000, 1.000000000000000000 ) ) ;
#100187 = ORIENTED_EDGE ( 'NONE', *, *, #95830, .T. ) ;
#100188 = DIRECTION ( 'NONE',  ( -0.000000000000000000, 1.000000000000000000, -0.000000000000000000 ) ) ;
#100190 = ORIENTED_EDGE ( 'NONE', *, *, #72215, .F. ) ;
#100189 = EDGE_LOOP ( 'NONE', ( #35908, #72389, #34002, #123990 ) ) ;
#100191 = ORIENTED_EDGE ( 'NONE', *, *, #67560, .T. ) ;
#100192 = CONICAL_SURFACE ( 'NONE', #60497, 0.1000000000000002554, 0.003490658503988666988 ) ;
#100193 = LINE ( 'NONE', #30175, #20723 ) ;
#100194 = CARTESIAN_POINT ( 'NONE',  ( -4.400000000000028777, 2.500000000000000000, -4.576537180435978236 ) ) ;
#100195 = DIRECTION ( 'NONE',  ( 0.000000000000000000, 0.000000000000000000, -1.000000000000000000 ) ) ;
#100196 = SURFACE_STYLE_USAGE ( .BOTH. , #41929 ) ;
#100197 = VECTOR ( 'NONE', #119543, 1000.000000000000000 ) ;
#100198 = CARTESIAN_POINT ( 'NONE',  ( -0.6000000000000323963, 12.50000000000000000, -0.4115034346978133639 ) ) ;
#100199 = LINE ( 'NONE', #49823, #121144 ) ;
#100200 = DIRECTION ( 'NONE',  ( -0.000000000000000000, 1.000000000000000000, -0.000000000000000000 ) ) ;
#100201 = CARTESIAN_POINT ( 'NONE',  ( 12.29999999999990479, 2.500000000000000000, -4.083716857408426826 ) ) ;
#100202 = CARTESIAN_POINT ( 'NONE',  ( 6.649999999999931966, 2.500000000000000000, -7.188010851410854052 ) ) ;
#100203 = VECTOR ( 'NONE', #24492, 1000.000000000000000 ) ;
#100204 = DIRECTION ( 'NONE',  ( 0.000000000000000000, 0.000000000000000000, 1.000000000000000000 ) ) ;
#100206 = AXIS2_PLACEMENT_3D ( 'NONE', #56134, #69169, #10273 ) ;
#100205 = AXIS2_PLACEMENT_3D ( 'NONE', #88112, #37759, #128077 ) ;
#100207 = EDGE_LOOP ( 'NONE', ( #45178, #67750 ) ) ;
#100208 = DIRECTION ( 'NONE',  ( 0.000000000000000000, 1.000000000000000000, 0.000000000000000000 ) ) ;
#100209 = ORIENTED_EDGE ( 'NONE', *, *, #109392, .T. ) ;
#100210 = ORIENTED_EDGE ( 'NONE', *, *, #83457, .T. ) ;
#100211 = CARTESIAN_POINT ( 'NONE',  ( 8.749999999999953815, 2.500000000000000000, -2.265063509461101798 ) ) ;
#100212 = DIRECTION ( 'NONE',  ( 0.000000000000000000, 0.000000000000000000, 1.000000000000000000 ) ) ;
#100213 = CARTESIAN_POINT ( 'NONE',  ( 8.099999999999923261, 12.50000000000000000, -4.676537180435978769 ) ) ;
#100214 = FACE_OUTER_BOUND ( 'NONE', #107983, .T. ) ;
#100215 = CARTESIAN_POINT ( 'NONE',  ( 1.049999999999954081, 2.500000000000000000, -6.248780366869526759 ) ) ;
#100217 = AXIS2_PLACEMENT_3D ( 'NONE', #88877, #12085, #61196 ) ;
#100216 = DIRECTION ( 'NONE',  ( 0.000000000000000000, -0.9999939076577903929, 0.003490651415223739937 ) ) ;
#100218 = ORIENTED_EDGE ( 'NONE', *, *, #82968, .F. ) ;
#100219 = ORIENTED_EDGE ( 'NONE', *, *, #111436, .F. ) ;
#100221 = DIRECTION ( 'NONE',  ( 0.000000000000000000, 0.000000000000000000, -1.000000000000000000 ) ) ;
#100220 = AXIS2_PLACEMENT_3D ( 'NONE', #120698, #70956, #21204 ) ;
#100222 = EDGE_CURVE ( 'NONE', #62914, #53677, #79370, .T. ) ;
#100224 = ORIENTED_EDGE ( 'NONE', *, *, #92005, .F. ) ;
#100223 = AXIS2_PLACEMENT_3D ( 'NONE', #93473, #3796, #103936 ) ;
#100225 = FACE_OUTER_BOUND ( 'NONE', #74340, .T. ) ;
#100226 = ORIENTED_EDGE ( 'NONE', *, *, #93211, .T. ) ;
#100227 = EDGE_CURVE ( 'NONE', #67249, #86863, #66559, .T. ) ;
#100228 = ORIENTED_EDGE ( 'NONE', *, *, #73044, .F. ) ;
#100229 = EDGE_CURVE ( 'NONE', #122300, #28419, #16644, .T. ) ;
#100231 = AXIS2_PLACEMENT_3D ( 'NONE', #57083, #125816, #5406 ) ;
#100230 = PLANE ( 'NONE',  #69089 ) ;
#100232 = DIRECTION ( 'NONE',  ( -0.000000000000000000, 1.000000000000000000, -0.000000000000000000 ) ) ;
#100233 = AXIS2_PLACEMENT_3D ( 'NONE', #36481, #56712, #107773 ) ;
#100234 = AXIS2_PLACEMENT_3D ( 'NONE', #36119, #36773, #5988 ) ;
#100235 = DIRECTION ( 'NONE',  ( -0.000000000000000000, 1.000000000000000000, -0.000000000000000000 ) ) ;
#100236 = CARTESIAN_POINT ( 'NONE',  ( -4.150000000000024336, 2.500000000000000000, -2.265063509461101798 ) ) ;
#100237 = EDGE_CURVE ( 'NONE', #6356, #2890, #28588, .T. ) ;
#100238 = FACE_OUTER_BOUND ( 'NONE', #84718, .T. ) ;
#100240 = ORIENTED_EDGE ( 'NONE', *, *, #109734, .F. ) ;
#100239 = EDGE_CURVE ( 'NONE', #11222, #108234, #6978, .T. ) ;
#100241 = DIRECTION ( 'NONE',  ( 0.000000000000000000, -0.000000000000000000, 1.000000000000000000 ) ) ;
#100242 = CARTESIAN_POINT ( 'NONE',  ( -3.100000000000028511, 2.500000000000000000, -0.3464101615137782364 ) ) ;
#100243 = EDGE_CURVE ( 'NONE', #127840, #110110, #64685, .T. ) ;
#100244 = DIRECTION ( 'NONE',  ( 0.000000000000000000, 1.000000000000000000, 0.000000000000000000 ) ) ;
#100245 = EDGE_CURVE ( 'NONE', #18590, #75910, #37125, .T. ) ;
#100246 = ADVANCED_FACE ( 'NONE', ( #67180 ), #116990, .T. ) ;
#100247 = DIRECTION ( 'NONE',  ( 0.000000000000000000, -0.000000000000000000, 1.000000000000000000 ) ) ;
#100248 = CIRCLE ( 'NONE', #102389, 0.09999999999999982514 ) ;
#100249 = DIRECTION ( 'NONE',  ( 0.000000000000000000, 0.000000000000000000, 1.000000000000000000 ) ) ;
#100250 = CIRCLE ( 'NONE', #35403, 0.1000000000000002554 ) ;
#100251 = ORIENTED_EDGE ( 'NONE', *, *, #78978, .F. ) ;
#100252 = CIRCLE ( 'NONE', #35505, 0.06509327318403745899 ) ;
#100253 = ORIENTED_EDGE ( 'NONE', *, *, #14401, .F. ) ;
#100254 = FACE_OUTER_BOUND ( 'NONE', #121469, .T. ) ;
#100255 = ADVANCED_FACE ( 'NONE', ( #107125 ), #47979, .T. ) ;
#100256 = ORIENTED_EDGE ( 'NONE', *, *, #124639, .T. ) ;
#100257 = CARTESIAN_POINT ( 'NONE',  ( 17.50000000000000355, -2.413248583741843589, 3.595440551767155934 ) ) ;
#100258 = DIRECTION ( 'NONE',  ( 0.000000000000000000, 0.000000000000000000, 1.000000000000000000 ) ) ;
#100259 = CIRCLE ( 'NONE', #83538, 0.06509327318403745899 ) ;
#100260 = ORIENTED_EDGE ( 'NONE', *, *, #16544, .T. ) ;
#100261 = CARTESIAN_POINT ( 'NONE',  ( 2.499999999999947153, 12.50000000000000000, 3.637306695894644726 ) ) ;
#100262 = DIRECTION ( 'NONE',  ( 0.000000000000000000, 0.000000000000000000, 1.000000000000000000 ) ) ;
#100263 = DIRECTION ( 'NONE',  ( 0.000000000000000000, 0.000000000000000000, -1.000000000000000000 ) ) ;
#100264 = DIRECTION ( 'NONE',  ( 0.000000000000000000, -0.9999939076577903929, 0.003490651415223739937 ) ) ;
#100265 = DIRECTION ( 'NONE',  ( 0.000000000000000000, 0.000000000000000000, -1.000000000000000000 ) ) ;
#100266 = VERTEX_POINT ( 'NONE', #8922 ) ;
#100267 =( BOUNDED_CURVE ( )  B_SPLINE_CURVE ( 2, ( #119003, #118353, #107890, #49640, #28703, #109166, #68606 ),
 .UNSPECIFIED., .F., .F. ) 
 B_SPLINE_CURVE_WITH_KNOTS ( ( 3, 2, 2, 3 ),
 ( 0.1428571428571429880, 0.1666666666666668239, 0.1904761904761906322, 0.2142857142857144681 ),
 .UNSPECIFIED. ) 
 CURVE ( )  GEOMETRIC_REPRESENTATION_ITEM ( )  RATIONAL_B_SPLINE_CURVE ( ( 0.9999999999999992228, 0.8660254037844394848, 1.000000000000000000, 0.8660254037844387076, 1.000000000000000000, 0.8660254037844375974, 1.000000000000001110 ) ) 
 REPRESENTATION_ITEM ( '' )  );
#100268 = CARTESIAN_POINT ( 'NONE',  ( 21.24754738303275658, 0.7337760880902297611, -4.182111650399359171 ) ) ;
#100269 = DIRECTION ( 'NONE',  ( -4.274815082592931898E-19, -0.9999939076577903929, -0.003490651415223739937 ) ) ;
#100270 = DIRECTION ( 'NONE',  ( 0.000000000000000000, 0.000000000000000000, 1.000000000000000000 ) ) ;
#100271 = DIRECTION ( 'NONE',  ( -0.000000000000000000, 1.000000000000000000, -0.000000000000000000 ) ) ;
#100272 = ORIENTED_EDGE ( 'NONE', *, *, #9492, .F. ) ;
#100273 = ORIENTED_EDGE ( 'NONE', *, *, #122437, .T. ) ;
#100274 = EDGE_CURVE ( 'NONE', #43147, #108043, #129567, .T. ) ;
#100276 = CIRCLE ( 'NONE', #8319, 0.1000000000000000472 ) ;
#100275 = CARTESIAN_POINT ( 'NONE',  ( -1.450000000000035039, 2.500000000000000000, -2.511473670974877948 ) ) ;
#100277 = DIRECTION ( 'NONE',  ( 0.000000000000000000, 0.000000000000000000, 1.000000000000000000 ) ) ;
#100278 = DIRECTION ( 'NONE',  ( 0.000000000000000000, 0.000000000000000000, 1.000000000000000000 ) ) ;
#100279 = EDGE_CURVE ( 'NONE', #93088, #119152, #6185, .T. ) ;
#100280 = ORIENTED_EDGE ( 'NONE', *, *, #70743, .F. ) ;
#100281 = DIRECTION ( 'NONE',  ( 0.000000000000000000, 1.000000000000000000, 0.000000000000000000 ) ) ;
#100282 = EDGE_CURVE ( 'NONE', #40877, #76430, #12450, .T. ) ;
#100284 = CONICAL_SURFACE ( 'NONE', #102436, 0.09999999999999982514, 0.003490658503988666988 ) ;
#100283 = VECTOR ( 'NONE', #54664, 1000.000000000000000 ) ;
#100285 = DIRECTION ( 'NONE',  ( -4.274815082592931898E-19, -0.9999939076577903929, -0.003490651415223739937 ) ) ;
#100286 = CIRCLE ( 'NONE', #112810, 0.06509327318403745899 ) ;
#100287 = ORIENTED_EDGE ( 'NONE', *, *, #16331, .F. ) ;
#100288 = CARTESIAN_POINT ( 'NONE',  ( 10.64999999999990976, 2.500000000000000000, -6.941600689897077459 ) ) ;
#100289 = ADVANCED_FACE ( 'NONE', ( #90725 ), #109727, .F. ) ;
#100290 = ORIENTED_EDGE ( 'NONE', *, *, #97607, .T. ) ;
#100291 = FACE_BOUND ( 'NONE', #56484, .T. ) ;
#100292 = ADVANCED_FACE ( 'NONE', ( #89435 ), #75161, .T. ) ;
#100294 = AXIS2_PLACEMENT_3D ( 'NONE', #25225, #66450, #57939 ) ;
#100293 = AXIS2_PLACEMENT_3D ( 'NONE', #97960, #118248, #58690 ) ;
#100295 = ADVANCED_FACE ( 'NONE', ( #90064 ), #93944, .T. ) ;
#100296 = EDGE_CURVE ( 'NONE', #73598, #109355, #49525, .T. ) ;
#100297 = ORIENTED_EDGE ( 'NONE', *, *, #110866, .T. ) ;
#100298 = DIRECTION ( 'NONE',  ( 0.000000000000000000, 0.000000000000000000, 1.000000000000000000 ) ) ;
#100299 = CARTESIAN_POINT ( 'NONE',  ( 15.62915144542244583, 2.499999999999999556, -5.624002559040090610 ) ) ;
#100300 = ORIENTED_EDGE ( 'NONE', *, *, #36832, .F. ) ;
#100301 = ORIENTED_EDGE ( 'NONE', *, *, #45253, .F. ) ;
#100302 = DIRECTION ( 'NONE',  ( 0.000000000000000000, 1.000000000000000000, 0.000000000000000000 ) ) ;
#100303 = CARTESIAN_POINT ( 'NONE',  ( 11.89999999999990798, 2.500000000000000000, -4.676537180435977881 ) ) ;
#100304 = ORIENTED_EDGE ( 'NONE', *, *, #117221, .T. ) ;
#100305 = EDGE_CURVE ( 'NONE', #13873, #91647, #123278, .T. ) ;
#100306 = CARTESIAN_POINT ( 'NONE',  ( -5.000000000000022204, 12.50000000000000000, -0.6928203230275541413 ) ) ;
#100307 = CARTESIAN_POINT ( 'NONE',  ( 186.4843750003414016, -8.734944146203032389, -1.604583208406767949E-15 ) ) ;
#100308 = CARTESIAN_POINT ( 'NONE',  ( 4.599999999999936584, 2.500000000000000000, 3.637306695894644726 ) ) ;
#100309 = CARTESIAN_POINT ( 'NONE',  ( 103.5210970489751361, 8.410658075108495169, 2.246395211621319277 ) ) ;
#100310 = CARTESIAN_POINT ( 'NONE',  ( -5.400000000000020783, 12.50000000000000000, 5.022947341949748790 ) ) ;
#100311 = CARTESIAN_POINT ( 'NONE',  ( 4.999999999999973355, 12.50000000000000000, -4.330127018922201643 ) ) ;
#100312 = PLANE ( 'NONE',  #100603 ) ;
#100313 = VECTOR ( 'NONE', #21870, 1000.000000000000000 ) ;
#100314 = CIRCLE ( 'NONE', #27059, 0.09999999999999982514 ) ;
#100315 = ORIENTED_EDGE ( 'NONE', *, *, #56331, .T. ) ;
#100316 = EDGE_LOOP ( 'NONE', ( #67658, #40834, #102273, #53682 ) ) ;
#100317 = ORIENTED_EDGE ( 'NONE', *, *, #75095, .T. ) ;
#100318 = CARTESIAN_POINT ( 'NONE',  ( -10.84999999999999964, 12.50000000000000000, 7.188010851410848723 ) ) ;
#100319 = PLANE ( 'NONE',  #57493 ) ;
#100320 = CARTESIAN_POINT ( 'NONE',  ( 10.84999999999991260, 2.500000000000000000, 5.802370205355744659 ) ) ;
#100322 = ORIENTED_EDGE ( 'NONE', *, *, #15389, .T. ) ;
#100321 = EDGE_LOOP ( 'NONE', ( #46995, #88553 ) ) ;
#100323 = FACE_BOUND ( 'NONE', #118699, .T. ) ;
#100324 = VERTEX_POINT ( 'NONE', #21333 ) ;
#100325 = EDGE_CURVE ( 'NONE', #6598, #67150, #110360, .T. ) ;
#100326 = DIRECTION ( 'NONE',  ( 0.000000000000000000, 0.000000000000000000, 1.000000000000000000 ) ) ;
#100327 = CARTESIAN_POINT ( 'NONE',  ( -4.293440603042597559E-14, 2.500000000000000000, 5.022947341949748790 ) ) ;
#100328 = CIRCLE ( 'NONE', #31290, 0.09999999999999982514 ) ;
#100329 = CARTESIAN_POINT ( 'NONE',  ( -5.400000000000020783, 12.50000000000000000, 5.088040615133786027 ) ) ;
#100330 = CARTESIAN_POINT ( 'NONE',  ( -1.250000000000036193, 12.50000000000000000, 1.472243186433545459 ) ) ;
#100331 = CARTESIAN_POINT ( 'NONE',  ( -11.25000000000000000, 2.500000000000000000, -7.088010851410849966 ) ) ;
#100332 = DIRECTION ( 'NONE',  ( -0.000000000000000000, 1.000000000000000000, -0.000000000000000000 ) ) ;
#100333 = CARTESIAN_POINT ( 'NONE',  ( 13.94999999999989804, 12.50000000000000000, 1.753560074763284016 ) ) ;
#100334 = CARTESIAN_POINT ( 'NONE',  ( 11.64999999999990443, 2.500000000000000000, 1.472243186433545459 ) ) ;
#100335 = LINE ( 'NONE', #33536, #57959 ) ;
#100336 = CIRCLE ( 'NONE', #31390, 0.09999999999999982514 ) ;
#100337 = DIRECTION ( 'NONE',  ( 0.000000000000000000, 0.000000000000000000, 1.000000000000000000 ) ) ;
#100338 = ORIENTED_EDGE ( 'NONE', *, *, #24868, .F. ) ;
#100339 = EDGE_LOOP ( 'NONE', ( #36460, #84797, #77715, #40125 ) ) ;
#100340 = CIRCLE ( 'NONE', #43914, 0.09999999999999982514 ) ;
#100341 = EDGE_CURVE ( 'NONE', #118072, #107774, #112817, .T. ) ;
#100342 = ORIENTED_EDGE ( 'NONE', *, *, #17438, .F. ) ;
#100343 = ORIENTED_EDGE ( 'NONE', *, *, #39698, .T. ) ;
#100344 = MANIFOLD_SOLID_BREP ( 'Boss-Extrude2', #12224 ) ;
#100345 = CARTESIAN_POINT ( 'NONE',  ( -8.550000000000013145, 2.500000000000000000, -1.718653347947326049 ) ) ;
#100346 = DIRECTION ( 'NONE',  ( 0.000000000000000000, 1.000000000000000000, 0.000000000000000000 ) ) ;
#100348 = VERTEX_POINT ( 'NONE', #91367 ) ;
#100347 = EDGE_LOOP ( 'NONE', ( #99803, #5542 ) ) ;
#100349 = AXIS2_PLACEMENT_3D ( 'NONE', #77948, #118514, #87122 ) ;
#100350 = ORIENTED_EDGE ( 'NONE', *, *, #14133, .F. ) ;
#100351 = LINE ( 'NONE', #1486, #27101 ) ;
#100352 = VECTOR ( 'NONE', #15545, 1000.000000000000000 ) ;
#100353 = DIRECTION ( 'NONE',  ( 0.000000000000000000, 1.000000000000000000, 0.000000000000000000 ) ) ;
#100354 = CARTESIAN_POINT ( 'NONE',  ( 185.9166666666666856, 6.668395609140176816, 3.850000000000000977 ) ) ;
#100355 = DIRECTION ( 'NONE',  ( 0.000000000000000000, 1.000000000000000000, 0.000000000000000000 ) ) ;
#100356 = DIRECTION ( 'NONE',  ( 0.000000000000000000, 1.000000000000000000, 0.000000000000000000 ) ) ;
#100357 = AXIS2_PLACEMENT_3D ( 'NONE', #19646, #59595, #20930 ) ;
#100358 = DIRECTION ( 'NONE',  ( 0.000000000000000000, 0.000000000000000000, -1.000000000000000000 ) ) ;
#100359 = DIRECTION ( 'NONE',  ( 0.000000000000000000, 0.000000000000000000, -1.000000000000000000 ) ) ;
#100360 = ADVANCED_FACE ( 'NONE', ( #1685 ), #76180, .T. ) ;
#100361 = EDGE_LOOP ( 'NONE', ( #821, #87587 ) ) ;
#100362 = DIRECTION ( 'NONE',  ( 0.000000000000000000, 0.000000000000000000, 1.000000000000000000 ) ) ;
#100363 = VERTEX_POINT ( 'NONE', #50645 ) ;
#100364 = ORIENTED_EDGE ( 'NONE', *, *, #116746, .F. ) ;
#100365 = ORIENTED_EDGE ( 'NONE', *, *, #16541, .F. ) ;
#100366 = LINE ( 'NONE', #89887, #79859 ) ;
#100367 = EDGE_LOOP ( 'NONE', ( #53713, #127356, #114370, #100219 ) ) ;
#100368 = EDGE_LOOP ( 'NONE', ( #106361, #22422 ) ) ;
#100369 = CARTESIAN_POINT ( 'NONE',  ( 9.149999999999918643, 2.500000000000000000, -6.595190528383302109 ) ) ;
#100370 = DIRECTION ( 'NONE',  ( -0.000000000000000000, -1.000000000000000000, -0.000000000000000000 ) ) ;
#100371 = CARTESIAN_POINT ( 'NONE',  ( -2.100000000000034284, 2.500000000000000000, -4.330127018922201643 ) ) ;
#100372 = CARTESIAN_POINT ( 'NONE',  ( 13.09999999999990195, 2.500000000000000000, 3.983716857408420076 ) ) ;
#100373 = CARTESIAN_POINT ( 'NONE',  ( -12.09999999999999609, 2.500000000000000000, -5.022947341949751454 ) ) ;
#100374 = LINE ( 'NONE', #50619, #77594 ) ;
#100375 = LINE ( 'NONE', #90544, #51321 ) ;
#100376 = ORIENTED_EDGE ( 'NONE', *, *, #91979, .F. ) ;
#100377 = LINE ( 'NONE', #48708, #115217 ) ;
#100378 = EDGE_CURVE ( 'NONE', #50211, #54998, #120039, .T. ) ;
#100379 = VECTOR ( 'NONE', #31090, 1000.000000000000000 ) ;
#100380 = EDGE_LOOP ( 'NONE', ( #5083, #123326, #19001, #31622 ) ) ;
#100381 = CARTESIAN_POINT ( 'NONE',  ( -6.250000000000017764, 2.500000000000000000, 7.188010851410848723 ) ) ;
#100382 = CARTESIAN_POINT ( 'NONE',  ( -7.500000000000001776, 1.500000000000000000, 10.00000000000000178 ) ) ;
#100383 = ORIENTED_EDGE ( 'NONE', *, *, #51119, .F. ) ;
#100384 = FACE_OUTER_BOUND ( 'NONE', #106808, .T. ) ;
#100385 = DIRECTION ( 'NONE',  ( -0.000000000000000000, 1.000000000000000000, -0.000000000000000000 ) ) ;
#100386 = ORIENTED_EDGE ( 'NONE', *, *, #110150, .F. ) ;
#100387 = EDGE_CURVE ( 'NONE', #35157, #62991, #101686, .T. ) ;
#100388 = AXIS2_PLACEMENT_3D ( 'NONE', #57748, #38099, #55801 ) ;
#100389 = LINE ( 'NONE', #32321, #15398 ) ;
#100390 = ORIENTED_EDGE ( 'NONE', *, *, #4896, .F. ) ;
#100391 = EDGE_CURVE ( 'NONE', #38596, #89563, #33412, .T. ) ;
#100393 = ORIENTED_EDGE ( 'NONE', *, *, #77407, .F. ) ;
#100392 = EDGE_CURVE ( 'NONE', #88710, #61895, #243, .T. ) ;
#100394 = LINE ( 'NONE', #60488, #14281 ) ;
#100395 = DIRECTION ( 'NONE',  ( 0.000000000000000000, 0.000000000000000000, -1.000000000000000000 ) ) ;
#100396 = ADVANCED_FACE ( 'NONE', ( #69641 ), #83580, .T. ) ;
#100397 = DIRECTION ( 'NONE',  ( -4.274815082592931898E-19, -0.9999939076577903929, -0.003490651415223739937 ) ) ;
#100398 = ADVANCED_FACE ( 'NONE', ( #19234 ), #59195, .T. ) ;
#100399 = DIRECTION ( 'NONE',  ( 0.000000000000000000, 1.000000000000000000, 0.000000000000000000 ) ) ;
#100400 = DIRECTION ( 'NONE',  ( 0.000000000000000000, -0.000000000000000000, 1.000000000000000000 ) ) ;
#100401 = VERTEX_POINT ( 'NONE', #99759 ) ;
#100402 = DIRECTION ( 'NONE',  ( -0.000000000000000000, -1.000000000000000000, -0.000000000000000000 ) ) ;
#100403 = EDGE_CURVE ( 'NONE', #62801, #115200, #20549, .T. ) ;
#100404 = VERTEX_POINT ( 'NONE', #10692 ) ;
#100405 = EDGE_CURVE ( 'NONE', #26161, #63939, #90564, .T. ) ;
#100406 = DIRECTION ( 'NONE',  ( 0.000000000000000000, 0.000000000000000000, 1.000000000000000000 ) ) ;
#100407 = CIRCLE ( 'NONE', #58556, 0.1000000000000000472 ) ;
#100408 = DIRECTION ( 'NONE',  ( 0.000000000000000000, 0.000000000000000000, 1.000000000000000000 ) ) ;
#100409 = EDGE_CURVE ( 'NONE', #58364, #2839, #21181, .T. ) ;
#100410 = VECTOR ( 'NONE', #84053, 1000.000000000000000 ) ;
#100411 = CARTESIAN_POINT ( 'NONE',  ( 186.1302083336747444, -4.367472073101514418, -7.564683531250002702 ) ) ;
#100412 = DIRECTION ( 'NONE',  ( 0.000000000000000000, -0.000000000000000000, 1.000000000000000000 ) ) ;
#100413 = CARTESIAN_POINT ( 'NONE',  ( 2.299999999999948752, 2.500000000000000000, -3.883716857408426648 ) ) ;
#100414 = CARTESIAN_POINT ( 'NONE',  ( 8.149999999999920419, 12.50000000000000000, -1.753560074763288457 ) ) ;
#100415 = DIRECTION ( 'NONE',  ( 0.000000000000000000, -0.000000000000000000, 1.000000000000000000 ) ) ;
#100416 = ORIENTED_EDGE ( 'NONE', *, *, #23218, .T. ) ;
#100417 = VECTOR ( 'NONE', #10423, 1000.000000000000000 ) ;
#100418 = FACE_OUTER_BOUND ( 'NONE', #26956, .T. ) ;
#100419 = DIRECTION ( 'NONE',  ( -0.000000000000000000, -1.000000000000000000, -0.000000000000000000 ) ) ;
#100420 = DIRECTION ( 'NONE',  ( 0.000000000000000000, 0.000000000000000000, -1.000000000000000000 ) ) ;
#100421 = ORIENTED_EDGE ( 'NONE', *, *, #39860, .T. ) ;
#100422 = CARTESIAN_POINT ( 'NONE',  ( 2.499999999999947153, 2.500000000000000000, 0.6928203230275494784 ) ) ;
#100423 = CONICAL_SURFACE ( 'NONE', #115069, 0.1000000000000002554, 0.003490658503988666988 ) ;
#100424 = AXIS2_PLACEMENT_3D ( 'NONE', #29294, #98649, #9641 ) ;
#100425 = EDGE_LOOP ( 'NONE', ( #57139, #7633 ) ) ;
#100426 = VERTEX_POINT ( 'NONE', #103623 ) ;
#100427 = DIRECTION ( 'NONE',  ( -0.000000000000000000, -1.000000000000000000, -0.000000000000000000 ) ) ;
#100428 = ORIENTED_EDGE ( 'NONE', *, *, #61887, .T. ) ;
#100429 = DIRECTION ( 'NONE',  ( -4.274815082592931898E-19, -0.9999939076577903929, -0.003490651415223739937 ) ) ;
#100430 = CARTESIAN_POINT ( 'NONE',  ( 3.349999999999941913, 12.50000000000000000, 5.867463478539781896 ) ) ;
#100431 = VECTOR ( 'NONE', #128297, 1000.000000000000000 ) ;
#100432 = ORIENTED_EDGE ( 'NONE', *, *, #73518, .F. ) ;
#100433 = DIRECTION ( 'NONE',  ( 0.000000000000000000, 1.000000000000000000, 0.000000000000000000 ) ) ;
#100434 = DIRECTION ( 'NONE',  ( -0.000000000000000000, 1.000000000000000000, -0.000000000000000000 ) ) ;
#100435 = CONICAL_SURFACE ( 'NONE', #52405, 0.1000000000000002554, 0.003490658503988666988 ) ;
#100436 = PLANE ( 'NONE',  #2752 ) ;
#100437 = EDGE_CURVE ( 'NONE', #13897, #21869, #34895, .T. ) ;
#100438 = ORIENTED_EDGE ( 'NONE', *, *, #75443, .F. ) ;
#100439 = EDGE_CURVE ( 'NONE', #16079, #29645, #37696, .T. ) ;
#100440 = ORIENTED_EDGE ( 'NONE', *, *, #19721, .F. ) ;
#100441 = EDGE_CURVE ( 'NONE', #60185, #69366, #98221, .T. ) ;
#100442 = ORIENTED_EDGE ( 'NONE', *, *, #64801, .F. ) ;
#100443 = CARTESIAN_POINT ( 'NONE',  ( -15.39999999999997904, 2.500000000000000000, -0.6928203230275519209 ) ) ;
#100444 = CARTESIAN_POINT ( 'NONE',  ( 7.899999999999924860, 12.50000000000000000, -4.330127018922201643 ) ) ;
#100445 = CARTESIAN_POINT ( 'NONE',  ( 7.499999999999960032, 12.50000000000000000, -2.276824562219559311E-15 ) ) ;
#100446 = FACE_BOUND ( 'NONE', #14567, .T. ) ;
#100447 = ORIENTED_EDGE ( 'NONE', *, *, #2687, .F. ) ;
#100448 = DIRECTION ( 'NONE',  ( 0.000000000000000000, 0.000000000000000000, -1.000000000000000000 ) ) ;
#100449 = DIRECTION ( 'NONE',  ( -0.000000000000000000, 1.000000000000000000, -0.000000000000000000 ) ) ;
#100450 = ORIENTED_EDGE ( 'NONE', *, *, #119343, .T. ) ;
#100451 = ADVANCED_FACE ( 'NONE', ( #4107 ), #121208, .T. ) ;
#100452 = CARTESIAN_POINT ( 'NONE',  ( 15.83209681635555910, -1.499999999999999556, -5.404881881984147540 ) ) ;
#100453 = DIRECTION ( 'NONE',  ( -4.274815082592931898E-19, -0.9999939076577903929, -0.003490651415223739937 ) ) ;
#100455 = DIRECTION ( 'NONE',  ( 0.000000000000000000, 0.000000000000000000, -1.000000000000000000 ) ) ;
#100454 = VECTOR ( 'NONE', #98561, 1000.000000000000000 ) ;
#100456 = DIRECTION ( 'NONE',  ( 0.000000000000000000, 1.000000000000000000, 0.000000000000000000 ) ) ;
#100457 = DIRECTION ( 'NONE',  ( 0.000000000000000000, 1.000000000000000000, 0.000000000000000000 ) ) ;
#100458 = AXIS2_PLACEMENT_3D ( 'NONE', #6951, #44321, #66536 ) ;
#100459 = DIRECTION ( 'NONE',  ( 0.000000000000000000, 0.000000000000000000, 1.000000000000000000 ) ) ;
#100460 = FACE_OUTER_BOUND ( 'NONE', #68395, .T. ) ;
#100461 = AXIS2_PLACEMENT_3D ( 'NONE', #56453, #18469, #115354 ) ;
#100462 = ORIENTED_EDGE ( 'NONE', *, *, #40411, .T. ) ;
#100463 = EDGE_LOOP ( 'NONE', ( #119702, #36674 ) ) ;
#100464 = ORIENTED_EDGE ( 'NONE', *, *, #3427, .F. ) ;
#100465 = ORIENTED_EDGE ( 'NONE', *, *, #61078, .T. ) ;
#100466 = DIRECTION ( 'NONE',  ( 0.000000000000000000, 1.000000000000000000, 0.000000000000000000 ) ) ;
#100467 = CARTESIAN_POINT ( 'NONE',  ( 0.8499999999999557909, 2.500000000000000000, -6.395190528383301931 ) ) ;
#100468 = ORIENTED_EDGE ( 'NONE', *, *, #46480, .F. ) ;
#100469 = FACE_BOUND ( 'NONE', #96579, .T. ) ;
#100470 = EDGE_CURVE ( 'NONE', #34681, #76856, #83664, .T. ) ;
#100471 = CARTESIAN_POINT ( 'NONE',  ( 9.599999999999914380, 2.500000000000000000, 4.330127018922196314 ) ) ;
#100472 = FACE_OUTER_BOUND ( 'NONE', #61466, .T. ) ;
#100473 = CARTESIAN_POINT ( 'NONE',  ( 4.149999999999938183, 2.500000000000000000, 2.165063509461097713 ) ) ;
#100474 = DIRECTION ( 'NONE',  ( 0.000000000000000000, 1.000000000000000000, 0.000000000000000000 ) ) ;
#100475 = DIRECTION ( 'NONE',  ( 0.000000000000000000, 1.000000000000000000, 0.000000000000000000 ) ) ;
#100476 = CARTESIAN_POINT ( 'NONE',  ( -11.25000000000000178, 12.50000000000000000, -1.537336459617583584 ) ) ;
#100477 = DIRECTION ( 'NONE',  ( -0.000000000000000000, -1.000000000000000000, -0.000000000000000000 ) ) ;
#100478 = FACE_OUTER_BOUND ( 'NONE', #28669, .T. ) ;
#100479 = VERTEX_POINT ( 'NONE', #83959 ) ;
#100480 = ORIENTED_EDGE ( 'NONE', *, *, #21353, .T. ) ;
#100481 = EDGE_LOOP ( 'NONE', ( #34213, #12656 ) ) ;
#100482 = ORIENTED_EDGE ( 'NONE', *, *, #114716, .F. ) ;
#100483 = EDGE_CURVE ( 'NONE', #10045, #33882, #72238, .T. ) ;
#100484 = VERTEX_POINT ( 'NONE', #93163 ) ;
#100485 = EDGE_LOOP ( 'NONE', ( #74207, #29373, #74991, #44637 ) ) ;
#100486 = DIRECTION ( 'NONE',  ( -0.000000000000000000, -1.000000000000000000, -0.000000000000000000 ) ) ;
#100487 = ORIENTED_EDGE ( 'NONE', *, *, #123421, .F. ) ;
#100488 = AXIS2_PLACEMENT_3D ( 'NONE', #5870, #33437, #5239 ) ;
#100489 = CIRCLE ( 'NONE', #77417, 0.1000000000000002554 ) ;
#100490 = FACE_OUTER_BOUND ( 'NONE', #59909, .T. ) ;
#100491 = CARTESIAN_POINT ( 'NONE',  ( 184.1093750003413732, 9.264065473108010111E-16, -7.564683531250000925 ) ) ;
#100492 = DIRECTION ( 'NONE',  ( 0.000000000000000000, 0.000000000000000000, 1.000000000000000000 ) ) ;
#100493 = DIRECTION ( 'NONE',  ( 0.000000000000000000, -0.9999939076577903929, 0.003490651415223739937 ) ) ;
#100494 = EDGE_CURVE ( 'NONE', #39770, #6418, #14572, .T. ) ;
#100495 = ORIENTED_EDGE ( 'NONE', *, *, #127895, .T. ) ;
#100496 = DIRECTION ( 'NONE',  ( 0.000000000000000000, 1.000000000000000000, 0.000000000000000000 ) ) ;
#100497 = AXIS2_PLACEMENT_3D ( 'NONE', #29923, #40396, #20099 ) ;
#100498 = ORIENTED_EDGE ( 'NONE', *, *, #46641, .F. ) ;
#100499 = VERTEX_POINT ( 'NONE', #32326 ) ;
#100500 = CARTESIAN_POINT ( 'NONE',  ( -4.150000000000027889, 12.50000000000000000, -6.495190528383302464 ) ) ;
#100501 = CARTESIAN_POINT ( 'NONE',  ( 6.049999999999934097, 12.50000000000000000, -2.446380397790840266 ) ) ;
#100503 = ADVANCED_FACE ( 'NONE', ( #52575 ), #113433, .T. ) ;
#100502 = DIRECTION ( 'NONE',  ( 0.000000000000000000, 1.000000000000000000, 0.000000000000000000 ) ) ;
#100504 = EDGE_LOOP ( 'NONE', ( #47100, #40662, #115163, #37356 ) ) ;
#100505 = EDGE_LOOP ( 'NONE', ( #47688, #4104 ) ) ;
#100506 = CIRCLE ( 'NONE', #69198, 0.1000000000000000056 ) ;
#100507 = CARTESIAN_POINT ( 'NONE',  ( -1.650000000000035660, 2.500000000000000000, 2.757883832488649656 ) ) ;
#100508 = AXIS2_PLACEMENT_3D ( 'NONE', #11563, #10289, #72435 ) ;
#100509 = DIRECTION ( 'NONE',  ( 0.000000000000000000, 1.000000000000000000, 0.000000000000000000 ) ) ;
#100510 = FACE_OUTER_BOUND ( 'NONE', #9555, .T. ) ;
#100511 = CARTESIAN_POINT ( 'NONE',  ( -5.200000000000024158, 12.50000000000000000, -4.676537180435977881 ) ) ;
#100512 = EDGE_LOOP ( 'NONE', ( #88299, #68441, #67442, #88502 ) ) ;
#100513 = DIRECTION ( 'NONE',  ( -0.000000000000000000, -1.000000000000000000, -0.000000000000000000 ) ) ;
#100514 = VERTEX_POINT ( 'NONE', #53874 ) ;
#100515 = CARTESIAN_POINT ( 'NONE',  ( -2.700000000000029932, 2.500000000000000000, -4.576537180435977348 ) ) ;
#100516 = ORIENTED_EDGE ( 'NONE', *, *, #17635, .F. ) ;
#100517 = CARTESIAN_POINT ( 'NONE',  ( 87.50000000000001421, 3.974992050023849810, 6.359987280038159163 ) ) ;
#100518 = EDGE_CURVE ( 'NONE', #93018, #86595, #64774, .T. ) ;
#100519 = DIRECTION ( 'NONE',  ( 0.000000000000000000, 0.000000000000000000, 1.000000000000000000 ) ) ;
#100520 = AXIS2_PLACEMENT_3D ( 'NONE', #107706, #20620, #38999 ) ;
#100521 = FACE_OUTER_BOUND ( 'NONE', #44322, .T. ) ;
#100522 = DIRECTION ( 'NONE',  ( 0.000000000000000000, 0.000000000000000000, -1.000000000000000000 ) ) ;
#100523 = EDGE_LOOP ( 'NONE', ( #55962, #8801, #4196, #53572 ) ) ;
#100524 = EDGE_CURVE ( 'NONE', #99397, #72027, #79470, .T. ) ;
#100525 = DIRECTION ( 'NONE',  ( -0.000000000000000000, -1.000000000000000000, -0.000000000000000000 ) ) ;
#100526 = LINE ( 'NONE', #82192, #44478 ) ;
#100527 = ORIENTED_EDGE ( 'NONE', *, *, #83709, .T. ) ;
#100528 = ORIENTED_EDGE ( 'NONE', *, *, #115026, .F. ) ;
#100529 = EDGE_CURVE ( 'NONE', #5370, #50596, #33499, .T. ) ;
#100531 = VERTEX_POINT ( 'NONE', #102960 ) ;
#100530 = ADVANCED_FACE ( 'NONE', ( #64963 ), #94423, .T. ) ;
#100532 = DIRECTION ( 'NONE',  ( 0.000000000000000000, -0.9999939076577903929, 0.003490651415223739937 ) ) ;
#100533 = CARTESIAN_POINT ( 'NONE',  ( -13.14999999999999147, 2.500000000000000000, -1.818653347947323917 ) ) ;
#100534 = CARTESIAN_POINT ( 'NONE',  ( 19.95908882845300170, 2.629614671951224114, 2.273431397254408903 ) ) ;
#100535 = ADVANCED_FACE ( 'NONE', ( #64333 ), #46015, .T. ) ;
#100536 = DIRECTION ( 'NONE',  ( 0.000000000000000000, -0.9999939076577903929, 0.003490651415223739937 ) ) ;
#100537 = EDGE_CURVE ( 'NONE', #97073, #15146, #6270, .T. ) ;
#100538 = DIRECTION ( 'NONE',  ( -4.274815082592931898E-19, -0.9999939076577903929, -0.003490651415223739937 ) ) ;
#100539 = LINE ( 'NONE', #82201, #36096 ) ;
#100540 = CARTESIAN_POINT ( 'NONE',  ( -5.850000000000018296, 2.500000000000000000, 5.802370205355744659 ) ) ;
#100541 = FACE_OUTER_BOUND ( 'NONE', #104607, .T. ) ;
#100542 = DIRECTION ( 'NONE',  ( 0.000000000000000000, -0.9999939076577903929, 0.003490651415223739937 ) ) ;
#100543 = ADVANCED_FACE ( 'NONE', ( #92496 ), #27215, .T. ) ;
#100544 = VECTOR ( 'NONE', #30198, 1000.000000000000000 ) ;
#100545 = CIRCLE ( 'NONE', #121379, 0.06509327318403745899 ) ;
#100546 = CONICAL_SURFACE ( 'NONE', #50373, 0.09999999999999982514, 0.003490658503988666988 ) ;
#100547 = EDGE_CURVE ( 'NONE', #4391, #95241, #20959, .T. ) ;
#100548 = ADVANCED_FACE ( 'NONE', ( #63046 ), #112905, .T. ) ;
#100550 = ADVANCED_FACE ( 'NONE', ( #95086 ), #4219, .T. ) ;
#100549 = CIRCLE ( 'NONE', #52532, 0.1000000000000000472 ) ;
#100551 = ORIENTED_EDGE ( 'NONE', *, *, #25748, .F. ) ;
#100552 = DIRECTION ( 'NONE',  ( 0.000000000000000000, 0.000000000000000000, 1.000000000000000000 ) ) ;
#100553 = PLANE ( 'NONE',  #30763 ) ;
#100554 = DIRECTION ( 'NONE',  ( -0.000000000000000000, 1.000000000000000000, -0.000000000000000000 ) ) ;
#100555 = DIRECTION ( 'NONE',  ( 0.000000000000000000, 0.000000000000000000, 1.000000000000000000 ) ) ;
#100556 = EDGE_CURVE ( 'NONE', #85131, #118944, #117265, .T. ) ;
#100557 = ORIENTED_EDGE ( 'NONE', *, *, #100070, .T. ) ;
#100558 = CARTESIAN_POINT ( 'NONE',  ( -3.950000000000026379, 2.500000000000000000, -1.818653347947326138 ) ) ;
#100559 = DIRECTION ( 'NONE',  ( 0.000000000000000000, -0.000000000000000000, 1.000000000000000000 ) ) ;
#100561 = ORIENTED_EDGE ( 'NONE', *, *, #2421, .T. ) ;
#100560 = CARTESIAN_POINT ( 'NONE',  ( 6.899999999999926636, 2.500000000000000000, 0.2464101615137736789 ) ) ;
#100562 = EDGE_LOOP ( 'NONE', ( #47509, #88886, #81624, #113171 ) ) ;
#100563 = DIRECTION ( 'NONE',  ( 0.000000000000000000, 1.000000000000000000, 0.000000000000000000 ) ) ;
#100564 = VECTOR ( 'NONE', #125591, 1000.000000000000000 ) ;
#100565 = ORIENTED_EDGE ( 'NONE', *, *, #67555, .F. ) ;
#100566 = EDGE_LOOP ( 'NONE', ( #50636, #21144, #86585, #84016 ) ) ;
#100567 = DIRECTION ( 'NONE',  ( 0.000000000000000000, 0.000000000000000000, 1.000000000000000000 ) ) ;
#100568 = CARTESIAN_POINT ( 'NONE',  ( 18.78720903128162334, 2.539625591035298946, -4.564429507521253093 ) ) ;
#100569 = CARTESIAN_POINT ( 'NONE',  ( 12.49999999999993960, 12.50000000000000000, 4.330127018922196314 ) ) ;
#100570 = DIRECTION ( 'NONE',  ( 0.000000000000000000, 1.000000000000000000, 0.000000000000000000 ) ) ;
#100571 = AXIS2_PLACEMENT_3D ( 'NONE', #115169, #65444, #15691 ) ;
#100572 = EDGE_LOOP ( 'NONE', ( #17743, #66834 ) ) ;
#100573 = VECTOR ( 'NONE', #98568, 1000.000000000000000 ) ;
#100574 = CARTESIAN_POINT ( 'NONE',  ( 0.000000000000000000, 12.50000000000000000, 0.000000000000000000 ) ) ;
#100575 = VERTEX_POINT ( 'NONE', #36819 ) ;
#100576 = FACE_OUTER_BOUND ( 'NONE', #56032, .T. ) ;
#100577 = CARTESIAN_POINT ( 'NONE',  ( 16.56576425165006583, -1.500000000000000666, 6.084390597445813675 ) ) ;
#100578 = AXIS2_PLACEMENT_3D ( 'NONE', #27471, #67375, #5260 ) ;
#100579 = ORIENTED_EDGE ( 'NONE', *, *, #30011, .F. ) ;
#100580 = AXIS2_PLACEMENT_3D ( 'NONE', #39388, #79296, #119207 ) ;
#100581 = EDGE_CURVE ( 'NONE', #82804, #94907, #37610, .T. ) ;
#100582 = ORIENTED_EDGE ( 'NONE', *, *, #53653, .F. ) ;
#100584 = EDGE_CURVE ( 'NONE', #18587, #71296, #31351, .T. ) ;
#100583 = ORIENTED_EDGE ( 'NONE', *, *, #53993, .F. ) ;
#100585 = ORIENTED_EDGE ( 'NONE', *, *, #70945, .T. ) ;
#100586 = CARTESIAN_POINT ( 'NONE',  ( 9.149999999999918643, 12.50000000000000000, 2.165063509461097713 ) ) ;
#100587 = CARTESIAN_POINT ( 'NONE',  ( 10.63722763381497849, 2.499999999999999556, 8.014330155767298791 ) ) ;
#100588 = FACE_OUTER_BOUND ( 'NONE', #30819, .T. ) ;
#100589 = FACE_BOUND ( 'NONE', #100036, .T. ) ;
#100590 = DIRECTION ( 'NONE',  ( 0.000000000000000000, 0.000000000000000000, 1.000000000000000000 ) ) ;
#100591 = CARTESIAN_POINT ( 'NONE',  ( 186.6145833340161175, 6.668395609140177704, -3.849999999999998312 ) ) ;
#100592 = CARTESIAN_POINT ( 'NONE',  ( 9.199999999999915801, 2.500000000000000000, -4.430127018922202176 ) ) ;
#100593 = DIRECTION ( 'NONE',  ( 0.000000000000000000, 0.000000000000000000, 1.000000000000000000 ) ) ;
#100594 = AXIS2_PLACEMENT_3D ( 'NONE', #128113, #19429, #10272 ) ;
#100595 = EDGE_CURVE ( 'NONE', #104576, #76747, #75245, .T. ) ;
#100596 = AXIS2_PLACEMENT_3D ( 'NONE', #101737, #120093, #30439 ) ;
#100597 = CARTESIAN_POINT ( 'NONE',  ( -9.600000000000008527, 12.50000000000000000, -3.702399969078682851 ) ) ;
#100598 = FACE_OUTER_BOUND ( 'NONE', #59413, .T. ) ;
#100599 = DIRECTION ( 'NONE',  ( -0.000000000000000000, 1.000000000000000000, -0.000000000000000000 ) ) ;
#100600 = AXIS2_PLACEMENT_3D ( 'NONE', #43003, #1741, #111038 ) ;
#100601 = DIRECTION ( 'NONE',  ( -0.000000000000000000, 1.000000000000000000, -0.000000000000000000 ) ) ;
#100602 = ORIENTED_EDGE ( 'NONE', *, *, #72546, .T. ) ;
#100603 = AXIS2_PLACEMENT_3D ( 'NONE', #9992, #89833, #87246 ) ;
#100604 = ORIENTED_EDGE ( 'NONE', *, *, #43805, .F. ) ;
#100605 = VERTEX_POINT ( 'NONE', #117933 ) ;
#100606 = ORIENTED_EDGE ( 'NONE', *, *, #10657, .T. ) ;
#100607 = LINE ( 'NONE', #102545, #106671 ) ;
#100608 = CARTESIAN_POINT ( 'NONE',  ( -2.500000000000030642, 2.500000000000000000, -5.022947341949754119 ) ) ;
#100609 = ORIENTED_EDGE ( 'NONE', *, *, #107902, .F. ) ;
#100610 = FACE_BOUND ( 'NONE', #53970, .T. ) ;
#100611 = DIRECTION ( 'NONE',  ( 0.000000000000000000, 1.000000000000000000, 0.000000000000000000 ) ) ;
#100612 = ORIENTED_EDGE ( 'NONE', *, *, #71009, .F. ) ;
#100613 = DIRECTION ( 'NONE',  ( -4.274815082592931898E-19, -0.9999939076577903929, -0.003490651415223739937 ) ) ;
#100614 = CARTESIAN_POINT ( 'NONE',  ( -11.89999999999999503, 2.500000000000000000, 4.676537180435972552 ) ) ;
#100615 = FACE_OUTER_BOUND ( 'NONE', #74945, .T. ) ;
#100616 = DIRECTION ( 'NONE',  ( -0.000000000000000000, -1.000000000000000000, -0.000000000000000000 ) ) ;
#100617 = ORIENTED_EDGE ( 'NONE', *, *, #103965, .T. ) ;
#100618 = CARTESIAN_POINT ( 'NONE',  ( 9.199999999999915801, 2.500000000000000000, -4.230127018922201998 ) ) ;
#100619 = ADVANCED_FACE ( 'NONE', ( #66897 ), #85261, .T. ) ;
#100620 = ORIENTED_EDGE ( 'NONE', *, *, #47474, .T. ) ;
#100621 = CONICAL_SURFACE ( 'NONE', #44196, 0.09999999999999982514, 0.003490658503988666988 ) ;
#100622 = EDGE_LOOP ( 'NONE', ( #19652, #3312, #62795, #57814 ) ) ;
#100623 = DIRECTION ( 'NONE',  ( 0.000000000000000000, 0.000000000000000000, 1.000000000000000000 ) ) ;
#100624 = AXIS2_PLACEMENT_3D ( 'NONE', #64453, #3607, #104385 ) ;
#100625 = DIRECTION ( 'NONE',  ( 0.000000000000000000, 1.000000000000000000, 0.000000000000000000 ) ) ;
#100626 = ORIENTED_EDGE ( 'NONE', *, *, #79081, .F. ) ;
#100627 = DIRECTION ( 'NONE',  ( 0.000000000000000000, 1.000000000000000000, 0.000000000000000000 ) ) ;
#100628 = CARTESIAN_POINT ( 'NONE',  ( -7.300000000000018474, 2.500000000000000000, -3.983716857408426293 ) ) ;
#100629 = CIRCLE ( 'NONE', #117328, 0.06509327318403745899 ) ;
#100631 = VECTOR ( 'NONE', #98545, 1000.000000000000000 ) ;
#100630 = DIRECTION ( 'NONE',  ( -0.000000000000000000, -1.000000000000000000, -0.000000000000000000 ) ) ;
#100632 = DIRECTION ( 'NONE',  ( 0.000000000000000000, 0.000000000000000000, 1.000000000000000000 ) ) ;
#100633 = ORIENTED_EDGE ( 'NONE', *, *, #126097, .F. ) ;
#100635 = EDGE_CURVE ( 'NONE', #25412, #64421, #75429, .T. ) ;
#100634 = CONICAL_SURFACE ( 'NONE', #19060, 0.1000000000000002554, 0.003490658503988666988 ) ;
#100636 = EDGE_CURVE ( 'NONE', #57597, #66863, #35553, .T. ) ;
#100637 = DIRECTION ( 'NONE',  ( -0.000000000000000000, -1.000000000000000000, -0.000000000000000000 ) ) ;
#100638 = ORIENTED_EDGE ( 'NONE', *, *, #99814, .T. ) ;
#100639 = DIRECTION ( 'NONE',  ( 0.000000000000000000, 1.000000000000000000, 0.000000000000000000 ) ) ;
#100640 = EDGE_LOOP ( 'NONE', ( #10681, #68197, #4392, #67115 ) ) ;
#100641 = DIRECTION ( 'NONE',  ( -0.000000000000000000, 1.000000000000000000, -0.000000000000000000 ) ) ;
#100642 = EDGE_LOOP ( 'NONE', ( #112431, #27969, #1227, #78824 ) ) ;
#100643 = FACE_OUTER_BOUND ( 'NONE', #25786, .T. ) ;
#100644 = DIRECTION ( 'NONE',  ( 0.000000000000000000, 0.000000000000000000, -1.000000000000000000 ) ) ;
#100645 = DIRECTION ( 'NONE',  ( 0.000000000000000000, 1.000000000000000000, 0.000000000000000000 ) ) ;
#100647 = EDGE_CURVE ( 'NONE', #89951, #17587, #105554, .T. ) ;
#100646 = LINE ( 'NONE', #111099, #11115 ) ;
#100648 = FACE_OUTER_BOUND ( 'NONE', #123619, .T. ) ;
#100649 = ORIENTED_EDGE ( 'NONE', *, *, #8198, .F. ) ;
#100650 = ORIENTED_EDGE ( 'NONE', *, *, #31802, .T. ) ;
#100651 = ORIENTED_EDGE ( 'NONE', *, *, #117105, .T. ) ;
#100652 = FACE_OUTER_BOUND ( 'NONE', #1773, .T. ) ;
#100653 = CARTESIAN_POINT ( 'NONE',  ( 14.79999999999989235, 2.500000000000000000, 0.2464101615137735679 ) ) ;
#100654 = FACE_OUTER_BOUND ( 'NONE', #96715, .T. ) ;
#100656 = ORIENTED_EDGE ( 'NONE', *, *, #58889, .T. ) ;
#100655 = ORIENTED_EDGE ( 'NONE', *, *, #68965, .T. ) ;
#100657 = EDGE_LOOP ( 'NONE', ( #24289, #97951, #47478, #113724 ) ) ;
#100658 = CARTESIAN_POINT ( 'NONE',  ( 4.799999999999935874, 12.50000000000000000, 0.3464101615137735735 ) ) ;
#100660 = ORIENTED_EDGE ( 'NONE', *, *, #39862, .F. ) ;
#100659 = CONICAL_SURFACE ( 'NONE', #67188, 0.1000000000000000472, 0.003490658503988666988 ) ;
#100661 = CARTESIAN_POINT ( 'NONE',  ( 7.499999999999927169, 2.500000000000000000, 3.537306695894645081 ) ) ;
#100662 = CONICAL_SURFACE ( 'NONE', #63027, 0.1000000000000000472, 0.003490658503988666988 ) ;
#100663 = PLANE ( 'NONE',  #120068 ) ;
#100664 = CARTESIAN_POINT ( 'NONE',  ( 2.499999999999947153, 2.500000000000000000, -3.537306695894649966 ) ) ;
#100665 = LINE ( 'NONE', #69940, #17229 ) ;
#100666 = DIRECTION ( 'NONE',  ( 0.000000000000000000, -0.9999939076577903929, 0.003490651415223739937 ) ) ;
#100667 = DIRECTION ( 'NONE',  ( -0.000000000000000000, 1.000000000000000000, -0.000000000000000000 ) ) ;
#100669 = AXIS2_PLACEMENT_3D ( 'NONE', #50357, #80485, #120393 ) ;
#100668 = DIRECTION ( 'NONE',  ( 0.000000000000000000, 1.000000000000000000, 0.000000000000000000 ) ) ;
#100670 = ORIENTED_EDGE ( 'NONE', *, *, #56087, .F. ) ;
#100671 = CIRCLE ( 'NONE', #75539, 0.06509327318403745899 ) ;
#100672 = EDGE_LOOP ( 'NONE', ( #44184, #126579, #129444, #87475 ) ) ;
#100673 = EDGE_CURVE ( 'NONE', #59628, #77485, #39767, .T. ) ;
#100674 = LINE ( 'NONE', #11003, #25737 ) ;
#100675 = CONICAL_SURFACE ( 'NONE', #54692, 0.1000000000000000472, 0.003490658503988666988 ) ;
#100676 = DIRECTION ( 'NONE',  ( 0.000000000000000000, 1.000000000000000000, 0.000000000000000000 ) ) ;
#100677 = VERTEX_POINT ( 'NONE', #115337 ) ;
#100678 = ORIENTED_EDGE ( 'NONE', *, *, #108921, .T. ) ;
#100679 = ADVANCED_FACE ( 'NONE', ( #65615 ), #52269, .T. ) ;
#100680 = CARTESIAN_POINT ( 'NONE',  ( 185.3593750003413732, 0.000000000000000000, 7.564683531250000925 ) ) ;
#100681 = DIRECTION ( 'NONE',  ( 0.000000000000000000, 0.000000000000000000, 1.000000000000000000 ) ) ;
#100682 = DIRECTION ( 'NONE',  ( 0.000000000000000000, -0.000000000000000000, 1.000000000000000000 ) ) ;
#100683 = EDGE_CURVE ( 'NONE', #114828, #26322, #37466, .T. ) ;
#100684 = AXIS2_PLACEMENT_3D ( 'NONE', #92697, #33144, #73060 ) ;
#100685 = CARTESIAN_POINT ( 'NONE',  ( 1.249999999999988454, 2.500000000000000000, 2.065063509461097624 ) ) ;
#100686 = DIRECTION ( 'NONE',  ( -4.274815082592931898E-19, -0.9999939076577903929, -0.003490651415223739937 ) ) ;
#100687 = FACE_OUTER_BOUND ( 'NONE', #128374, .T. ) ;
#100688 = DIRECTION ( 'NONE',  ( 0.000000000000000000, -0.000000000000000000, 1.000000000000000000 ) ) ;
#100689 = VECTOR ( 'NONE', #12807, 1000.000000000000000 ) ;
#100690 = DIRECTION ( 'NONE',  ( -4.274815082592931898E-19, -0.9999939076577903929, -0.003490651415223739937 ) ) ;
#100691 = EDGE_CURVE ( 'NONE', #4868, #11053, #12537, .T. ) ;
#100692 = EDGE_CURVE ( 'NONE', #37929, #56654, #102444, .T. ) ;
#100693 = EDGE_CURVE ( 'NONE', #109444, #16630, #119157, .T. ) ;
#100694 = VECTOR ( 'NONE', #67761, 1000.000000000000000 ) ;
#100695 = DIRECTION ( 'NONE',  ( 0.000000000000000000, 0.000000000000000000, 1.000000000000000000 ) ) ;
#100696 = ORIENTED_EDGE ( 'NONE', *, *, #55447, .T. ) ;
#100697 = ORIENTED_EDGE ( 'NONE', *, *, #33018, .F. ) ;
#100698 = EDGE_CURVE ( 'NONE', #127171, #27644, #94120, .T. ) ;
#100699 = AXIS2_PLACEMENT_3D ( 'NONE', #35441, #16400, #26901 ) ;
#100700 = VERTEX_POINT ( 'NONE', #17797 ) ;
#100701 = ORIENTED_EDGE ( 'NONE', *, *, #65683, .F. ) ;
#100702 = EDGE_LOOP ( 'NONE', ( #44294, #32074 ) ) ;
#100703 = DIRECTION ( 'NONE',  ( 0.000000000000000000, 0.000000000000000000, 1.000000000000000000 ) ) ;
#100704 = DIRECTION ( 'NONE',  ( 0.000000000000000000, 0.000000000000000000, 1.000000000000000000 ) ) ;
#100705 = ADVANCED_FACE ( 'NONE', ( #6040 ), #77113, .T. ) ;
#100706 = EDGE_LOOP ( 'NONE', ( #50602, #22030, #4979, #115040 ) ) ;
#100707 = LINE ( 'NONE', #79168, #29826 ) ;
#100708 = CARTESIAN_POINT ( 'NONE',  ( 186.0312500006828031, 9.429780353434619030E-16, -7.700000000000000178 ) ) ;
#100709 = CARTESIAN_POINT ( 'NONE',  ( -14.39999999999998614, 12.50000000000000000, 0.3464101615137758494 ) ) ;
#100711 = ORIENTED_EDGE ( 'NONE', *, *, #3997, .F. ) ;
#100710 = CARTESIAN_POINT ( 'NONE',  ( -8.100000000000010303, 12.50000000000000000, 4.611443907251934426 ) ) ;
#100712 = DIRECTION ( 'NONE',  ( -0.000000000000000000, 1.000000000000000000, -0.000000000000000000 ) ) ;
#100713 = DIRECTION ( 'NONE',  ( 0.000000000000000000, 0.000000000000000000, -1.000000000000000000 ) ) ;
#100714 = VERTEX_POINT ( 'NONE', #104882 ) ;
#100715 = ORIENTED_EDGE ( 'NONE', *, *, #47438, .F. ) ;
#100716 = ORIENTED_EDGE ( 'NONE', *, *, #107308, .T. ) ;
#100717 = CIRCLE ( 'NONE', #10816, 0.06509327318403745899 ) ;
#100718 = VERTEX_POINT ( 'NONE', #15203 ) ;
#100719 = FACE_OUTER_BOUND ( 'NONE', #56037, .T. ) ;
#100720 = CONICAL_SURFACE ( 'NONE', #61015, 0.1000000000000000472, 0.003490658503988666988 ) ;
#100721 = AXIS2_PLACEMENT_3D ( 'NONE', #60470, #111466, #19883 ) ;
#100722 = LINE ( 'NONE', #119721, #61338 ) ;
#100723 = CARTESIAN_POINT ( 'NONE',  ( 1.849999999999949685, 2.500000000000000000, 1.918653347947321564 ) ) ;
#100724 = AXIS2_PLACEMENT_3D ( 'NONE', #93835, #14603, #44085 ) ;
#100725 = CARTESIAN_POINT ( 'NONE',  ( 4.149999999999939959, 2.500000000000000000, -6.595190528383302109 ) ) ;
#100727 = ORIENTED_EDGE ( 'NONE', *, *, #108506, .F. ) ;
#100726 = AXIS2_PLACEMENT_3D ( 'NONE', #61870, #102429, #70388 ) ;
#100728 = CARTESIAN_POINT ( 'NONE',  ( 9.599999999999914380, 12.50000000000000000, -3.702399969078687292 ) ) ;
#100729 = FACE_OUTER_BOUND ( 'NONE', #57598, .T. ) ;
#100730 = CARTESIAN_POINT ( 'NONE',  ( -11.84999999999999609, 12.50000000000000000, 2.511473670974873507 ) ) ;
#100731 = DIRECTION ( 'NONE',  ( 0.000000000000000000, 1.000000000000000000, 0.000000000000000000 ) ) ;
#100732 = AXIS2_PLACEMENT_3D ( 'NONE', #14781, #54728, #94656 ) ;
#100733 = EDGE_LOOP ( 'NONE', ( #27991, #110308, #65743, #12202 ) ) ;
#100734 = EDGE_CURVE ( 'NONE', #61946, #19850, #45995, .T. ) ;
#100735 = VERTEX_POINT ( 'NONE', #9281 ) ;
#100736 = ORIENTED_EDGE ( 'NONE', *, *, #119899, .F. ) ;
#100737 = LINE ( 'NONE', #102050, #72775 ) ;
#100738 = DIRECTION ( 'NONE',  ( 0.000000000000000000, -0.9999939076577903929, 0.003490651415223739937 ) ) ;
#100739 = FACE_BOUND ( 'NONE', #75450, .T. ) ;
#100740 = LINE ( 'NONE', #18319, #7411 ) ;
#100741 = CARTESIAN_POINT ( 'NONE',  ( 3.349999999999943689, 2.500000000000000000, 2.265063509461097357 ) ) ;
#100742 = FACE_OUTER_BOUND ( 'NONE', #53152, .T. ) ;
#100743 = EDGE_CURVE ( 'NONE', #112572, #44266, #19074, .T. ) ;
#100744 = DIRECTION ( 'NONE',  ( 0.000000000000000000, 0.000000000000000000, 1.000000000000000000 ) ) ;
#100745 = DIRECTION ( 'NONE',  ( 0.000000000000000000, 1.000000000000000000, 0.000000000000000000 ) ) ;
#100746 = DIRECTION ( 'NONE',  ( 0.000000000000000000, 0.000000000000000000, 1.000000000000000000 ) ) ;
#100747 = ORIENTED_EDGE ( 'NONE', *, *, #86199, .F. ) ;
#100748 = AXIS2_PLACEMENT_3D ( 'NONE', #67869, #65936, #128094 ) ;
#100749 = DIRECTION ( 'NONE',  ( 0.000000000000000000, 1.000000000000000000, 0.000000000000000000 ) ) ;
#100750 = CARTESIAN_POINT ( 'NONE',  ( -3.150000000000029221, 2.500000000000000000, 2.611473670974873151 ) ) ;
#100751 = VERTEX_POINT ( 'NONE', #59027 ) ;
#100752 = ORIENTED_EDGE ( 'NONE', *, *, #46817, .T. ) ;
#100753 = DIRECTION ( 'NONE',  ( 0.000000000000000000, 0.000000000000000000, 1.000000000000000000 ) ) ;
#100754 = DIRECTION ( 'NONE',  ( 0.000000000000000000, 1.000000000000000000, 0.000000000000000000 ) ) ;
#100755 = FACE_BOUND ( 'NONE', #2460, .T. ) ;
#100756 = CIRCLE ( 'NONE', #8813, 0.06509327318403745899 ) ;
#100757 = FACE_OUTER_BOUND ( 'NONE', #56754, .T. ) ;
#100758 = CIRCLE ( 'NONE', #56834, 0.09999999999999982514 ) ;
#100759 = VECTOR ( 'NONE', #13921, 1000.000000000000000 ) ;
#100761 = DIRECTION ( 'NONE',  ( -0.000000000000000000, 1.000000000000000000, -0.000000000000000000 ) ) ;
#100760 = CIRCLE ( 'NONE', #67293, 0.06509327318403745899 ) ;
#100762 = VERTEX_POINT ( 'NONE', #58397 ) ;
#100763 = DIRECTION ( 'NONE',  ( 0.000000000000000000, -0.9999939076577903929, 0.003490651415223739937 ) ) ;
#100764 = DIRECTION ( 'NONE',  ( 0.000000000000000000, 1.000000000000000000, 0.000000000000000000 ) ) ;
#100765 = ORIENTED_EDGE ( 'NONE', *, *, #66567, .T. ) ;
#100767 = DIRECTION ( 'NONE',  ( 0.000000000000000000, 1.000000000000000000, 0.000000000000000000 ) ) ;
#100766 = AXIS2_PLACEMENT_3D ( 'NONE', #110880, #113299, #124422 ) ;
#100768 = DIRECTION ( 'NONE',  ( 0.000000000000000000, 0.000000000000000000, -1.000000000000000000 ) ) ;
#100769 = ADVANCED_FACE ( 'NONE', ( #48566 ), #70851, .T. ) ;
#100770 = CIRCLE ( 'NONE', #104889, 0.06509327318403745899 ) ;
#100771 = AXIS2_PLACEMENT_3D ( 'NONE', #36791, #117896, #107443 ) ;
#100772 = AXIS2_PLACEMENT_3D ( 'NONE', #68773, #109345, #29506 ) ;
#100773 = CARTESIAN_POINT ( 'NONE',  ( -8.750000000000010658, 2.500000000000000000, -7.188010851410848723 ) ) ;
#100774 = DIRECTION ( 'NONE',  ( 1.000000000000000000, -0.000000000000000000, -0.000000000000000000 ) ) ;
#100775 = AXIS2_PLACEMENT_3D ( 'NONE', #70669, #19647, #631 ) ;
#100776 = EDGE_CURVE ( 'NONE', #111375, #36539, #69474, .T. ) ;
#100777 = EDGE_LOOP ( 'NONE', ( #1821, #26117 ) ) ;
#100778 = CARTESIAN_POINT ( 'NONE',  ( 4.999999999999969802, 2.500000000000000000, 4.230127018922196669 ) ) ;
#100779 = CIRCLE ( 'NONE', #94535, 0.06509327318403745899 ) ;
#100780 = CARTESIAN_POINT ( 'NONE',  ( -8.150000000000014566, 2.500000000000000000, -6.148780366869520897 ) ) ;
#100781 = CARTESIAN_POINT ( 'NONE',  ( 6.249999999999967137, 12.50000000000000000, -2.165063509461101710 ) ) ;
#100782 = VERTEX_POINT ( 'NONE', #98949 ) ;
#100783 = EDGE_CURVE ( 'NONE', #7958, #46669, #72910, .T. ) ;
#100784 = ORIENTED_EDGE ( 'NONE', *, *, #21025, .T. ) ;
#100785 = ADVANCED_FACE ( 'NONE', ( #89127 ), #43688, .T. ) ;
#100786 = CARTESIAN_POINT ( 'NONE',  ( -8.300000000000011369, 12.50000000000000000, -2.276824562219559311E-15 ) ) ;
#100787 = EDGE_LOOP ( 'NONE', ( #4822, #28527, #66636, #15007 ) ) ;
#100788 = CARTESIAN_POINT ( 'NONE',  ( -1.050000000000038680, 12.50000000000000000, 2.446380397790835826 ) ) ;
#100789 = CARTESIAN_POINT ( 'NONE',  ( 0.5999999999999547917, 2.500000000000000000, 3.983716857408420076 ) ) ;
#100790 = DIRECTION ( 'NONE',  ( -0.000000000000000000, -1.000000000000000000, -0.000000000000000000 ) ) ;
#100791 = ORIENTED_EDGE ( 'NONE', *, *, #57497, .T. ) ;
#100792 = ADVANCED_FACE ( 'NONE', ( #81248 ), #88469, .T. ) ;
#100793 = LINE ( 'NONE', #3894, #1507 ) ;
#100794 = DIRECTION ( 'NONE',  ( -0.000000000000000000, 1.000000000000000000, -0.000000000000000000 ) ) ;
#100795 = CARTESIAN_POINT ( 'NONE',  ( 9.399999999999915090, 2.500000000000000000, 4.576537180435972019 ) ) ;
#100796 = DIRECTION ( 'NONE',  ( -0.000000000000000000, -1.000000000000000000, -0.000000000000000000 ) ) ;
#100797 = DIRECTION ( 'NONE',  ( 0.000000000000000000, 0.000000000000000000, -1.000000000000000000 ) ) ;
#100798 = ADVANCED_FACE ( 'NONE', ( #128435 ), #28934, .T. ) ;
#100799 = CARTESIAN_POINT ( 'NONE',  ( -8.550000000000013145, 12.50000000000000000, -6.841600689897073373 ) ) ;
#100800 = ORIENTED_EDGE ( 'NONE', *, *, #67572, .T. ) ;
#100801 = ORIENTED_EDGE ( 'NONE', *, *, #87201, .F. ) ;
#100802 = DIRECTION ( 'NONE',  ( -4.274815082592931898E-19, -0.9999939076577903929, -0.003490651415223739937 ) ) ;
#100803 = ORIENTED_EDGE ( 'NONE', *, *, #68865, .T. ) ;
#100804 = CIRCLE ( 'NONE', #75671, 0.1000000000000002554 ) ;
#100805 = CARTESIAN_POINT ( 'NONE',  ( 103.5362392592695642, 7.362830575048670667, 2.258572230843124196 ) ) ;
#100806 = VECTOR ( 'NONE', #21048, 1000.000000000000000 ) ;
#100807 = CIRCLE ( 'NONE', #452, 0.1000000000000002554 ) ;
#100809 = EDGE_LOOP ( 'NONE', ( #85554, #5981 ) ) ;
#100808 = ORIENTED_EDGE ( 'NONE', *, *, #113504, .T. ) ;
#100810 = VERTEX_POINT ( 'NONE', #110062 ) ;
#100811 = DIRECTION ( 'NONE',  ( 0.000000000000000000, 1.000000000000000000, 0.000000000000000000 ) ) ;
#100812 = CARTESIAN_POINT ( 'NONE',  ( 7.699999999999922018, 12.50000000000000000, 0.3464101615137735735 ) ) ;
#100814 = CARTESIAN_POINT ( 'NONE',  ( 3.949999999999940670, 12.50000000000000000, 1.753560074763284016 ) ) ;
#100813 = VECTOR ( 'NONE', #72706, 1000.000000000000000 ) ;
#100815 = CIRCLE ( 'NONE', #102866, 0.09999999999999999167 ) ;
#100816 = FILL_AREA_STYLE_COLOUR ( '', #41524 ) ;
#100817 = CARTESIAN_POINT ( 'NONE',  ( 7.049999999999928768, 12.50000000000000000, 6.430097255199259010 ) ) ;
#100818 = CARTESIAN_POINT ( 'NONE',  ( -9.350000000000006750, 12.50000000000000000, 1.753560074763284016 ) ) ;
#100819 = DIRECTION ( 'NONE',  ( 0.000000000000000000, 0.000000000000000000, 1.000000000000000000 ) ) ;
#100820 = AXIS2_PLACEMENT_3D ( 'NONE', #53972, #53340, #73597 ) ;
#100821 = DIRECTION ( 'NONE',  ( 0.000000000000000000, 0.000000000000000000, 1.000000000000000000 ) ) ;
#100822 = LINE ( 'NONE', #28890, #109308 ) ;
#100823 = AXIS2_PLACEMENT_3D ( 'NONE', #119035, #107917, #58195 ) ;
#100824 = DIRECTION ( 'NONE',  ( 0.000000000000000000, 0.000000000000000000, 1.000000000000000000 ) ) ;
#100825 = VECTOR ( 'NONE', #1846, 1000.000000000000000 ) ;
#100826 = ORIENTED_EDGE ( 'NONE', *, *, #115570, .T. ) ;
#100827 = EDGE_CURVE ( 'NONE', #119283, #109616, #95986, .T. ) ;
#100828 = DIRECTION ( 'NONE',  ( 0.000000000000000000, 0.000000000000000000, 1.000000000000000000 ) ) ;
#100829 = ORIENTED_EDGE ( 'NONE', *, *, #650, .T. ) ;
#100830 = VERTEX_POINT ( 'NONE', #109408 ) ;
#100831 = LINE ( 'NONE', #121134, #73349 ) ;
#100832 = CARTESIAN_POINT ( 'NONE',  ( -4.600000000000025402, 2.500000000000000000, 4.230127018922196669 ) ) ;
#100833 = ADVANCED_FACE ( 'NONE', ( #121163 ), #37418, .T. ) ;
#100834 = AXIS2_PLACEMENT_3D ( 'NONE', #56760, #96695, #86885 ) ;
#100835 = FACE_OUTER_BOUND ( 'NONE', #86552, .T. ) ;
#100836 = CARTESIAN_POINT ( 'NONE',  ( 6.249999999999968914, 12.50000000000000000, -6.495190528383302464 ) ) ;
#100837 = DIRECTION ( 'NONE',  ( 0.000000000000000000, 0.000000000000000000, -1.000000000000000000 ) ) ;
#100838 = DIRECTION ( 'NONE',  ( -4.274815082592931898E-19, -0.9999939076577903929, -0.003490651415223739937 ) ) ;
#100839 = VERTEX_POINT ( 'NONE', #9921 ) ;
#100840 = ADVANCED_FACE ( 'NONE', ( #60334 ), #31164, .T. ) ;
#100841 = ADVANCED_FACE ( 'NONE', ( #30230 ), #112714, .T. ) ;
#100842 = EDGE_CURVE ( 'NONE', #108104, #79172, #91775, .T. ) ;
#100843 = CIRCLE ( 'NONE', #36020, 0.06509327318403745899 ) ;
#100844 = VERTEX_POINT ( 'NONE', #30872 ) ;
#100845 = CARTESIAN_POINT ( 'NONE',  ( 13.34999999999990017, 2.500000000000000000, 2.165063509461097713 ) ) ;
#100846 = CIRCLE ( 'NONE', #128056, 0.06509327318403745899 ) ;
#100847 = EDGE_LOOP ( 'NONE', ( #129469, #50699, #87184, #13387 ) ) ;
#100848 = DIRECTION ( 'NONE',  ( 0.000000000000000000, 1.000000000000000000, 0.000000000000000000 ) ) ;
#100849 = ADVANCED_FACE ( 'NONE', ( #10547 ), #116809, .T. ) ;
#100850 = EDGE_LOOP ( 'NONE', ( #56872, #2637 ) ) ;
#100851 = VERTEX_POINT ( 'NONE', #100866 ) ;
#100852 = AXIS2_PLACEMENT_3D ( 'NONE', #19278, #79517, #119414 ) ;
#100853 = FACE_OUTER_BOUND ( 'NONE', #603, .T. ) ;
#100854 = CARTESIAN_POINT ( 'NONE',  ( 6.649999999999931966, 2.500000000000000000, -5.802370205355749988 ) ) ;
#100855 = CIRCLE ( 'NONE', #98702, 0.06509327318403745899 ) ;
#100856 = EDGE_CURVE ( 'NONE', #850, #116295, #51151, .T. ) ;
#100857 = CIRCLE ( 'NONE', #2650, 0.09999999999999999167 ) ;
#100858 = ADVANCED_FACE ( 'NONE', ( #108116 ), #121024, .T. ) ;
#100859 = CARTESIAN_POINT ( 'NONE',  ( -13.29999999999999005, 12.50000000000000000, -4.330127018922198978 ) ) ;
#100860 = CONICAL_SURFACE ( 'NONE', #90388, 0.1000000000000000056, 0.003490658503988666988 ) ;
#100861 = DIRECTION ( 'NONE',  ( 0.000000000000000000, 0.000000000000000000, 1.000000000000000000 ) ) ;
#100862 = LINE ( 'NONE', #120521, #20018 ) ;
#100863 = EDGE_LOOP ( 'NONE', ( #57301, #116377 ) ) ;
#100864 = DIRECTION ( 'NONE',  ( -0.000000000000000000, 1.000000000000000000, -0.000000000000000000 ) ) ;
#100865 = DIRECTION ( 'NONE',  ( 0.000000000000000000, 1.000000000000000000, 0.000000000000000000 ) ) ;
#100866 = CARTESIAN_POINT ( 'NONE',  ( -3.150000000000030109, 2.500000000000000000, -2.411473670974877859 ) ) ;
#100867 = CARTESIAN_POINT ( 'NONE',  ( -2.300000000000033573, 12.50000000000000000, 0.2813168883297361700 ) ) ;
#100868 = AXIS2_PLACEMENT_3D ( 'NONE', #102055, #63416, #12373 ) ;
#100869 = AXIS2_PLACEMENT_3D ( 'NONE', #117168, #37366, #128328 ) ;
#100870 = CARTESIAN_POINT ( 'NONE',  ( -3.100000000000028955, 12.50000000000000000, 4.676537180435972552 ) ) ;
#100871 = VERTEX_POINT ( 'NONE', #102795 ) ;
#100872 = VECTOR ( 'NONE', #32117, 1000.000000000000000 ) ;
#100873 = CIRCLE ( 'NONE', #98820, 0.06509327318403745899 ) ;
#100874 = ORIENTED_EDGE ( 'NONE', *, *, #29573, .T. ) ;
#100875 = ORIENTED_EDGE ( 'NONE', *, *, #41140, .T. ) ;
#100876 = CARTESIAN_POINT ( 'NONE',  ( -7.950000000000012612, 2.500000000000000000, 2.265063509461097357 ) ) ;
#100877 = CIRCLE ( 'NONE', #17238, 0.06509327318403745899 ) ;
#100878 = VERTEX_POINT ( 'NONE', #11843 ) ;
#100879 = CARTESIAN_POINT ( 'NONE',  ( 17.50000000000011369, -2.362783583790017961, 3.757116699120848669 ) ) ;
#100880 = FACE_OUTER_BOUND ( 'NONE', #113195, .T. ) ;
#100881 = AXIS2_PLACEMENT_3D ( 'NONE', #16251, #115094, #14325 ) ;
#100882 = ORIENTED_EDGE ( 'NONE', *, *, #31858, .T. ) ;
#100883 = CARTESIAN_POINT ( 'NONE',  ( 184.0416666666666572, -4.445597072760122614, 7.699999999999998401 ) ) ;
#100884 = DIRECTION ( 'NONE',  ( -0.000000000000000000, 1.000000000000000000, -0.000000000000000000 ) ) ;
#100885 = DIRECTION ( 'NONE',  ( 0.000000000000000000, 1.000000000000000000, 0.000000000000000000 ) ) ;
#100886 = CARTESIAN_POINT ( 'NONE',  ( 8.549999999999922551, 2.500000000000000000, -6.148780366869526226 ) ) ;
#100887 = DIRECTION ( 'NONE',  ( 0.000000000000000000, 0.000000000000000000, 1.000000000000000000 ) ) ;
#100888 = EDGE_LOOP ( 'NONE', ( #80323, #26983, #118790, #37886 ) ) ;
#100889 = AXIS2_PLACEMENT_3D ( 'NONE', #80600, #21018, #100861 ) ;
#100890 = CARTESIAN_POINT ( 'NONE',  ( 2.499999999999948930, 2.500000000000000000, -5.022947341949754119 ) ) ;
#100891 = DIRECTION ( 'NONE',  ( 0.000000000000000000, 1.000000000000000000, 0.000000000000000000 ) ) ;
#100892 = PLANE ( 'NONE',  #70135 ) ;
#100893 = FACE_OUTER_BOUND ( 'NONE', #116938, .T. ) ;
#100894 = ADVANCED_FACE ( 'NONE', ( #52418 ), #29107, .T. ) ;
#100895 = ORIENTED_EDGE ( 'NONE', *, *, #10269, .T. ) ;
#100896 = AXIS2_PLACEMENT_3D ( 'NONE', #10752, #40922, #61180 ) ;
#100897 = CONICAL_SURFACE ( 'NONE', #38237, 0.09999999999999982514, 0.003490658503988666988 ) ;
#100898 = VECTOR ( 'NONE', #83164, 1000.000000000000000 ) ;
#100899 = ORIENTED_EDGE ( 'NONE', *, *, #37727, .F. ) ;
#100900 = DIRECTION ( 'NONE',  ( 0.000000000000000000, 0.000000000000000000, 1.000000000000000000 ) ) ;
#100901 = FACE_OUTER_BOUND ( 'NONE', #10401, .T. ) ;
#100902 = DIRECTION ( 'NONE',  ( -4.274815082592931898E-19, -0.9999939076577903929, -0.003490651415223739937 ) ) ;
#100903 = VERTEX_POINT ( 'NONE', #125505 ) ;
#100905 = DIRECTION ( 'NONE',  ( -4.274815082592931898E-19, -0.9999939076577903929, -0.003490651415223739937 ) ) ;
#100904 = AXIS2_PLACEMENT_3D ( 'NONE', #44504, #75255, #94899 ) ;
#100906 = VECTOR ( 'NONE', #128266, 1000.000000000000000 ) ;
#100907 = AXIS2_PLACEMENT_3D ( 'NONE', #25199, #114867, #86040 ) ;
#100908 = CARTESIAN_POINT ( 'NONE',  ( -10.20000000000000639, 2.500000000000000000, -3.983716857408421852 ) ) ;
#100909 = CONICAL_SURFACE ( 'NONE', #4757, 0.1000000000000002554, 0.003490658503988666988 ) ;
#100910 = EDGE_LOOP ( 'NONE', ( #70079, #47583 ) ) ;
#100911 = CONICAL_SURFACE ( 'NONE', #11026, 0.1000000000000002554, 0.003490658503988666988 ) ;
#100912 = AXIS2_PLACEMENT_3D ( 'NONE', #118694, #37577, #49342 ) ;
#100913 = CARTESIAN_POINT ( 'NONE',  ( -11.25000000000000178, 2.500000000000000000, -1.372243186433546036 ) ) ;
#100914 = ORIENTED_EDGE ( 'NONE', *, *, #25424, .F. ) ;
#100915 = CIRCLE ( 'NONE', #96713, 0.06509327318403745899 ) ;
#100916 = DIRECTION ( 'NONE',  ( -0.000000000000000000, -1.000000000000000000, -0.000000000000000000 ) ) ;
#100917 = VERTEX_POINT ( 'NONE', #32805 ) ;
#100918 = ORIENTED_EDGE ( 'NONE', *, *, #106491, .T. ) ;
#100919 = FACE_OUTER_BOUND ( 'NONE', #53290, .T. ) ;
#100920 = DIRECTION ( 'NONE',  ( 0.000000000000000000, -0.9999939076577903929, 0.003490651415223739937 ) ) ;
#100921 = ORIENTED_EDGE ( 'NONE', *, *, #12869, .F. ) ;
#100922 = ORIENTED_EDGE ( 'NONE', *, *, #8818, .F. ) ;
#100923 = CARTESIAN_POINT ( 'NONE',  ( 4.599999999999940137, 12.50000000000000000, -4.330127018922201643 ) ) ;
#100924 = DIRECTION ( 'NONE',  ( 0.000000000000000000, 1.000000000000000000, 0.000000000000000000 ) ) ;
#100925 = EDGE_LOOP ( 'NONE', ( #91310, #30981, #28072, #109648 ) ) ;
#100926 = AXIS2_PLACEMENT_3D ( 'NONE', #119404, #50679, #51354 ) ;
#100927 = DIRECTION ( 'NONE',  ( 0.000000000000000000, 0.000000000000000000, -1.000000000000000000 ) ) ;
#100928 = CARTESIAN_POINT ( 'NONE',  ( 186.2760416670080588, 6.551208109652274736, 3.782341765625001351 ) ) ;
#100929 = CARTESIAN_POINT ( 'NONE',  ( 10.39999999999990976, 2.500000000000000000, 4.230127018922196669 ) ) ;
#100930 = DIRECTION ( 'NONE',  ( 0.000000000000000000, 0.000000000000000000, 1.000000000000000000 ) ) ;
#100931 = DIRECTION ( 'NONE',  ( 0.000000000000000000, 1.000000000000000000, 0.000000000000000000 ) ) ;
#100932 = DIRECTION ( 'NONE',  ( -0.000000000000000000, -1.000000000000000000, -0.000000000000000000 ) ) ;
#100933 = FACE_OUTER_BOUND ( 'NONE', #58621, .T. ) ;
#100934 = AXIS2_PLACEMENT_3D ( 'NONE', #64977, #15223, #35549 ) ;
#100935 = AXIS2_PLACEMENT_3D ( 'NONE', #98503, #108964, #117484 ) ;
#100936 = ADVANCED_FACE ( 'NONE', ( #121798 ), #6350, .T. ) ;
#100937 = CIRCLE ( 'NONE', #36217, 0.06509327318403745899 ) ;
#100938 = EDGE_LOOP ( 'NONE', ( #5383, #57944, #817, #41104 ) ) ;
#100939 = ORIENTED_EDGE ( 'NONE', *, *, #25318, .T. ) ;
#100940 = CARTESIAN_POINT ( 'NONE',  ( -4.400000000000028777, 2.500000000000000000, -4.083716857408426826 ) ) ;
#100941 = ORIENTED_EDGE ( 'NONE', *, *, #37490, .F. ) ;
#100942 = CARTESIAN_POINT ( 'NONE',  ( 4.999999999999935163, 2.500000000000000000, 0.5928203230275495006 ) ) ;
#100943 = DIRECTION ( 'NONE',  ( 0.000000000000000000, 1.000000000000000000, 0.000000000000000000 ) ) ;
#100944 = FACE_OUTER_BOUND ( 'NONE', #104770, .T. ) ;
#100946 = ORIENTED_EDGE ( 'NONE', *, *, #82509, .F. ) ;
#100945 = EDGE_LOOP ( 'NONE', ( #127235, #96148 ) ) ;
#100947 = EDGE_CURVE ( 'NONE', #114104, #11372, #105874, .T. ) ;
#100948 = FACE_BOUND ( 'NONE', #117594, .T. ) ;
#100949 = VERTEX_POINT ( 'NONE', #23604 ) ;
#100950 = AXIS2_PLACEMENT_3D ( 'NONE', #67404, #65494, #66140 ) ;
#100951 = EDGE_CURVE ( 'NONE', #66596, #104677, #41968, .T. ) ;
#100952 = DIRECTION ( 'NONE',  ( 0.000000000000000000, 0.000000000000000000, -1.000000000000000000 ) ) ;
#100953 = CARTESIAN_POINT ( 'NONE',  ( -17.50000000000000000, 1.500000000000000000, -9.999999999999998224 ) ) ;
#100954 = CIRCLE ( 'NONE', #92544, 0.1000000000000002554 ) ;
#100956 = CARTESIAN_POINT ( 'NONE',  ( 13.09999999999990195, 12.50000000000000000, -4.676537180435978769 ) ) ;
#100955 = CONICAL_SURFACE ( 'NONE', #65447, 0.1000000000000002554, 0.003490658503988666988 ) ;
#100957 = CARTESIAN_POINT ( 'NONE',  ( 16.98713617295297951, -1.503435538384354286, 5.629434171173322454 ) ) ;
#100958 = AXIS2_PLACEMENT_3D ( 'NONE', #106826, #46003, #6049 ) ;
#100959 = DIRECTION ( 'NONE',  ( -0.000000000000000000, -1.000000000000000000, -0.000000000000000000 ) ) ;
#100960 = CARTESIAN_POINT ( 'NONE',  ( 6.899999999999928413, 2.500000000000000000, 4.676537180435972552 ) ) ;
#100961 = EDGE_CURVE ( 'NONE', #96927, #129477, #33218, .T. ) ;
#100962 = CARTESIAN_POINT ( 'NONE',  ( -7.500000000000001776, -2.500000000000000000, 1.734723475976807094E-15 ) ) ;
#100963 = EDGE_CURVE ( 'NONE', #95314, #12469, #64582, .T. ) ;
#100964 = PLANE ( 'NONE',  #35938 ) ;
#100965 = EDGE_CURVE ( 'NONE', #16718, #126358, #8143, .T. ) ;
#100966 = CARTESIAN_POINT ( 'NONE',  ( -0.8000000000000376810, 2.500000000000000000, -4.330127018922201643 ) ) ;
#100967 = DIRECTION ( 'NONE',  ( 0.000000000000000000, -0.9999939076577903929, 0.003490651415223739937 ) ) ;
#100968 = EDGE_CURVE ( 'NONE', #33066, #72150, #100102, .T. ) ;
#100969 = AXIS2_PLACEMENT_3D ( 'NONE', #86254, #6386, #57467 ) ;
#100970 = DIRECTION ( 'NONE',  ( 0.000000000000000000, 0.000000000000000000, 1.000000000000000000 ) ) ;
#100971 = ORIENTED_EDGE ( 'NONE', *, *, #59203, .T. ) ;
#100972 = VERTEX_POINT ( 'NONE', #123102 ) ;
#100973 = VERTEX_POINT ( 'NONE', #26031 ) ;
#100975 = EDGE_LOOP ( 'NONE', ( #69897, #75390, #101136, #100561 ) ) ;
#100974 = AXIS2_PLACEMENT_3D ( 'NONE', #98099, #129531, #39857 ) ;
#100976 = AXIS2_PLACEMENT_3D ( 'NONE', #33105, #92001, #112928 ) ;
#100977 = AXIS2_PLACEMENT_3D ( 'NONE', #105970, #67968, #27387 ) ;
#100978 = DIRECTION ( 'NONE',  ( 0.000000000000000000, 0.000000000000000000, 1.000000000000000000 ) ) ;
#100979 = CARTESIAN_POINT ( 'NONE',  ( 12.49999999999993960, 2.500000000000000000, 4.330127018922196314 ) ) ;
#100981 = ORIENTED_EDGE ( 'NONE', *, *, #31691, .F. ) ;
#100980 = ORIENTED_EDGE ( 'NONE', *, *, #99182, .F. ) ;
#100982 = ORIENTED_EDGE ( 'NONE', *, *, #35687, .F. ) ;
#100983 = AXIS2_PLACEMENT_3D ( 'NONE', #71814, #11596, #80986 ) ;
#100984 = CARTESIAN_POINT ( 'NONE',  ( 185.0416666666667140, -4.445597072760063107, 7.700000000000102318 ) ) ;
#100985 = DIRECTION ( 'NONE',  ( 0.000000000000000000, -0.000000000000000000, 1.000000000000000000 ) ) ;
#100986 = DIRECTION ( 'NONE',  ( 0.000000000000000000, -0.000000000000000000, 1.000000000000000000 ) ) ;
#100987 = DIRECTION ( 'NONE',  ( 0.000000000000000000, 0.000000000000000000, 1.000000000000000000 ) ) ;
#100988 = CARTESIAN_POINT ( 'NONE',  ( -9.600000000000008527, 2.500000000000000000, 4.330127018922196314 ) ) ;
#100989 = CARTESIAN_POINT ( 'NONE',  ( 9.399999999999915090, 2.500000000000000000, -4.676537180435977881 ) ) ;
#100990 = CARTESIAN_POINT ( 'NONE',  ( 15.39999999999989200, 2.500000000000000000, -0.6928203230275542523 ) ) ;
#100991 = ORIENTED_EDGE ( 'NONE', *, *, #9547, .T. ) ;
#100992 = DIRECTION ( 'NONE',  ( 0.000000000000000000, 0.000000000000000000, 1.000000000000000000 ) ) ;
#100993 = ORIENTED_EDGE ( 'NONE', *, *, #70510, .T. ) ;
#100994 = ORIENTED_EDGE ( 'NONE', *, *, #4595, .T. ) ;
#100995 = ORIENTED_EDGE ( 'NONE', *, *, #125327, .T. ) ;
#100996 = DIRECTION ( 'NONE',  ( 0.000000000000000000, -0.000000000000000000, 1.000000000000000000 ) ) ;
#100997 = VECTOR ( 'NONE', #80569, 1000.000000000000000 ) ;
#100999 = EDGE_CURVE ( 'NONE', #14446, #45963, #60407, .T. ) ;
#100998 = CIRCLE ( 'NONE', #11096, 0.06509327318403745899 ) ;
#101000 = ORIENTED_EDGE ( 'NONE', *, *, #90362, .F. ) ;
#101001 = EDGE_LOOP ( 'NONE', ( #31779, #11084, #29863, #117899 ) ) ;
#101002 = EDGE_LOOP ( 'NONE', ( #108796, #17677 ) ) ;
#101003 = DIRECTION ( 'NONE',  ( 0.000000000000000000, 0.000000000000000000, 1.000000000000000000 ) ) ;
#101004 = DIRECTION ( 'NONE',  ( -0.000000000000000000, -1.000000000000000000, -0.000000000000000000 ) ) ;
#101005 = CARTESIAN_POINT ( 'NONE',  ( 108.0000000000000142, 9.000000000000001776, 0.2500000000000000000 ) ) ;
#101006 = FACE_OUTER_BOUND ( 'NONE', #120574, .T. ) ;
#101007 = DIRECTION ( 'NONE',  ( 0.000000000000000000, 1.000000000000000000, 0.000000000000000000 ) ) ;
#101008 = AXIS2_PLACEMENT_3D ( 'NONE', #510, #28709, #59479 ) ;
#101009 = EDGE_CURVE ( 'NONE', #44822, #120717, #56268, .T. ) ;
#101010 = CARTESIAN_POINT ( 'NONE',  ( -8.550000000000013145, 2.500000000000000000, 2.511473670974873507 ) ) ;
#101011 = EDGE_CURVE ( 'NONE', #40034, #84934, #41635, .T. ) ;
#101012 = EDGE_CURVE ( 'NONE', #103318, #58785, #114752, .T. ) ;
#101013 = LINE ( 'NONE', #41478, #80550 ) ;
#101014 = VERTEX_POINT ( 'NONE', #53708 ) ;
#101015 = LINE ( 'NONE', #11350, #75615 ) ;
#101016 = CIRCLE ( 'NONE', #117717, 0.06509327318403745899 ) ;
#101017 = VERTEX_POINT ( 'NONE', #102175 ) ;
#101018 = DIRECTION ( 'NONE',  ( -4.274815082592931898E-19, -0.9999939076577903929, -0.003490651415223739937 ) ) ;
#101019 = LINE ( 'NONE', #121955, #18962 ) ;
#101020 = CONICAL_SURFACE ( 'NONE', #29924, 0.1000000000000000472, 0.003490658503988666988 ) ;
#101022 = EDGE_LOOP ( 'NONE', ( #113640, #49967 ) ) ;
#101021 = EDGE_CURVE ( 'NONE', #12902, #10113, #129374, .T. ) ;
#101023 = CARTESIAN_POINT ( 'NONE',  ( -13.29999999999998828, 12.50000000000000000, 4.330127018922196314 ) ) ;
#101024 = EDGE_CURVE ( 'NONE', #69317, #108726, #39583, .T. ) ;
#101025 = CARTESIAN_POINT ( 'NONE',  ( 15.19999999999989271, 12.50000000000000000, -0.3464101615137783474 ) ) ;
#101026 = ORIENTED_EDGE ( 'NONE', *, *, #36978, .T. ) ;
#101027 = AXIS2_PLACEMENT_3D ( 'NONE', #115329, #47274, #87172 ) ;
#101028 = EDGE_CURVE ( 'NONE', #28470, #94678, #68795, .T. ) ;
#101029 = EDGE_CURVE ( 'NONE', #51312, #47117, #16538, .T. ) ;
#101030 = EDGE_CURVE ( 'NONE', #98954, #7787, #41713, .T. ) ;
#101031 = CARTESIAN_POINT ( 'NONE',  ( 12.69999999999990159, 12.50000000000000000, 4.676537180435972552 ) ) ;
#101032 = EDGE_LOOP ( 'NONE', ( #113143, #95904 ) ) ;
#101033 = VERTEX_POINT ( 'NONE', #86868 ) ;
#101034 = CARTESIAN_POINT ( 'NONE',  ( 5.849999999999934808, 2.500000000000000000, -5.802370205355749988 ) ) ;
#101035 = CARTESIAN_POINT ( 'NONE',  ( 12.09999999999990195, 2.500000000000000000, 0.09999999999999772959 ) ) ;
#101036 = DIRECTION ( 'NONE',  ( 0.000000000000000000, -0.9999939076577903929, 0.003490651415223739937 ) ) ;
#101037 = PLANE ( 'NONE',  #11663 ) ;
#101038 = EDGE_CURVE ( 'NONE', #121928, #5867, #112808, .T. ) ;
#101039 = CONICAL_SURFACE ( 'NONE', #84304, 0.09999999999999982514, 0.003490658503988666988 ) ;
#101040 = CARTESIAN_POINT ( 'NONE',  ( 6.699999999999928235, 2.500000000000000000, -0.1000000000000022815 ) ) ;
#101041 = ORIENTED_EDGE ( 'NONE', *, *, #30551, .F. ) ;
#101042 = DIRECTION ( 'NONE',  ( 0.000000000000000000, 0.000000000000000000, -1.000000000000000000 ) ) ;
#101043 = CIRCLE ( 'NONE', #6923, 0.06509327318403745899 ) ;
#101044 = ORIENTED_EDGE ( 'NONE', *, *, #105449, .F. ) ;
#101045 = AXIS2_PLACEMENT_3D ( 'NONE', #4168, #123953, #45414 ) ;
#101046 = CARTESIAN_POINT ( 'NONE',  ( 4.149999999999938183, 12.50000000000000000, 5.802370205355744659 ) ) ;
#101047 = CARTESIAN_POINT ( 'NONE',  ( 10.39999999999990976, 12.50000000000000000, -4.330127018922201643 ) ) ;
#101048 = AXIS2_PLACEMENT_3D ( 'NONE', #88378, #9194, #87101 ) ;
#101049 = CARTESIAN_POINT ( 'NONE',  ( 186.5468750003414300, -8.734944146203032389, -1.604583208406768146E-15 ) ) ;
#101050 = DIRECTION ( 'NONE',  ( 0.000000000000000000, 0.000000000000000000, -1.000000000000000000 ) ) ;
#101051 = CARTESIAN_POINT ( 'NONE',  ( 6.249999999999965361, 2.500000000000000000, 2.165063509461097713 ) ) ;
#101052 = CARTESIAN_POINT ( 'NONE',  ( 10.84999999999991260, 12.50000000000000000, 7.188010851410848723 ) ) ;
#101053 = CONICAL_SURFACE ( 'NONE', #124035, 0.1000000000000000472, 0.003490658503988666988 ) ;
#101055 = VECTOR ( 'NONE', #101345, 1000.000000000000000 ) ;
#101054 = CARTESIAN_POINT ( 'NONE',  ( -6.250000000000021316, 2.500000000000000000, -1.372243186433550033 ) ) ;
#101056 = EDGE_LOOP ( 'NONE', ( #66598, #12784 ) ) ;
#101057 = CIRCLE ( 'NONE', #32215, 0.1000000000000002554 ) ;
#101058 = CIRCLE ( 'NONE', #11165, 0.1000000000000002554 ) ;
#101059 = CARTESIAN_POINT ( 'NONE',  ( 5.399999999999931966, 2.500000000000000000, 4.330127018922196314 ) ) ;
#101060 = CARTESIAN_POINT ( 'NONE',  ( -3.950000000000024603, 12.50000000000000000, -2.511473670974877948 ) ) ;
#101061 = CARTESIAN_POINT ( 'NONE',  ( -11.64999999999999680, 2.500000000000000000, -2.957883832488649833 ) ) ;
#101062 = AXIS2_PLACEMENT_3D ( 'NONE', #79873, #60257, #82947 ) ;
#101063 = ORIENTED_EDGE ( 'NONE', *, *, #18216, .T. ) ;
#101064 = CARTESIAN_POINT ( 'NONE',  ( -3.100000000000028955, 2.500000000000000000, 3.883716857408421319 ) ) ;
#101065 = ADVANCED_FACE ( 'NONE', ( #38443 ), #8236, .T. ) ;
#101066 = ORIENTED_EDGE ( 'NONE', *, *, #32128, .T. ) ;
#101067 = CONICAL_SURFACE ( 'NONE', #714, 0.1000000000000002554, 0.003490658503988666988 ) ;
#101069 = ORIENTED_EDGE ( 'NONE', *, *, #16015, .F. ) ;
#101068 = CIRCLE ( 'NONE', #115631, 0.1000000000000000472 ) ;
#101070 = VECTOR ( 'NONE', #46909, 1000.000000000000000 ) ;
#101071 = DIRECTION ( 'NONE',  ( 0.000000000000000000, 0.000000000000000000, -1.000000000000000000 ) ) ;
#101073 = ORIENTED_EDGE ( 'NONE', *, *, #37254, .T. ) ;
#101072 = AXIS2_PLACEMENT_3D ( 'NONE', #69724, #109652, #71017 ) ;
#101074 = DIRECTION ( 'NONE',  ( -4.274815082592931898E-19, -0.9999939076577903929, -0.003490651415223739937 ) ) ;
#101075 = LINE ( 'NONE', #80151, #38264 ) ;
#101076 = DIRECTION ( 'NONE',  ( -0.000000000000000000, -1.000000000000000000, -0.000000000000000000 ) ) ;
#101077 = EDGE_LOOP ( 'NONE', ( #62121, #21471 ) ) ;
#101078 = DIRECTION ( 'NONE',  ( 0.000000000000000000, 0.000000000000000000, 1.000000000000000000 ) ) ;
#101079 = DIRECTION ( 'NONE',  ( -0.000000000000000000, 1.000000000000000000, -0.000000000000000000 ) ) ;
#101080 = DIRECTION ( 'NONE',  ( 0.000000000000000000, 0.000000000000000000, 1.000000000000000000 ) ) ;
#101081 = EDGE_CURVE ( 'NONE', #22839, #111368, #87653, .T. ) ;
#101082 = ORIENTED_EDGE ( 'NONE', *, *, #89326, .T. ) ;
#101083 = EDGE_LOOP ( 'NONE', ( #57800, #34646, #74383, #54252 ) ) ;
#101084 = ORIENTED_EDGE ( 'NONE', *, *, #102730, .T. ) ;
#101085 = CARTESIAN_POINT ( 'NONE',  ( -0.6500000000000389910, 2.500000000000000000, -1.818653347947326138 ) ) ;
#101086 = PLANE ( 'NONE',  #54185 ) ;
#101088 = DIRECTION ( 'NONE',  ( 0.000000000000000000, 0.000000000000000000, -1.000000000000000000 ) ) ;
#101087 = CIRCLE ( 'NONE', #73896, 0.1000000000000002554 ) ;
#101089 = AXIS2_PLACEMENT_3D ( 'NONE', #34662, #65373, #33997 ) ;
#101090 = FACE_BOUND ( 'NONE', #68742, .T. ) ;
#101091 = ORIENTED_EDGE ( 'NONE', *, *, #15659, .T. ) ;
#101092 = DIRECTION ( 'NONE',  ( 0.000000000000000000, 1.000000000000000000, 0.000000000000000000 ) ) ;
#101093 = CARTESIAN_POINT ( 'NONE',  ( -0.8500000000000382805, 2.500000000000000000, -5.902370205355750521 ) ) ;
#101094 = ORIENTED_EDGE ( 'NONE', *, *, #129344, .T. ) ;
#101095 = CARTESIAN_POINT ( 'NONE',  ( -0.8500000000000395017, 12.50000000000000000, 6.495190528383297135 ) ) ;
#101096 = CARTESIAN_POINT ( 'NONE',  ( 17.49149641758760509, 2.499999999999969358, 4.292093396892645352 ) ) ;
#101097 = AXIS2_PLACEMENT_3D ( 'NONE', #33896, #75113, #105206 ) ;
#101098 = AXIS2_PLACEMENT_3D ( 'NONE', #101316, #11634, #43703 ) ;
#101100 = AXIS2_PLACEMENT_3D ( 'NONE', #103618, #15858, #115998 ) ;
#101099 = DIRECTION ( 'NONE',  ( 0.000000000000000000, 0.000000000000000000, 1.000000000000000000 ) ) ;
#101101 = DIRECTION ( 'NONE',  ( 0.000000000000000000, 1.000000000000000000, 0.000000000000000000 ) ) ;
#101102 = DIRECTION ( 'NONE',  ( 0.000000000000000000, 0.000000000000000000, -1.000000000000000000 ) ) ;
#101103 = CARTESIAN_POINT ( 'NONE',  ( -8.300000000000011369, 2.500000000000000000, -2.276824562219559311E-15 ) ) ;
#101104 = CARTESIAN_POINT ( 'NONE',  ( 2.299999999999948752, 2.500000000000000000, -3.983716857408426293 ) ) ;
#101105 = VECTOR ( 'NONE', #11851, 1000.000000000000000 ) ;
#101106 = AXIS2_PLACEMENT_3D ( 'NONE', #109527, #1490, #51902 ) ;
#101108 = EDGE_CURVE ( 'NONE', #126341, #83526, #33310, .T. ) ;
#101107 = AXIS2_PLACEMENT_3D ( 'NONE', #85318, #35590, #66319 ) ;
#101109 = ORIENTED_EDGE ( 'NONE', *, *, #73504, .T. ) ;
#101110 = ORIENTED_EDGE ( 'NONE', *, *, #22512, .F. ) ;
#101111 = ORIENTED_EDGE ( 'NONE', *, *, #49281, .T. ) ;
#101112 = EDGE_LOOP ( 'NONE', ( #64152, #67688, #40333, #106411 ) ) ;
#101113 = DIRECTION ( 'NONE',  ( 0.000000000000000000, 1.000000000000000000, 0.000000000000000000 ) ) ;
#101114 = VECTOR ( 'NONE', #70, 1000.000000000000000 ) ;
#101115 = CARTESIAN_POINT ( 'NONE',  ( -8.749999999999976907, 12.50000000000000000, -6.560283801567334372 ) ) ;
#101116 = EDGE_LOOP ( 'NONE', ( #108939, #30817 ) ) ;
#101117 = FACE_BOUND ( 'NONE', #52006, .T. ) ;
#101118 = ADVANCED_FACE ( 'NONE', ( #67870 ), #121116, .T. ) ;
#101119 = DIRECTION ( 'NONE',  ( -0.000000000000000000, 1.000000000000000000, -0.000000000000000000 ) ) ;
#101120 = DIRECTION ( 'NONE',  ( -4.274815082592931898E-19, -0.9999939076577903929, -0.003490651415223739937 ) ) ;
#101121 = LINE ( 'NONE', #7074, #111858 ) ;
#101122 = DIRECTION ( 'NONE',  ( 0.000000000000000000, 0.000000000000000000, -1.000000000000000000 ) ) ;
#101123 = DIRECTION ( 'NONE',  ( -0.000000000000000000, -1.000000000000000000, -0.000000000000000000 ) ) ;
#101124 = EDGE_CURVE ( 'NONE', #124699, #120570, #31245, .T. ) ;
#101125 = CARTESIAN_POINT ( 'NONE',  ( 12.69999999999989981, 12.50000000000000000, -0.3464101615137783474 ) ) ;
#101126 = ADVANCED_FACE ( 'NONE', ( #118262 ), #127385, .T. ) ;
#101127 = PLANE ( 'NONE',  #104006 ) ;
#101128 = CARTESIAN_POINT ( 'NONE',  ( -1.850000000000033396, 12.50000000000000000, -1.818653347947325916 ) ) ;
#101129 = EDGE_CURVE ( 'NONE', #51103, #16412, #62638, .T. ) ;
#101130 = CARTESIAN_POINT ( 'NONE',  ( 12.49999999999990408, 12.50000000000000000, -3.637306695894650055 ) ) ;
#101131 = EDGE_CURVE ( 'NONE', #59733, #88940, #79363, .T. ) ;
#101132 = ORIENTED_EDGE ( 'NONE', *, *, #1122, .T. ) ;
#101133 = ADVANCED_FACE ( 'NONE', ( #79011 ), #22927, .T. ) ;
#101134 = CIRCLE ( 'NONE', #63477, 0.1000000000000000056 ) ;
#101135 = ORIENTED_EDGE ( 'NONE', *, *, #90865, .F. ) ;
#101136 = ORIENTED_EDGE ( 'NONE', *, *, #46305, .T. ) ;
#101137 = ORIENTED_EDGE ( 'NONE', *, *, #57677, .F. ) ;
#101138 = VERTEX_POINT ( 'NONE', #67194 ) ;
#101139 = ORIENTED_EDGE ( 'NONE', *, *, #25077, .T. ) ;
#101140 = DIRECTION ( 'NONE',  ( 0.000000000000000000, 0.000000000000000000, 1.000000000000000000 ) ) ;
#101141 = ORIENTED_EDGE ( 'NONE', *, *, #105582, .T. ) ;
#101142 = EDGE_CURVE ( 'NONE', #126312, #103698, #18124, .T. ) ;
#101143 = VECTOR ( 'NONE', #91400, 1000.000000000000000 ) ;
#101145 = EDGE_CURVE ( 'NONE', #113182, #72573, #87501, .T. ) ;
#101144 = CIRCLE ( 'NONE', #44714, 0.1000000000000002554 ) ;
#101146 = VECTOR ( 'NONE', #78236, 1000.000000000000000 ) ;
#101147 = ADVANCED_FACE ( 'NONE', ( #88130 ), #58436, .T. ) ;
#101148 = CARTESIAN_POINT ( 'NONE',  ( 16.86635082839116606, 0.4716143926291154198, 5.778906370536208925 ) ) ;
#101149 = CARTESIAN_POINT ( 'NONE',  ( 13.51931942407985332, -1.499999999999904521, 8.074217333073772096 ) ) ;
#101150 = DIRECTION ( 'NONE',  ( 0.000000000000000000, -0.9999939076577903929, 0.003490651415223739937 ) ) ;
#101151 = CARTESIAN_POINT ( 'NONE',  ( -3.550000000000031797, 12.50000000000000000, -6.083687093685488989 ) ) ;
#101152 = CIRCLE ( 'NONE', #34266, 0.09999999999999999167 ) ;
#101153 = ORIENTED_EDGE ( 'NONE', *, *, #82726, .F. ) ;
#101154 = CARTESIAN_POINT ( 'NONE',  ( 1.649999999999951505, 12.50000000000000000, -2.922977105672691422 ) ) ;
#101155 = CIRCLE ( 'NONE', #42588, 0.1000000000000002554 ) ;
#101156 = VECTOR ( 'NONE', #74913, 1000.000000000000000 ) ;
#101157 = ORIENTED_EDGE ( 'NONE', *, *, #15949, .F. ) ;
#101158 = CIRCLE ( 'NONE', #101239, 0.1000000000000002554 ) ;
#101159 = ORIENTED_EDGE ( 'NONE', *, *, #67985, .T. ) ;
#101160 = LINE ( 'NONE', #51430, #34313 ) ;
#101161 = DIRECTION ( 'NONE',  ( 0.000000000000000000, 0.000000000000000000, 1.000000000000000000 ) ) ;
#101162 = CARTESIAN_POINT ( 'NONE',  ( 8.549999999999918998, 2.500000000000000000, 6.841600689897072485 ) ) ;
#101163 = AXIS2_PLACEMENT_3D ( 'NONE', #127380, #114956, #96600 ) ;
#101164 = ORIENTED_EDGE ( 'NONE', *, *, #2482, .F. ) ;
#101165 = VERTEX_POINT ( 'NONE', #37780 ) ;
#101166 = DIRECTION ( 'NONE',  ( 0.000000000000000000, 0.000000000000000000, 1.000000000000000000 ) ) ;
#101167 = DIRECTION ( 'NONE',  ( 0.000000000000000000, 1.000000000000000000, 0.000000000000000000 ) ) ;
#101168 = CARTESIAN_POINT ( 'NONE',  ( -10.65000000000000213, 12.50000000000000000, 2.511473670974873507 ) ) ;
#101169 = DIRECTION ( 'NONE',  ( -0.000000000000000000, 1.000000000000000000, -0.000000000000000000 ) ) ;
#101170 = VERTEX_POINT ( 'NONE', #98603 ) ;
#101171 = DIRECTION ( 'NONE',  ( 0.000000000000000000, 1.000000000000000000, 0.000000000000000000 ) ) ;
#101172 = AXIS2_PLACEMENT_3D ( 'NONE', #42201, #978, #93235 ) ;
#101173 = ORIENTED_EDGE ( 'NONE', *, *, #75766, .F. ) ;
#101174 = CONICAL_SURFACE ( 'NONE', #42705, 0.1000000000000002554, 0.003490658503988666988 ) ;
#101175 = FACE_OUTER_BOUND ( 'NONE', #45260, .T. ) ;
#101176 = ORIENTED_EDGE ( 'NONE', *, *, #113779, .T. ) ;
#101177 = CARTESIAN_POINT ( 'NONE',  ( 186.2500000000000000, 9.429780353434619030E-16, -7.700000000000000178 ) ) ;
#101178 = CARTESIAN_POINT ( 'NONE',  ( 1.849999999999949019, 2.500000000000000000, 6.841600689897072485 ) ) ;
#101179 = CARTESIAN_POINT ( 'NONE',  ( 3.549999999999943867, 2.500000000000000000, -6.148780366869526226 ) ) ;
#101180 = EDGE_CURVE ( 'NONE', #40494, #108185, #77208, .T. ) ;
#101181 = DIRECTION ( 'NONE',  ( 0.000000000000000000, 1.000000000000000000, 0.000000000000000000 ) ) ;
#101182 = VERTEX_POINT ( 'NONE', #78362 ) ;
#101183 = ADVANCED_FACE ( 'NONE', ( #8942 ), #75149, .T. ) ;
#101184 = CARTESIAN_POINT ( 'NONE',  ( -5.850000000000019185, 2.500000000000000000, 2.065063509461097624 ) ) ;
#101185 = EDGE_CURVE ( 'NONE', #63648, #111056, #116319, .T. ) ;
#101186 = CARTESIAN_POINT ( 'NONE',  ( 9.999999999999948486, 2.500000000000000000, 4.430127018922196847 ) ) ;
#101187 = EDGE_LOOP ( 'NONE', ( #93267, #7627 ) ) ;
#101188 = ORIENTED_EDGE ( 'NONE', *, *, #74344, .F. ) ;
#101189 = CONICAL_SURFACE ( 'NONE', #13335, 0.1000000000000000056, 0.003490658503988666988 ) ;
#101190 = VECTOR ( 'NONE', #128182, 1000.000000000000000 ) ;
#101191 = ORIENTED_EDGE ( 'NONE', *, *, #2026, .T. ) ;
#101192 = CARTESIAN_POINT ( 'NONE',  ( 17.50000000000000000, -0.9166666666666694052, 4.000000000000001776 ) ) ;
#101193 = CARTESIAN_POINT ( 'NONE',  ( 1.899999999999951283, 2.500000000000000000, -4.676537180435977881 ) ) ;
#101194 = CARTESIAN_POINT ( 'NONE',  ( 20.59313469514023964, 2.666874593322334341, 2.243770147468749698 ) ) ;
#101195 = DIRECTION ( 'NONE',  ( -0.000000000000000000, 1.000000000000000000, -0.000000000000000000 ) ) ;
#101196 = CARTESIAN_POINT ( 'NONE',  ( 2.299999999999947864, 2.500000000000000000, 3.883716857408421319 ) ) ;
#101197 = EDGE_CURVE ( 'NONE', #48618, #56136, #127453, .T. ) ;
#101198 = CARTESIAN_POINT ( 'NONE',  ( -8.300000000000011369, 2.500000000000000000, -4.330127018922201643 ) ) ;
#101199 = CIRCLE ( 'NONE', #9253, 0.09999999999999982514 ) ;
#101200 = DIRECTION ( 'NONE',  ( 0.000000000000000000, 0.000000000000000000, 1.000000000000000000 ) ) ;
#101201 = AXIS2_PLACEMENT_3D ( 'NONE', #29734, #27153, #67050 ) ;
#101202 = DIRECTION ( 'NONE',  ( 0.000000000000000000, 0.000000000000000000, 1.000000000000000000 ) ) ;
#101204 = VECTOR ( 'NONE', #98252, 1000.000000000000000 ) ;
#101203 = DIRECTION ( 'NONE',  ( 0.000000000000000000, 0.000000000000000000, -1.000000000000000000 ) ) ;
#101205 = AXIS2_PLACEMENT_3D ( 'NONE', #122325, #112497, #20889 ) ;
#101206 = VECTOR ( 'NONE', #12594, 1000.000000000000000 ) ;
#101207 = CIRCLE ( 'NONE', #92903, 0.09999999999999999167 ) ;
#101208 = EDGE_LOOP ( 'NONE', ( #66685, #47876, #129188, #40329 ) ) ;
#101209 = DIRECTION ( 'NONE',  ( 0.000000000000000000, 0.000000000000000000, -1.000000000000000000 ) ) ;
#101210 = CARTESIAN_POINT ( 'NONE',  ( -1.850000000000033396, 2.500000000000000000, -6.048780366869526581 ) ) ;
#101211 = EDGE_CURVE ( 'NONE', #13926, #48067, #123180, .T. ) ;
#101212 = CARTESIAN_POINT ( 'NONE',  ( -1.250000000000037526, 12.50000000000000000, -5.737276932171712751 ) ) ;
#101213 = DIRECTION ( 'NONE',  ( 0.000000000000000000, 1.000000000000000000, 0.000000000000000000 ) ) ;
#101214 = ORIENTED_EDGE ( 'NONE', *, *, #89301, .T. ) ;
#101215 = FACE_OUTER_BOUND ( 'NONE', #43716, .T. ) ;
#101216 = DIRECTION ( 'NONE',  ( 0.000000000000000000, 0.000000000000000000, 1.000000000000000000 ) ) ;
#101218 = ORIENTED_EDGE ( 'NONE', *, *, #3767, .T. ) ;
#101217 = LINE ( 'NONE', #41028, #104788 ) ;
#101219 = AXIS2_PLACEMENT_3D ( 'NONE', #33558, #3433, #82656 ) ;
#101220 = VECTOR ( 'NONE', #38648, 1000.000000000000000 ) ;
#101221 = VERTEX_POINT ( 'NONE', #50195 ) ;
#101222 = DIRECTION ( 'NONE',  ( 0.000000000000000000, 0.000000000000000000, 1.000000000000000000 ) ) ;
#101223 = ADVANCED_FACE ( 'NONE', ( #71754 ), #52163, .T. ) ;
#101224 = ORIENTED_EDGE ( 'NONE', *, *, #80353, .F. ) ;
#101225 = VERTEX_POINT ( 'NONE', #79632 ) ;
#101226 = DIRECTION ( 'NONE',  ( -0.000000000000000000, 1.000000000000000000, -0.000000000000000000 ) ) ;
#101227 = FACE_OUTER_BOUND ( 'NONE', #121411, .T. ) ;
#101228 = CARTESIAN_POINT ( 'NONE',  ( 2.299999999999949640, 2.500000000000000000, -0.3464101615137782364 ) ) ;
#101229 = VECTOR ( 'NONE', #44280, 1000.000000000000000 ) ;
#101230 = CARTESIAN_POINT ( 'NONE',  ( 14.39999999999989555, 2.500000000000000000, 0.2464101615137736789 ) ) ;
#101231 = AXIS2_PLACEMENT_3D ( 'NONE', #47162, #97534, #5282 ) ;
#101232 = ORIENTED_EDGE ( 'NONE', *, *, #16495, .F. ) ;
#101233 = DIRECTION ( 'NONE',  ( 0.000000000000000000, 1.000000000000000000, 0.000000000000000000 ) ) ;
#101234 = EDGE_LOOP ( 'NONE', ( #116643, #62531 ) ) ;
#101235 = CARTESIAN_POINT ( 'NONE',  ( 16.96615051717511591, 1.026750547576220862, 5.590381354649148093 ) ) ;
#101236 = ADVANCED_FACE ( 'NONE', ( #60020 ), #60654, .T. ) ;
#101237 = CARTESIAN_POINT ( 'NONE',  ( 3.149999999999942624, 2.500000000000000000, 6.741600689897071952 ) ) ;
#101238 = EDGE_LOOP ( 'NONE', ( #502, #127855, #61160, #36117 ) ) ;
#101239 = AXIS2_PLACEMENT_3D ( 'NONE', #98463, #117442, #97832 ) ;
#101240 = ORIENTED_EDGE ( 'NONE', *, *, #113883, .T. ) ;
#101241 = ORIENTED_EDGE ( 'NONE', *, *, #93511, .T. ) ;
#101242 = ORIENTED_EDGE ( 'NONE', *, *, #53819, .F. ) ;
#101243 = DIRECTION ( 'NONE',  ( 0.000000000000000000, 1.000000000000000000, 0.000000000000000000 ) ) ;
#101244 = CARTESIAN_POINT ( 'NONE',  ( 8.340322510126762623, 2.500000000000001332, 8.517653997967753909 ) ) ;
#101245 = CARTESIAN_POINT ( 'NONE',  ( 3.099999999999945022, 2.500000000000000000, -0.3464101615137783474 ) ) ;
#101246 = FACE_BOUND ( 'NONE', #24698, .T. ) ;
#101247 = FACE_OUTER_BOUND ( 'NONE', #70465, .T. ) ;
#101248 = CARTESIAN_POINT ( 'NONE',  ( 185.6979166673494603, 6.668395609140176816, 3.850000000000000977 ) ) ;
#101249 = CARTESIAN_POINT ( 'NONE',  ( 11.24999999999990941, 2.500000000000000000, 7.188010851410848723 ) ) ;
#101250 = CARTESIAN_POINT ( 'NONE',  ( -8.350000000000013856, 12.50000000000000000, -5.802370205355744659 ) ) ;
#101251 = AXIS2_PLACEMENT_3D ( 'NONE', #110730, #2061, #111363 ) ;
#101252 = CIRCLE ( 'NONE', #99208, 0.1000000000000002554 ) ;
#101253 = DIRECTION ( 'NONE',  ( 0.000000000000000000, 0.000000000000000000, 1.000000000000000000 ) ) ;
#101254 = CARTESIAN_POINT ( 'NONE',  ( -13.14999999999999147, 2.500000000000000000, -2.611473670974875372 ) ) ;
#101255 = AXIS2_PLACEMENT_3D ( 'NONE', #93715, #23685, #63620 ) ;
#101256 = DIRECTION ( 'NONE',  ( 0.000000000000000000, 0.000000000000000000, 1.000000000000000000 ) ) ;
#101257 = VECTOR ( 'NONE', #73079, 1000.000000000000000 ) ;
#101258 = CARTESIAN_POINT ( 'NONE',  ( -5.850000000000021849, 12.50000000000000000, -1.472243186433550122 ) ) ;
#101259 = ADVANCED_FACE ( 'NONE', ( #20077 ), #29199, .T. ) ;
#101260 = VERTEX_POINT ( 'NONE', #2337 ) ;
#101261 = ORIENTED_EDGE ( 'NONE', *, *, #40395, .F. ) ;
#101262 = VERTEX_POINT ( 'NONE', #40371 ) ;
#101263 = ORIENTED_EDGE ( 'NONE', *, *, #83606, .F. ) ;
#101264 = EDGE_LOOP ( 'NONE', ( #119926, #10785 ) ) ;
#101265 = DIRECTION ( 'NONE',  ( -0.000000000000000000, 1.000000000000000000, -0.000000000000000000 ) ) ;
#101266 = DIRECTION ( 'NONE',  ( 0.000000000000000000, 1.000000000000000000, 0.000000000000000000 ) ) ;
#101267 = ORIENTED_EDGE ( 'NONE', *, *, #31527, .F. ) ;
#101268 = FACE_BOUND ( 'NONE', #98038, .T. ) ;
#101269 = FACE_OUTER_BOUND ( 'NONE', #25117, .T. ) ;
#101270 = EDGE_CURVE ( 'NONE', #125301, #76186, #45908, .T. ) ;
#101271 = AXIS2_PLACEMENT_3D ( 'NONE', #32140, #101509, #89107 ) ;
#101272 = AXIS2_PLACEMENT_3D ( 'NONE', #83010, #41806, #84274 ) ;
#101274 = ORIENTED_EDGE ( 'NONE', *, *, #52932, .F. ) ;
#101273 = AXIS2_PLACEMENT_3D ( 'NONE', #109038, #127418, #79604 ) ;
#101275 = EDGE_CURVE ( 'NONE', #57444, #48343, #80289, .T. ) ;
#101277 = VECTOR ( 'NONE', #27370, 1000.000000000000000 ) ;
#101276 = DIRECTION ( 'NONE',  ( 0.000000000000000000, 0.000000000000000000, 1.000000000000000000 ) ) ;
#101278 = CARTESIAN_POINT ( 'NONE',  ( 5.199999999999937117, 12.50000000000000000, -4.741630453620016006 ) ) ;
#101279 = EDGE_CURVE ( 'NONE', #29350, #102543, #119065, .T. ) ;
#101280 = CARTESIAN_POINT ( 'NONE',  ( -2.050000000000032685, 2.500000000000000000, -2.165063509461101710 ) ) ;
#101281 = EDGE_CURVE ( 'NONE', #97971, #115638, #96069, .T. ) ;
#101282 = DIRECTION ( 'NONE',  ( 0.000000000000000000, 0.000000000000000000, -1.000000000000000000 ) ) ;
#101283 = EDGE_CURVE ( 'NONE', #39915, #103444, #39670, .T. ) ;
#101284 = ORIENTED_EDGE ( 'NONE', *, *, #123031, .T. ) ;
#101285 = CARTESIAN_POINT ( 'NONE',  ( 4.149999999999939959, 2.500000000000000000, -2.265063509461101798 ) ) ;
#101286 = CONICAL_SURFACE ( 'NONE', #124275, 0.09999999999999999167, 0.003490658503988666988 ) ;
#101287 = CIRCLE ( 'NONE', #28132, 0.06509327318403745899 ) ;
#101288 = VECTOR ( 'NONE', #83357, 1000.000000000000000 ) ;
#101289 = ORIENTED_EDGE ( 'NONE', *, *, #25069, .T. ) ;
#101290 = EDGE_CURVE ( 'NONE', #6486, #34419, #70943, .T. ) ;
#101291 = ORIENTED_EDGE ( 'NONE', *, *, #109246, .T. ) ;
#101292 = LINE ( 'NONE', #21430, #80063 ) ;
#101293 = EDGE_CURVE ( 'NONE', #95559, #99317, #43774, .T. ) ;
#101294 = CARTESIAN_POINT ( 'NONE',  ( 3.349999999999945466, 12.50000000000000000, -2.165063509461101710 ) ) ;
#101295 = ORIENTED_EDGE ( 'NONE', *, *, #63331, .F. ) ;
#101296 = ADVANCED_FACE ( 'NONE', ( #99928 ), #102498, .T. ) ;
#101297 = CARTESIAN_POINT ( 'NONE',  ( -12.09999999999999609, 2.500000000000000000, -4.330127018922198978 ) ) ;
#101298 = ADVANCED_FACE ( 'NONE', ( #90080 ), #110377, .T. ) ;
#101299 = AXIS2_PLACEMENT_3D ( 'NONE', #52249, #122285, #40514 ) ;
#101300 = AXIS2_PLACEMENT_3D ( 'NONE', #31415, #1293, #41244 ) ;
#101301 = CARTESIAN_POINT ( 'NONE',  ( -4.999999999999986677, 12.50000000000000000, -2.276824562219559311E-15 ) ) ;
#101302 = ADVANCED_FACE ( 'NONE', ( #10859 ), #89453, .T. ) ;
#101303 = CARTESIAN_POINT ( 'NONE',  ( -4.350000000000023626, 12.50000000000000000, 2.576566944158910744 ) ) ;
#101304 = CARTESIAN_POINT ( 'NONE',  ( 6.649999999999931966, 2.500000000000000000, -5.702370205355749455 ) ) ;
#101305 = CARTESIAN_POINT ( 'NONE',  ( 186.6145833340161175, 6.668395609140177704, -3.849999999999998312 ) ) ;
#101307 = ORIENTED_EDGE ( 'NONE', *, *, #3861, .F. ) ;
#101306 = AXIS2_PLACEMENT_3D ( 'NONE', #59361, #68504, #1692 ) ;
#101308 = DIRECTION ( 'NONE',  ( 0.000000000000000000, 0.000000000000000000, 1.000000000000000000 ) ) ;
#101309 = EDGE_CURVE ( 'NONE', #103801, #126753, #94013, .T. ) ;
#101310 = ORIENTED_EDGE ( 'NONE', *, *, #66656, .F. ) ;
#101311 = FACE_OUTER_BOUND ( 'NONE', #73782, .T. ) ;
#101312 = ORIENTED_EDGE ( 'NONE', *, *, #2526, .T. ) ;
#101313 = CARTESIAN_POINT ( 'NONE',  ( 5.599999999999934808, 2.500000000000000000, -4.576537180435978236 ) ) ;
#101314 = EDGE_LOOP ( 'NONE', ( #86061, #8403 ) ) ;
#101315 = LINE ( 'NONE', #90839, #9510 ) ;
#101316 = CARTESIAN_POINT ( 'NONE',  ( 7.099999999999926814, 2.500000000000000000, -2.276824562219559311E-15 ) ) ;
#101317 = DIRECTION ( 'NONE',  ( -0.000000000000000000, -1.000000000000000000, -0.000000000000000000 ) ) ;
#101318 = DIRECTION ( 'NONE',  ( 0.000000000000000000, -0.9999939076577903929, 0.003490651415223739937 ) ) ;
#101319 = DIRECTION ( 'NONE',  ( -0.000000000000000000, -1.000000000000000000, -0.000000000000000000 ) ) ;
#101320 = AXIS2_PLACEMENT_3D ( 'NONE', #83334, #73483, #45342 ) ;
#101321 = VERTEX_POINT ( 'NONE', #11532 ) ;
#101322 = EDGE_LOOP ( 'NONE', ( #94692, #119295, #115509, #103375 ) ) ;
#101323 = ORIENTED_EDGE ( 'NONE', *, *, #69206, .T. ) ;
#101324 = DIRECTION ( 'NONE',  ( -0.000000000000000000, 1.000000000000000000, -0.000000000000000000 ) ) ;
#101325 = DIRECTION ( 'NONE',  ( 0.000000000000000000, 0.000000000000000000, 1.000000000000000000 ) ) ;
#101326 = DIRECTION ( 'NONE',  ( 0.000000000000000000, 0.000000000000000000, 1.000000000000000000 ) ) ;
#101328 = ORIENTED_EDGE ( 'NONE', *, *, #19974, .T. ) ;
#101327 = ORIENTED_EDGE ( 'NONE', *, *, #49119, .T. ) ;
#101329 = EDGE_LOOP ( 'NONE', ( #104948, #64114, #100995, #110289 ) ) ;
#101330 = CARTESIAN_POINT ( 'NONE',  ( 6.249999999999932498, 2.500000000000000000, -5.702370205355749455 ) ) ;
#101331 = CONICAL_SURFACE ( 'NONE', #63681, 0.1000000000000002554, 0.003490658503988666988 ) ;
#101332 = ORIENTED_EDGE ( 'NONE', *, *, #16609, .F. ) ;
#101333 = DIRECTION ( 'NONE',  ( 0.000000000000000000, 1.000000000000000000, 0.000000000000000000 ) ) ;
#101335 = AXIS2_PLACEMENT_3D ( 'NONE', #13661, #94165, #32050 ) ;
#101334 = DIRECTION ( 'NONE',  ( -0.000000000000000000, -1.000000000000000000, -0.000000000000000000 ) ) ;
#101336 = CARTESIAN_POINT ( 'NONE',  ( -10.85000000000000142, 2.500000000000000000, -7.288010851410851032 ) ) ;
#101337 = DIRECTION ( 'NONE',  ( 0.000000000000000000, 0.000000000000000000, -1.000000000000000000 ) ) ;
#101338 = CARTESIAN_POINT ( 'NONE',  ( 10.39999999999991331, 2.500000000000000000, -0.1000000000000023925 ) ) ;
#101339 = CARTESIAN_POINT ( 'NONE',  ( 11.04999999999990834, 2.500000000000000000, -6.941600689897077459 ) ) ;
#101340 = DIRECTION ( 'NONE',  ( 0.000000000000000000, 0.000000000000000000, 1.000000000000000000 ) ) ;
#101341 = FACE_OUTER_BOUND ( 'NONE', #69627, .T. ) ;
#101342 = ORIENTED_EDGE ( 'NONE', *, *, #91388, .F. ) ;
#101343 = AXIS2_PLACEMENT_3D ( 'NONE', #113459, #62446, #44735 ) ;
#101344 = EDGE_CURVE ( 'NONE', #117711, #27277, #51474, .T. ) ;
#101345 = DIRECTION ( 'NONE',  ( 0.000000000000000000, -0.9999939076577903929, 0.003490651415223739937 ) ) ;
#101348 = EDGE_CURVE ( 'NONE', #40443, #83814, #112322, .T. ) ;
#101347 = CONICAL_SURFACE ( 'NONE', #113861, 0.09999999999999999167, 0.003490658503988666988 ) ;
#101346 = DIRECTION ( 'NONE',  ( 0.000000000000000000, 0.000000000000000000, 1.000000000000000000 ) ) ;
#101349 = EDGE_LOOP ( 'NONE', ( #102579, #8014 ) ) ;
#101350 = VERTEX_POINT ( 'NONE', #124064 ) ;
#101351 = CARTESIAN_POINT ( 'NONE',  ( 186.8385416670080872, 6.551208109652274736, 3.782341765625001351 ) ) ;
#101352 = LINE ( 'NONE', #30039, #48987 ) ;
#101353 = DIRECTION ( 'NONE',  ( 0.000000000000000000, 0.000000000000000000, 1.000000000000000000 ) ) ;
#101354 = DIRECTION ( 'NONE',  ( 0.000000000000000000, 1.000000000000000000, 0.000000000000000000 ) ) ;
#101355 = EDGE_CURVE ( 'NONE', #46558, #92955, #8327, .T. ) ;
#101356 = DIRECTION ( 'NONE',  ( 0.000000000000000000, 1.000000000000000000, 0.000000000000000000 ) ) ;
#101357 = CONICAL_SURFACE ( 'NONE', #82578, 0.09999999999999982514, 0.003490658503988666988 ) ;
#101358 = PLANE ( 'NONE',  #42815 ) ;
#101359 = AXIS2_PLACEMENT_3D ( 'NONE', #2257, #3563, #13377 ) ;
#101360 = CARTESIAN_POINT ( 'NONE',  ( -2.700000000000031264, 12.50000000000000000, 4.676537180435972552 ) ) ;
#101361 = DIRECTION ( 'NONE',  ( 0.000000000000000000, -0.000000000000000000, 1.000000000000000000 ) ) ;
#101362 = CIRCLE ( 'NONE', #57439, 0.1000000000000002554 ) ;
#101363 = CIRCLE ( 'NONE', #97149, 0.1000000000000002554 ) ;
#101364 = FACE_OUTER_BOUND ( 'NONE', #17247, .T. ) ;
#101365 = EDGE_LOOP ( 'NONE', ( #44156, #59316 ) ) ;
#101366 = VERTEX_POINT ( 'NONE', #23280 ) ;
#101367 = EDGE_LOOP ( 'NONE', ( #23338, #24804, #125501, #21601 ) ) ;
#101368 = ORIENTED_EDGE ( 'NONE', *, *, #83322, .T. ) ;
#101369 = DIRECTION ( 'NONE',  ( 0.000000000000000000, -0.000000000000000000, 1.000000000000000000 ) ) ;
#101370 = CARTESIAN_POINT ( 'NONE',  ( -7.700000000000014388, 2.500000000000000000, -4.676537180435977881 ) ) ;
#101371 = ORIENTED_EDGE ( 'NONE', *, *, #73505, .F. ) ;
#101372 = PLANE ( 'NONE',  #128022 ) ;
#101373 = DIRECTION ( 'NONE',  ( 0.000000000000000000, 0.000000000000000000, -1.000000000000000000 ) ) ;
#101374 = CIRCLE ( 'NONE', #44937, 0.1000000000000002554 ) ;
#101375 = DIRECTION ( 'NONE',  ( 0.000000000000000000, 1.000000000000000000, 0.000000000000000000 ) ) ;
#101377 = ORIENTED_EDGE ( 'NONE', *, *, #68482, .F. ) ;
#101376 = FACE_OUTER_BOUND ( 'NONE', #3291, .T. ) ;
#101378 = CONICAL_SURFACE ( 'NONE', #13526, 0.09999999999999982514, 0.003490658503988666988 ) ;
#101379 = FACE_OUTER_BOUND ( 'NONE', #81713, .T. ) ;
#101380 = CARTESIAN_POINT ( 'NONE',  ( -1.650000000000034328, 2.500000000000000000, -2.165063509461101710 ) ) ;
#101381 = EDGE_CURVE ( 'NONE', #71296, #18587, #60593, .T. ) ;
#101382 = ORIENTED_EDGE ( 'NONE', *, *, #14651, .T. ) ;
#101383 = CIRCLE ( 'NONE', #122319, 2.750000000000002665 ) ;
#101384 = CIRCLE ( 'NONE', #88855, 0.06509327318403745899 ) ;
#101385 = AXIS2_PLACEMENT_3D ( 'NONE', #71550, #121948, #23102 ) ;
#101386 = ORIENTED_EDGE ( 'NONE', *, *, #97458, .F. ) ;
#101387 = ORIENTED_EDGE ( 'NONE', *, *, #82218, .T. ) ;
#101388 = VERTEX_POINT ( 'NONE', #122782 ) ;
#101389 = CARTESIAN_POINT ( 'NONE',  ( -10.45000000000000462, 12.50000000000000000, -6.495190528383298911 ) ) ;
#101390 = DIRECTION ( 'NONE',  ( -0.000000000000000000, 1.000000000000000000, -0.000000000000000000 ) ) ;
#101391 = CARTESIAN_POINT ( 'NONE',  ( 2.500000000000001332, -2.392226903609812716, -9.521986658763280431 ) ) ;
#101392 = CIRCLE ( 'NONE', #38723, 0.1000000000000002554 ) ;
#101393 = CIRCLE ( 'NONE', #70091, 0.09999999999999982514 ) ;
#101394 = ORIENTED_EDGE ( 'NONE', *, *, #43661, .T. ) ;
#101396 = AXIS2_PLACEMENT_3D ( 'NONE', #15859, #116000, #95731 ) ;
#101395 = CARTESIAN_POINT ( 'NONE',  ( 2.899999999999944844, 2.500000000000000000, 5.022947341949748790 ) ) ;
#101398 = ORIENTED_EDGE ( 'NONE', *, *, #36160, .F. ) ;
#101397 = EDGE_CURVE ( 'NONE', #46092, #72427, #54312, .T. ) ;
#101399 = DIRECTION ( 'NONE',  ( 0.000000000000000000, 1.000000000000000000, 0.000000000000000000 ) ) ;
#101400 = CARTESIAN_POINT ( 'NONE',  ( 17.19804440726981198, -0.4677972980984271834, -5.492654682185318826 ) ) ;
#101401 = DIRECTION ( 'NONE',  ( 0.000000000000000000, 0.000000000000000000, 1.000000000000000000 ) ) ;
#101402 = DIRECTION ( 'NONE',  ( 0.000000000000000000, 0.000000000000000000, -1.000000000000000000 ) ) ;
#101403 = EDGE_CURVE ( 'NONE', #97815, #24862, #66806, .T. ) ;
#101404 = ORIENTED_EDGE ( 'NONE', *, *, #57059, .T. ) ;
#101405 = ORIENTED_EDGE ( 'NONE', *, *, #46855, .F. ) ;
#101406 = VERTEX_POINT ( 'NONE', #65783 ) ;
#101407 = DIRECTION ( 'NONE',  ( 0.000000000000000000, 0.000000000000000000, 1.000000000000000000 ) ) ;
#101408 = EDGE_CURVE ( 'NONE', #101653, #62839, #98210, .T. ) ;
#101409 = DIRECTION ( 'NONE',  ( 0.000000000000000000, 0.000000000000000000, 1.000000000000000000 ) ) ;
#101410 = FACE_BOUND ( 'NONE', #160, .T. ) ;
#101411 = CARTESIAN_POINT ( 'NONE',  ( 12.09999999999990550, 12.50000000000000000, -3.702399969078687292 ) ) ;
#101412 = AXIS2_PLACEMENT_3D ( 'NONE', #99026, #89201, #11279 ) ;
#101413 = CARTESIAN_POINT ( 'NONE',  ( 0.8499999999999553468, 12.50000000000000000, -2.857883832488653741 ) ) ;
#101414 = DIRECTION ( 'NONE',  ( 0.000000000000000000, 0.000000000000000000, -1.000000000000000000 ) ) ;
#101415 = CARTESIAN_POINT ( 'NONE',  ( 1.649999999999949729, 2.500000000000000000, 5.902370205355745192 ) ) ;
#101416 = CARTESIAN_POINT ( 'NONE',  ( 184.1249999999999716, -8.891194145520236347, -1.633285867636356299E-15 ) ) ;
#101417 = DIRECTION ( 'NONE',  ( 0.000000000000000000, 1.000000000000000000, 0.000000000000000000 ) ) ;
#101418 = EDGE_LOOP ( 'NONE', ( #16758, #50947 ) ) ;
#101419 = VECTOR ( 'NONE', #39655, 1000.000000000000000 ) ;
#101420 = AXIS2_PLACEMENT_3D ( 'NONE', #8995, #87559, #37826 ) ;
#101421 = DIRECTION ( 'NONE',  ( 0.000000000000000000, 0.000000000000000000, 1.000000000000000000 ) ) ;
#101422 = CARTESIAN_POINT ( 'NONE',  ( -6.650000000000018119, 2.500000000000000000, -6.595190528383302109 ) ) ;
#101423 = ORIENTED_EDGE ( 'NONE', *, *, #29737, .T. ) ;
#101424 = ORIENTED_EDGE ( 'NONE', *, *, #15292, .T. ) ;
#101425 = FACE_OUTER_BOUND ( 'NONE', #15127, .T. ) ;
#101426 = PLANE ( 'NONE',  #10987 ) ;
#101427 = FACE_BOUND ( 'NONE', #14642, .T. ) ;
#101428 = DIRECTION ( 'NONE',  ( -0.000000000000000000, 1.000000000000000000, -0.000000000000000000 ) ) ;
#101429 = EDGE_CURVE ( 'NONE', #1020, #54054, #14731, .T. ) ;
#101430 = VERTEX_POINT ( 'NONE', #114246 ) ;
#101431 = DIRECTION ( 'NONE',  ( 0.000000000000000000, 0.000000000000000000, 1.000000000000000000 ) ) ;
#101432 = EDGE_CURVE ( 'NONE', #25321, #68325, #55336, .T. ) ;
#101433 = CARTESIAN_POINT ( 'NONE',  ( 185.2916666666666572, 4.445597072760120838, -7.699999999999998401 ) ) ;
#101434 = EDGE_CURVE ( 'NONE', #67249, #77153, #25065, .T. ) ;
#101435 = EDGE_CURVE ( 'NONE', #55449, #7001, #43867, .T. ) ;
#101436 = EDGE_LOOP ( 'NONE', ( #15789, #92790, #44952, #71785 ) ) ;
#101437 = DIRECTION ( 'NONE',  ( 0.000000000000000000, 0.000000000000000000, -1.000000000000000000 ) ) ;
#101438 = DIRECTION ( 'NONE',  ( 0.000000000000000000, 1.000000000000000000, 0.000000000000000000 ) ) ;
#101439 = AXIS2_PLACEMENT_3D ( 'NONE', #27839, #65824, #87395 ) ;
#101440 = CONICAL_SURFACE ( 'NONE', #38775, 0.1000000000000002554, 0.003490658503988666988 ) ;
#101441 = ADVANCED_FACE ( 'NONE', ( #75596 ), #42966, .T. ) ;
#101442 = ADVANCED_FACE ( 'NONE', ( #4919 ), #84786, .T. ) ;
#101443 = CARTESIAN_POINT ( 'NONE',  ( -3.750000000000025757, 2.500000000000000000, -2.757883832488654097 ) ) ;
#101444 = EDGE_CURVE ( 'NONE', #87657, #106953, #124713, .T. ) ;
#101445 = CARTESIAN_POINT ( 'NONE',  ( 11.44999999999990514, 2.500000000000000000, -6.148780366869526226 ) ) ;
#101446 = ORIENTED_EDGE ( 'NONE', *, *, #75435, .T. ) ;
#101447 = DIRECTION ( 'NONE',  ( 0.000000000000000000, 0.000000000000000000, -1.000000000000000000 ) ) ;
#101448 = EDGE_CURVE ( 'NONE', #122865, #8533, #74326, .T. ) ;
#101449 = CARTESIAN_POINT ( 'NONE',  ( 10.64999999999991331, 2.500000000000000000, 6.048780366869521252 ) ) ;
#101450 = DIRECTION ( 'NONE',  ( 0.000000000000000000, 0.000000000000000000, 1.000000000000000000 ) ) ;
#101451 = ORIENTED_EDGE ( 'NONE', *, *, #27743, .T. ) ;
#101452 = EDGE_LOOP ( 'NONE', ( #60207, #45915 ) ) ;
#101453 = EDGE_CURVE ( 'NONE', #67694, #73914, #114930, .T. ) ;
#101454 = DIRECTION ( 'NONE',  ( 0.000000000000000000, 0.000000000000000000, 1.000000000000000000 ) ) ;
#101455 = VECTOR ( 'NONE', #3286, 1000.000000000000000 ) ;
#101456 = EDGE_CURVE ( 'NONE', #93396, #34419, #94590, .T. ) ;
#101457 = ORIENTED_EDGE ( 'NONE', *, *, #88953, .T. ) ;
#101458 = DIRECTION ( 'NONE',  ( 0.000000000000000000, 0.000000000000000000, 1.000000000000000000 ) ) ;
#101459 = DIRECTION ( 'NONE',  ( 0.000000000000000000, 1.000000000000000000, 0.000000000000000000 ) ) ;
#101461 = CARTESIAN_POINT ( 'NONE',  ( -1.650000000000034328, 12.50000000000000000, -7.253104124594891289 ) ) ;
#101460 = AXIS2_PLACEMENT_3D ( 'NONE', #1621, #50730, #81488 ) ;
#101462 = VERTEX_POINT ( 'NONE', #4268 ) ;
#101463 = CIRCLE ( 'NONE', #93061, 0.06509327318403745899 ) ;
#101464 = DIRECTION ( 'NONE',  ( 0.000000000000000000, 0.000000000000000000, 1.000000000000000000 ) ) ;
#101465 = DIRECTION ( 'NONE',  ( 0.000000000000000000, 0.000000000000000000, 1.000000000000000000 ) ) ;
#101466 = CARTESIAN_POINT ( 'NONE',  ( -13.09999999999999254, 2.500000000000000000, -3.983716857408423628 ) ) ;
#101467 = AXIS2_PLACEMENT_3D ( 'NONE', #55104, #125747, #124495 ) ;
#101468 = DIRECTION ( 'NONE',  ( -4.274815082592931898E-19, -0.9999939076577903929, -0.003490651415223739937 ) ) ;
#101469 = DIRECTION ( 'NONE',  ( 1.000000000000000000, 0.000000000000000000, -0.000000000000000000 ) ) ;
#101470 = CARTESIAN_POINT ( 'NONE',  ( 6.449999999999930012, 2.500000000000000000, 1.718653347947321386 ) ) ;
#101471 = AXIS2_PLACEMENT_3D ( 'NONE', #103603, #124531, #25665 ) ;
#101472 = ORIENTED_EDGE ( 'NONE', *, *, #60269, .F. ) ;
#101474 = ORIENTED_EDGE ( 'NONE', *, *, #36165, .F. ) ;
#101473 = AXIS2_PLACEMENT_3D ( 'NONE', #41113, #81653, #101948 ) ;
#101476 = CARTESIAN_POINT ( 'NONE',  ( 1.649999999999949729, 12.50000000000000000, 7.188010851410848723 ) ) ;
#101475 = CIRCLE ( 'NONE', #28312, 0.06509327318403745899 ) ;
#101477 = ORIENTED_EDGE ( 'NONE', *, *, #92621, .T. ) ;
#101478 = LINE ( 'NONE', #3906, #124599 ) ;
#101481 = ORIENTED_EDGE ( 'NONE', *, *, #63015, .T. ) ;
#101480 = VERTEX_POINT ( 'NONE', #44209 ) ;
#101479 = AXIS2_PLACEMENT_3D ( 'NONE', #74973, #73671, #94597 ) ;
#101482 = EDGE_LOOP ( 'NONE', ( #100393, #12753 ) ) ;
#101483 = DIRECTION ( 'NONE',  ( -0.000000000000000000, 1.000000000000000000, -0.000000000000000000 ) ) ;
#101484 = CIRCLE ( 'NONE', #88861, 0.06509327318403745899 ) ;
#101486 = AXIS2_PLACEMENT_3D ( 'NONE', #31587, #74082, #42719 ) ;
#101485 = CARTESIAN_POINT ( 'NONE',  ( 9.799999999999913669, 2.500000000000000000, -3.983716857408426293 ) ) ;
#101487 = FACE_OUTER_BOUND ( 'NONE', #28388, .T. ) ;
#101488 = VECTOR ( 'NONE', #35484, 1000.000000000000000 ) ;
#101489 = DIRECTION ( 'NONE',  ( 0.000000000000000000, 0.000000000000000000, 1.000000000000000000 ) ) ;
#101490 = CARTESIAN_POINT ( 'NONE',  ( 3.349999999999945466, 2.500000000000000000, -2.857883832488653741 ) ) ;
#101491 = DIRECTION ( 'NONE',  ( -0.000000000000000000, -1.000000000000000000, -0.000000000000000000 ) ) ;
#101492 = CONICAL_SURFACE ( 'NONE', #57663, 0.1000000000000000056, 0.003490658503988666988 ) ;
#101493 = CARTESIAN_POINT ( 'NONE',  ( -6.450000000000016165, 2.500000000000000000, 2.511473670974873507 ) ) ;
#101494 = DIRECTION ( 'NONE',  ( 0.000000000000000000, -0.9999939076577903929, 0.003490651415223739937 ) ) ;
#101495 = CARTESIAN_POINT ( 'NONE',  ( 0.3999999999999568345, 2.500000000000000000, -3.737306695894649700 ) ) ;
#101496 = ORIENTED_EDGE ( 'NONE', *, *, #16989, .T. ) ;
#101497 = EDGE_CURVE ( 'NONE', #5264, #70467, #58534, .T. ) ;
#101498 = EDGE_CURVE ( 'NONE', #81764, #44564, #48062, .T. ) ;
#101499 = DIRECTION ( 'NONE',  ( 0.000000000000000000, 0.000000000000000000, -1.000000000000000000 ) ) ;
#101500 = EDGE_LOOP ( 'NONE', ( #108003, #22852 ) ) ;
#101501 = ORIENTED_EDGE ( 'NONE', *, *, #19659, .F. ) ;
#101502 = DIRECTION ( 'NONE',  ( 0.000000000000000000, 0.000000000000000000, 1.000000000000000000 ) ) ;
#101503 = DIRECTION ( 'NONE',  ( 0.000000000000000000, 0.000000000000000000, 1.000000000000000000 ) ) ;
#101504 = CIRCLE ( 'NONE', #122435, 0.06509327318403745899 ) ;
#101505 = CARTESIAN_POINT ( 'NONE',  ( -11.44999999999999751, 2.500000000000000000, 6.248780366869521430 ) ) ;
#101506 = CARTESIAN_POINT ( 'NONE',  ( 10.39999999999991509, 12.50000000000000000, -0.6277270498435167934 ) ) ;
#101508 = B_SPLINE_SURFACE_WITH_KNOTS ( 'NONE', 3, 1, ( 
 ( #96283, #46542 ),
 ( #86470, #126406 ),
 ( #36754, #76663 ),
 ( #77943, #19008 ),
 ( #68763, #60267 ),
 ( #118507, #98223 ),
 ( #39966, #40629 ),
 ( #109338, #79250 ),
 ( #49795, #97581 ),
 ( #38695, #79880 ),
 ( #80536, #120451 ),
 ( #119804, #69403 ),
 ( #47857, #30801 ),
 ( #88391, #25 ),
 ( #17719, #87753 ),
 ( #70703, #57673 ),
 ( #18373, #29499 ),
 ( #58958, #89699 ) ),
 .UNSPECIFIED., .F., .F., .F.,
 ( 4, 2, 2, 2, 2, 2, 2, 2, 4 ),
 ( 2, 2 ),
 ( 0.000000000000000000, 0.1250000000000000000, 0.2500000000000000000, 0.3750000000000000000, 0.5000000000000000000, 0.6250000000000000000, 0.7500000000000000000, 0.8750000000000000000, 1.000000000000000000 ),
 ( 0.000000000000000000, 1.000000000000000000 ),
 .UNSPECIFIED. ) ;
#101507 = CARTESIAN_POINT ( 'NONE',  ( -5.400000000000024336, 2.500000000000000000, -3.537306695894649966 ) ) ;
#101509 = DIRECTION ( 'NONE',  ( -0.000000000000000000, -1.000000000000000000, -0.000000000000000000 ) ) ;
#101510 = PLANE ( 'NONE',  #69814 ) ;
#101511 = EDGE_LOOP ( 'NONE', ( #118269, #33907, #45507, #58744 ) ) ;
#101512 = AXIS2_PLACEMENT_3D ( 'NONE', #4037, #5963, #105476 ) ;
#101513 = CIRCLE ( 'NONE', #120292, 0.06509327318403745899 ) ;
#101514 = AXIS2_PLACEMENT_3D ( 'NONE', #47500, #7551, #97234 ) ;
#101515 = EDGE_LOOP ( 'NONE', ( #72917, #55387, #126677, #79019 ) ) ;
#101516 = VERTEX_POINT ( 'NONE', #97188 ) ;
#101517 = ORIENTED_EDGE ( 'NONE', *, *, #48973, .F. ) ;
#101518 = ORIENTED_EDGE ( 'NONE', *, *, #110324, .T. ) ;
#101519 = DIRECTION ( 'NONE',  ( -4.274815082592931898E-19, -0.9999939076577903929, -0.003490651415223739937 ) ) ;
#101520 = DIRECTION ( 'NONE',  ( 0.000000000000000000, 0.000000000000000000, 1.000000000000000000 ) ) ;
#101521 = VECTOR ( 'NONE', #57619, 1000.000000000000000 ) ;
#101522 = DIRECTION ( 'NONE',  ( 0.000000000000000000, 0.000000000000000000, 1.000000000000000000 ) ) ;
#101523 = DIRECTION ( 'NONE',  ( 0.000000000000000000, 0.000000000000000000, 1.000000000000000000 ) ) ;
#101524 = CIRCLE ( 'NONE', #42971, 0.1000000000000000472 ) ;
#101525 = FACE_OUTER_BOUND ( 'NONE', #81813, .T. ) ;
#101526 = ORIENTED_EDGE ( 'NONE', *, *, #108527, .F. ) ;
#101527 = PLANE ( 'NONE',  #20661 ) ;
#101528 = DIRECTION ( 'NONE',  ( 0.000000000000000000, 0.000000000000000000, 1.000000000000000000 ) ) ;
#101529 = DIRECTION ( 'NONE',  ( -0.000000000000000000, 1.000000000000000000, -0.000000000000000000 ) ) ;
#101530 = DIRECTION ( 'NONE',  ( 0.000000000000000000, -0.000000000000000000, 1.000000000000000000 ) ) ;
#101531 = CARTESIAN_POINT ( 'NONE',  ( -1.650000000000034328, 12.50000000000000000, -7.188010851410854052 ) ) ;
#101532 = EDGE_CURVE ( 'NONE', #84837, #92462, #121201, .T. ) ;
#101533 = ORIENTED_EDGE ( 'NONE', *, *, #128490, .T. ) ;
#101534 = CIRCLE ( 'NONE', #17894, 0.1000000000000002554 ) ;
#101535 = CIRCLE ( 'NONE', #5378, 0.09999999999999982514 ) ;
#101536 = ORIENTED_EDGE ( 'NONE', *, *, #72801, .F. ) ;
#101537 = VERTEX_POINT ( 'NONE', #125985 ) ;
#101538 = CARTESIAN_POINT ( 'NONE',  ( -3.100000000000028955, 2.500000000000000000, 4.776537180435972196 ) ) ;
#101539 = ORIENTED_EDGE ( 'NONE', *, *, #111957, .F. ) ;
#101540 = DIRECTION ( 'NONE',  ( -4.274815082592931898E-19, -0.9999939076577903929, -0.003490651415223739937 ) ) ;
#101542 = ADVANCED_FACE ( 'NONE', ( #57267 ), #106531, .T. ) ;
#101541 = DIRECTION ( 'NONE',  ( 0.000000000000000000, 0.000000000000000000, 1.000000000000000000 ) ) ;
#101544 = ORIENTED_EDGE ( 'NONE', *, *, #46690, .F. ) ;
#101543 = EDGE_CURVE ( 'NONE', #128383, #106389, #64766, .T. ) ;
#101545 = CARTESIAN_POINT ( 'NONE',  ( 184.1250000000000284, -8.891194145520236347, -1.633285867636356693E-15 ) ) ;
#101546 = DIRECTION ( 'NONE',  ( 0.000000000000000000, 0.000000000000000000, -1.000000000000000000 ) ) ;
#101547 = LINE ( 'NONE', #20413, #115100 ) ;
#101548 = EDGE_CURVE ( 'NONE', #55365, #110679, #71039, .T. ) ;
#101549 = CARTESIAN_POINT ( 'NONE',  ( -11.44999999999999929, 2.500000000000000000, -6.048780366869523029 ) ) ;
#101550 = VECTOR ( 'NONE', #12580, 1000.000000000000000 ) ;
#101551 = CARTESIAN_POINT ( 'NONE',  ( -13.14999999999999147, 2.500000000000000000, -1.818653347947323917 ) ) ;
#101552 = EDGE_CURVE ( 'NONE', #32372, #94402, #46148, .T. ) ;
#101553 = AXIS2_PLACEMENT_3D ( 'NONE', #6664, #56435, #93803 ) ;
#101554 = ORIENTED_EDGE ( 'NONE', *, *, #43832, .T. ) ;
#101555 = B_SPLINE_CURVE_WITH_KNOTS ( 'NONE', 3,
 ( #15054, #94288, #82563, #32186, #112015, #2677 ),
 .UNSPECIFIED., .F., .F.,
 ( 4, 2, 4 ),
 ( 0.000000000000000000, 0.002961986837177525006, 0.005923973674355050012 ),
 .UNSPECIFIED. ) ;
#101556 = ORIENTED_EDGE ( 'NONE', *, *, #9143, .T. ) ;
#101557 = EDGE_CURVE ( 'NONE', #102950, #117733, #83567, .T. ) ;
#101558 = LINE ( 'NONE', #33471, #64730 ) ;
#101559 = CARTESIAN_POINT ( 'NONE',  ( -13.74999999999998934, 2.500000000000000000, 2.957883832488652942 ) ) ;
#101560 = DIRECTION ( 'NONE',  ( -0.000000000000000000, 1.000000000000000000, -0.000000000000000000 ) ) ;
#101561 = DIRECTION ( 'NONE',  ( 0.000000000000000000, 0.000000000000000000, -1.000000000000000000 ) ) ;
#101562 = VERTEX_POINT ( 'NONE', #126654 ) ;
#101563 = CIRCLE ( 'NONE', #124559, 0.1000000000000002554 ) ;
#101564 = VERTEX_POINT ( 'NONE', #117435 ) ;
#101565 = DIRECTION ( 'NONE',  ( -4.274815082592931898E-19, -0.9999939076577903929, -0.003490651415223739937 ) ) ;
#101566 = DIRECTION ( 'NONE',  ( 0.000000000000000000, 1.000000000000000000, 0.000000000000000000 ) ) ;
#101567 = DIRECTION ( 'NONE',  ( 0.000000000000000000, -0.000000000000000000, 1.000000000000000000 ) ) ;
#101568 = FACE_OUTER_BOUND ( 'NONE', #73544, .T. ) ;
#101569 = VERTEX_POINT ( 'NONE', #128615 ) ;
#101570 = AXIS2_PLACEMENT_3D ( 'NONE', #39570, #20548, #21849 ) ;
#101571 = CIRCLE ( 'NONE', #118286, 0.09999999999999982514 ) ;
#101572 = DIRECTION ( 'NONE',  ( 0.000000000000000000, 0.000000000000000000, 1.000000000000000000 ) ) ;
#101573 = FACE_OUTER_BOUND ( 'NONE', #118871, .T. ) ;
#101574 = AXIS2_PLACEMENT_3D ( 'NONE', #119080, #11038, #52275 ) ;
#101575 = ORIENTED_EDGE ( 'NONE', *, *, #57402, .F. ) ;
#101576 = DIRECTION ( 'NONE',  ( -0.000000000000000000, 1.000000000000000000, -0.000000000000000000 ) ) ;
#101577 = EDGE_LOOP ( 'NONE', ( #99679, #32553, #39399, #36504 ) ) ;
#101578 = CARTESIAN_POINT ( 'NONE',  ( -6.650000000000015454, 2.500000000000000000, 7.088010851410848190 ) ) ;
#101579 = ORIENTED_EDGE ( 'NONE', *, *, #12176, .F. ) ;
#101580 = ADVANCED_FACE ( 'NONE', ( #78859 ), #87739, .T. ) ;
#101581 = ORIENTED_EDGE ( 'NONE', *, *, #36344, .T. ) ;
#101582 = DIRECTION ( 'NONE',  ( -0.000000000000000000, -1.000000000000000000, -0.000000000000000000 ) ) ;
#101583 = DIRECTION ( 'NONE',  ( -0.000000000000000000, -1.000000000000000000, -0.000000000000000000 ) ) ;
#101584 = EDGE_LOOP ( 'NONE', ( #9661, #74054, #88160, #21811 ) ) ;
#101585 = EDGE_LOOP ( 'NONE', ( #46850, #88351 ) ) ;
#101586 = EDGE_CURVE ( 'NONE', #53470, #101913, #29113, .T. ) ;
#101587 = CARTESIAN_POINT ( 'NONE',  ( -11.24999999999996447, 2.500000000000000000, -2.265063509461097802 ) ) ;
#101588 = CYLINDRICAL_SURFACE ( 'NONE', #37329, 2.749999999999997335 ) ;
#101589 = AXIS2_PLACEMENT_3D ( 'NONE', #81789, #32082, #71998 ) ;
#101590 = EDGE_CURVE ( 'NONE', #94018, #35080, #116815, .T. ) ;
#101591 = DIRECTION ( 'NONE',  ( 0.000000000000000000, 0.000000000000000000, -1.000000000000000000 ) ) ;
#101592 = CARTESIAN_POINT ( 'NONE',  ( 184.6510416670080588, 4.367472073101518859, -7.564683531249999149 ) ) ;
#101593 = DIRECTION ( 'NONE',  ( 0.000000000000000000, 1.000000000000000000, 0.000000000000000000 ) ) ;
#101594 = CARTESIAN_POINT ( 'NONE',  ( 130.5000000000000000, 0.5000000000000000000, -7.500000000000001776 ) ) ;
#101595 = CARTESIAN_POINT ( 'NONE',  ( 9.999999999999914735, 12.50000000000000000, 0.6928203230275494784 ) ) ;
#101596 = EDGE_CURVE ( 'NONE', #65177, #34926, #18791, .T. ) ;
#101597 = ADVANCED_FACE ( 'NONE', ( #57920 ), #125411, .T. ) ;
#101598 = DIRECTION ( 'NONE',  ( -0.000000000000000000, -1.000000000000000000, -0.000000000000000000 ) ) ;
#101599 = AXIS2_PLACEMENT_3D ( 'NONE', #103390, #83112, #125585 ) ;
#101600 = CARTESIAN_POINT ( 'NONE',  ( -11.05000000000000071, 12.50000000000000000, -2.511473670974873951 ) ) ;
#101601 = ADVANCED_FACE ( 'NONE', ( #27155 ), #29279, .T. ) ;
#101602 = CIRCLE ( 'NONE', #22294, 0.06509327318403743123 ) ;
#101603 = EDGE_CURVE ( 'NONE', #31883, #45092, #85696, .T. ) ;
#101604 = AXIS2_PLACEMENT_3D ( 'NONE', #111567, #120741, #21245 ) ;
#101605 = VERTEX_POINT ( 'NONE', #8791 ) ;
#101606 = CIRCLE ( 'NONE', #17968, 0.1000000000000002554 ) ;
#101607 = ORIENTED_EDGE ( 'NONE', *, *, #104284, .T. ) ;
#101608 = DIRECTION ( 'NONE',  ( 0.000000000000000000, 1.000000000000000000, 0.000000000000000000 ) ) ;
#101609 = EDGE_CURVE ( 'NONE', #108744, #104158, #6839, .T. ) ;
#101610 = EDGE_LOOP ( 'NONE', ( #124414, #42867, #116296, #89971 ) ) ;
#101611 = DIRECTION ( 'NONE',  ( 0.000000000000000000, 0.000000000000000000, -1.000000000000000000 ) ) ;
#101612 = CARTESIAN_POINT ( 'NONE',  ( -8.750000000000010658, 2.500000000000000000, 2.857883832488649301 ) ) ;
#101613 = DIRECTION ( 'NONE',  ( 0.000000000000000000, 1.000000000000000000, 0.000000000000000000 ) ) ;
#101615 = ORIENTED_EDGE ( 'NONE', *, *, #92411, .F. ) ;
#101614 = EDGE_LOOP ( 'NONE', ( #107397, #77114 ) ) ;
#101616 = FACE_BOUND ( 'NONE', #48249, .T. ) ;
#101617 = ORIENTED_EDGE ( 'NONE', *, *, #111016, .T. ) ;
#101618 = DIRECTION ( 'NONE',  ( 0.000000000000000000, 0.000000000000000000, -1.000000000000000000 ) ) ;
#101619 = CARTESIAN_POINT ( 'NONE',  ( -7.300000000000016698, 2.500000000000000000, -4.676537180435978769 ) ) ;
#101620 = EDGE_CURVE ( 'NONE', #72103, #57756, #119147, .T. ) ;
#101621 = AXIS2_PLACEMENT_3D ( 'NONE', #40417, #69194, #118308 ) ;
#101622 = DIRECTION ( 'NONE',  ( -4.274815082592931898E-19, -0.9999939076577903929, -0.003490651415223739937 ) ) ;
#101623 = DIRECTION ( 'NONE',  ( 0.000000000000000000, 0.000000000000000000, -1.000000000000000000 ) ) ;
#101624 = CARTESIAN_POINT ( 'NONE',  ( 10.79999999999991012, 2.500000000000000000, -4.430127018922202176 ) ) ;
#101626 = CONICAL_SURFACE ( 'NONE', #9670, 0.1000000000000000472, 0.003490658503988666988 ) ;
#101625 = AXIS2_PLACEMENT_3D ( 'NONE', #6449, #55591, #57533 ) ;
#101627 = CARTESIAN_POINT ( 'NONE',  ( 9.149999999999915090, 12.50000000000000000, 6.560283801567334372 ) ) ;
#101628 = CARTESIAN_POINT ( 'NONE',  ( 1.649999999999951950, 2.500000000000000000, -5.802370205355749988 ) ) ;
#101629 = FACE_OUTER_BOUND ( 'NONE', #120234, .T. ) ;
#101630 = CARTESIAN_POINT ( 'NONE',  ( 11.69999999999990514, 2.500000000000000000, 0.09999999999999772959 ) ) ;
#101631 = CARTESIAN_POINT ( 'NONE',  ( 9.549999999999915445, 2.500000000000000000, 6.595190528383296780 ) ) ;
#101632 = DIRECTION ( 'NONE',  ( -4.274815082592931898E-19, -0.9999939076577903929, -0.003490651415223739937 ) ) ;
#101633 = ORIENTED_EDGE ( 'NONE', *, *, #112188, .F. ) ;
#101634 = ORIENTED_EDGE ( 'NONE', *, *, #102486, .F. ) ;
#101635 = ORIENTED_EDGE ( 'NONE', *, *, #107523, .T. ) ;
#101636 = ORIENTED_EDGE ( 'NONE', *, *, #11245, .T. ) ;
#101637 = CARTESIAN_POINT ( 'NONE',  ( 12.49999999999990408, 12.50000000000000000, 5.088040615133786027 ) ) ;
#101638 = DIRECTION ( 'NONE',  ( 0.000000000000000000, -0.9999939076577903929, 0.003490651415223739937 ) ) ;
#101640 = ORIENTED_EDGE ( 'NONE', *, *, #115704, .F. ) ;
#101639 = ORIENTED_EDGE ( 'NONE', *, *, #78989, .T. ) ;
#101641 = EDGE_LOOP ( 'NONE', ( #123659, #47851, #129579, #105139 ) ) ;
#101642 = LINE ( 'NONE', #123830, #29255 ) ;
#101643 = CARTESIAN_POINT ( 'NONE',  ( -2.500000000000030642, 2.500000000000000000, -0.5928203230275541635 ) ) ;
#101644 = CARTESIAN_POINT ( 'NONE',  ( 12.89999999999990088, 12.50000000000000000, 4.330127018922196314 ) ) ;
#101645 = DIRECTION ( 'NONE',  ( 0.000000000000000000, 1.000000000000000000, 0.000000000000000000 ) ) ;
#101646 = CARTESIAN_POINT ( 'NONE',  ( -0.4000000000000396572, 2.500000000000000000, 4.230127018922196669 ) ) ;
#101647 = CARTESIAN_POINT ( 'NONE',  ( -1.900000000000034106, 2.500000000000000000, 0.3464101615137735735 ) ) ;
#101648 = ADVANCED_FACE ( 'NONE', ( #47448 ), #96242, .T. ) ;
#101649 = ORIENTED_EDGE ( 'NONE', *, *, #113177, .F. ) ;
#101650 = DIRECTION ( 'NONE',  ( 0.000000000000000000, 1.000000000000000000, 0.000000000000000000 ) ) ;
#101651 = ORIENTED_EDGE ( 'NONE', *, *, #27775, .T. ) ;
#101653 = VERTEX_POINT ( 'NONE', #118108 ) ;
#101652 = AXIS2_PLACEMENT_3D ( 'NONE', #113366, #45291, #74740 ) ;
#101654 = ADVANCED_FACE ( 'NONE', ( #28460, #68362 ), #108290, .T. ) ;
#101655 = ORIENTED_EDGE ( 'NONE', *, *, #79518, .F. ) ;
#101656 = VECTOR ( 'NONE', #107485, 1000.000000000000000 ) ;
#101657 = CARTESIAN_POINT ( 'NONE',  ( 185.2395833340161460, 4.445597072760175905, 7.699999999999896261 ) ) ;
#101658 = VERTEX_POINT ( 'NONE', #79493 ) ;
#101659 = EDGE_LOOP ( 'NONE', ( #277, #25139, #89860, #60824 ) ) ;
#101660 = ORIENTED_EDGE ( 'NONE', *, *, #3121, .T. ) ;
#101661 = CARTESIAN_POINT ( 'NONE',  ( 9.549999999999915445, 12.50000000000000000, -2.099970236277064473 ) ) ;
#101662 = AXIS2_PLACEMENT_3D ( 'NONE', #86718, #38943, #99126 ) ;
#101663 = ADVANCED_FACE ( 'NONE', ( #61132 ), #79540, .T. ) ;
#101664 = DIRECTION ( 'NONE',  ( 0.000000000000000000, 0.000000000000000000, -1.000000000000000000 ) ) ;
#101665 = CARTESIAN_POINT ( 'NONE',  ( -14.14999999999998614, 2.500000000000000000, 1.572243186433549544 ) ) ;
#101666 = CARTESIAN_POINT ( 'NONE',  ( -4.800000000000028244, 2.500000000000000000, -3.983716857408426293 ) ) ;
#101667 = FACE_OUTER_BOUND ( 'NONE', #73445, .T. ) ;
#101668 = DIRECTION ( 'NONE',  ( 0.000000000000000000, 1.000000000000000000, 0.000000000000000000 ) ) ;
#101669 = CARTESIAN_POINT ( 'NONE',  ( -11.05000000000000071, 2.500000000000000000, -2.611473670974873595 ) ) ;
#101671 = AXIS2_PLACEMENT_3D ( 'NONE', #59738, #17847, #57788 ) ;
#101670 = AXIS2_PLACEMENT_3D ( 'NONE', #15200, #3476, #103622 ) ;
#101672 = EDGE_LOOP ( 'NONE', ( #64611, #76391, #110966, #40049 ) ) ;
#101673 = DIRECTION ( 'NONE',  ( -0.000000000000000000, 1.000000000000000000, -0.000000000000000000 ) ) ;
#101674 = AXIS2_PLACEMENT_3D ( 'NONE', #22929, #62217, #43226 ) ;
#101675 = VERTEX_POINT ( 'NONE', #82049 ) ;
#101676 = FACE_OUTER_BOUND ( 'NONE', #72555, .T. ) ;
#101677 = VERTEX_POINT ( 'NONE', #31052 ) ;
#101678 = CARTESIAN_POINT ( 'NONE',  ( 8.949999999999921130, 2.500000000000000000, 1.718653347947321386 ) ) ;
#101679 = EDGE_LOOP ( 'NONE', ( #86372, #4478, #27978, #86265 ) ) ;
#101680 = CARTESIAN_POINT ( 'NONE',  ( 3.349999999999945466, 12.50000000000000000, -6.495190528383302464 ) ) ;
#101681 = CARTESIAN_POINT ( 'NONE',  ( -6.650000000000018119, 2.500000000000000000, -7.288010851410854585 ) ) ;
#101682 = ORIENTED_EDGE ( 'NONE', *, *, #28316, .T. ) ;
#101683 = ORIENTED_EDGE ( 'NONE', *, *, #22987, .F. ) ;
#101684 = FACE_OUTER_BOUND ( 'NONE', #25766, .T. ) ;
#101685 = CARTESIAN_POINT ( 'NONE',  ( 4.149999999999939959, 2.500000000000000000, 1.472243186433545459 ) ) ;
#101686 = LINE ( 'NONE', #129239, #68885 ) ;
#101687 = AXIS2_PLACEMENT_3D ( 'NONE', #46377, #86299, #36597 ) ;
#101688 = DIRECTION ( 'NONE',  ( -0.000000000000000000, 1.000000000000000000, -0.000000000000000000 ) ) ;
#101689 = CARTESIAN_POINT ( 'NONE',  ( -9.200000000000009948, 2.500000000000000000, -4.430127018922197735 ) ) ;
#101690 = ORIENTED_EDGE ( 'NONE', *, *, #108666, .F. ) ;
#101691 = CONICAL_SURFACE ( 'NONE', #78712, 0.1000000000000000472, 0.003490658503988666988 ) ;
#101692 = VECTOR ( 'NONE', #17271, 1000.000000000000000 ) ;
#101693 = DIRECTION ( 'NONE',  ( 0.000000000000000000, -0.9999939076577903929, 0.003490651415223739937 ) ) ;
#101694 = AXIS2_PLACEMENT_3D ( 'NONE', #96135, #9036, #47696 ) ;
#101695 = AXIS2_PLACEMENT_3D ( 'NONE', #45897, #118335, #74705 ) ;
#101696 = ORIENTED_EDGE ( 'NONE', *, *, #40689, .F. ) ;
#101697 = VECTOR ( 'NONE', #106886, 1000.000000000000000 ) ;
#101698 = PLANE ( 'NONE',  #17214 ) ;
#101700 = EDGE_CURVE ( 'NONE', #55696, #9421, #75321, .T. ) ;
#101699 = DIRECTION ( 'NONE',  ( 0.000000000000000000, 0.000000000000000000, -1.000000000000000000 ) ) ;
#101701 = AXIS2_PLACEMENT_3D ( 'NONE', #65348, #124931, #117016 ) ;
#101702 = ADVANCED_FACE ( 'NONE', ( #99129 ), #112980, .T. ) ;
#101703 = ADVANCED_FACE ( 'NONE', ( #121988 ), #18887, .T. ) ;
#101704 = DIRECTION ( 'NONE',  ( -4.274815082592931898E-19, -0.9999939076577903929, -0.003490651415223739937 ) ) ;
#101705 = CARTESIAN_POINT ( 'NONE',  ( 184.5000000000000000, 0.000000000000000000, 0.000000000000000000 ) ) ;
#101706 = DIRECTION ( 'NONE',  ( 0.000000000000000000, 0.000000000000000000, 1.000000000000000000 ) ) ;
#101707 = DIRECTION ( 'NONE',  ( 1.000000000000000000, -0.000000000000000000, -0.000000000000000000 ) ) ;
#101708 = ADVANCED_FACE ( 'NONE', ( #21201 ), #115024, .T. ) ;
#101709 = FACE_OUTER_BOUND ( 'NONE', #87284, .T. ) ;
#101710 = VERTEX_POINT ( 'NONE', #109594 ) ;
#101711 = AXIS2_PLACEMENT_3D ( 'NONE', #41702, #64373, #61978 ) ;
#101712 = CARTESIAN_POINT ( 'NONE',  ( 184.3750000000000000, 8.891194145520236347, 5.444286225454521982E-16 ) ) ;
#101714 = CIRCLE ( 'NONE', #97500, 0.06509327318403745899 ) ;
#101713 = AXIS2_PLACEMENT_3D ( 'NONE', #102592, #54779, #114351 ) ;
#101715 = CARTESIAN_POINT ( 'NONE',  ( 4.349999999999939249, 12.50000000000000000, 2.511473670974873507 ) ) ;
#101716 = CARTESIAN_POINT ( 'NONE',  ( -9.600000000000008527, 2.500000000000000000, 0.09999999999999761857 ) ) ;
#101717 = EDGE_CURVE ( 'NONE', #113506, #76961, #64853, .T. ) ;
#101718 = ORIENTED_EDGE ( 'NONE', *, *, #26216, .T. ) ;
#101719 = ADVANCED_FACE ( 'NONE', ( #59872 ), #917, .T. ) ;
#101720 = ORIENTED_EDGE ( 'NONE', *, *, #87357, .T. ) ;
#101721 = CARTESIAN_POINT ( 'NONE',  ( -5.850000000000018296, 2.500000000000000000, 7.188010851410848723 ) ) ;
#101722 = VERTEX_POINT ( 'NONE', #50050 ) ;
#101723 = ORIENTED_EDGE ( 'NONE', *, *, #53279, .T. ) ;
#101724 = CARTESIAN_POINT ( 'NONE',  ( -13.74999999999998934, 2.500000000000000000, -1.472243186433547901 ) ) ;
#101725 = ORIENTED_EDGE ( 'NONE', *, *, #68146, .F. ) ;
#101726 = CARTESIAN_POINT ( 'NONE',  ( -1.850000000000033840, 12.50000000000000000, 2.446380397790835826 ) ) ;
#101727 = DIRECTION ( 'NONE',  ( -0.000000000000000000, 1.000000000000000000, -0.000000000000000000 ) ) ;
#101728 = CARTESIAN_POINT ( 'NONE',  ( 16.84158739990463616, 0.4722467112504742937, 5.802037699229681600 ) ) ;
#101729 = ORIENTED_EDGE ( 'NONE', *, *, #12566, .T. ) ;
#101730 = CARTESIAN_POINT ( 'NONE',  ( -14.34999999999998543, 2.500000000000000000, 2.511473670974877503 ) ) ;
#101731 = DIRECTION ( 'NONE',  ( -0.000000000000000000, -1.000000000000000000, -0.000000000000000000 ) ) ;
#101732 = ORIENTED_EDGE ( 'NONE', *, *, #91041, .T. ) ;
#101733 = AXIS2_PLACEMENT_3D ( 'NONE', #90331, #677, #40640 ) ;
#101734 = EDGE_LOOP ( 'NONE', ( #33153, #124008 ) ) ;
#101735 = CIRCLE ( 'NONE', #62033, 0.1000000000000000472 ) ;
#101736 = ORIENTED_EDGE ( 'NONE', *, *, #62556, .F. ) ;
#101737 = CARTESIAN_POINT ( 'NONE',  ( 2.099999999999948574, 12.50000000000000000, 4.330127018922196314 ) ) ;
#101738 = DIRECTION ( 'NONE',  ( 0.000000000000000000, 0.000000000000000000, 1.000000000000000000 ) ) ;
#101739 = DIRECTION ( 'NONE',  ( 0.000000000000000000, -0.000000000000000000, 1.000000000000000000 ) ) ;
#101740 = FACE_BOUND ( 'NONE', #126316, .T. ) ;
#101741 = ORIENTED_EDGE ( 'NONE', *, *, #1542, .T. ) ;
#101742 = DIRECTION ( 'NONE',  ( 0.000000000000000000, 0.000000000000000000, -1.000000000000000000 ) ) ;
#101743 = CARTESIAN_POINT ( 'NONE',  ( 8.549999999999924327, 2.500000000000000000, -6.941600689897077459 ) ) ;
#101744 = ORIENTED_EDGE ( 'NONE', *, *, #112275, .F. ) ;
#101746 = CONICAL_SURFACE ( 'NONE', #126793, 0.1000000000000000472, 0.003490658503988666988 ) ;
#101745 = VECTOR ( 'NONE', #113942, 1000.000000000000000 ) ;
#101747 = CARTESIAN_POINT ( 'NONE',  ( 0.8499999999999536815, 2.500000000000000000, 5.802370205355744659 ) ) ;
#101748 = DIRECTION ( 'NONE',  ( -0.000000000000000000, -1.000000000000000000, -0.000000000000000000 ) ) ;
#101750 = ADVANCED_FACE ( 'NONE', ( #89936 ), #69061, .T. ) ;
#101749 = CARTESIAN_POINT ( 'NONE',  ( 2.499999999999948930, 2.500000000000000000, -0.7928203230275542301 ) ) ;
#101751 = CARTESIAN_POINT ( 'NONE',  ( 9.799999999999915445, 12.50000000000000000, 3.983716857408420964 ) ) ;
#101752 = CARTESIAN_POINT ( 'NONE',  ( 2.899999999999946620, 2.500000000000000000, -3.637306695894650055 ) ) ;
#101753 = EDGE_CURVE ( 'NONE', #59442, #31405, #23105, .T. ) ;
#101754 = FACE_OUTER_BOUND ( 'NONE', #73946, .T. ) ;
#101755 = CARTESIAN_POINT ( 'NONE',  ( -4.550000000000022915, 2.500000000000000000, 2.265063509461097357 ) ) ;
#101756 = ADVANCED_FACE ( 'NONE', ( #40209 ), #71120, .T. ) ;
#101757 = AXIS2_PLACEMENT_3D ( 'NONE', #79394, #106263, #108186 ) ;
#101758 = VERTEX_POINT ( 'NONE', #40875 ) ;
#101759 = ORIENTED_EDGE ( 'NONE', *, *, #50899, .F. ) ;
#101761 = ORIENTED_EDGE ( 'NONE', *, *, #87631, .T. ) ;
#101760 = ADVANCED_FACE ( 'NONE', ( #120054 ), #123358, .T. ) ;
#101762 = EDGE_LOOP ( 'NONE', ( #44905, #40621, #77337, #16571 ) ) ;
#101763 = CARTESIAN_POINT ( 'NONE',  ( 1.249999999999950262, 2.500000000000000000, 7.288010851410849256 ) ) ;
#101764 = DIRECTION ( 'NONE',  ( -4.274815082592931898E-19, -0.9999939076577903929, -0.003490651415223739937 ) ) ;
#101765 = ORIENTED_EDGE ( 'NONE', *, *, #12913, .F. ) ;
#101766 = FACE_BOUND ( 'NONE', #83553, .T. ) ;
#101767 = DIRECTION ( 'NONE',  ( 0.000000000000000000, -0.000000000000000000, 1.000000000000000000 ) ) ;
#101768 = DIRECTION ( 'NONE',  ( 0.000000000000000000, 0.000000000000000000, 1.000000000000000000 ) ) ;
#101769 = ADVANCED_FACE ( 'NONE', ( #81426 ), #77390, .T. ) ;
#101770 = CARTESIAN_POINT ( 'NONE',  ( -1.650000000000035660, 2.500000000000000000, 2.857883832488649301 ) ) ;
#101771 = ADVANCED_FACE ( 'NONE', ( #61792 ), #110230, .F. ) ;
#101772 = CARTESIAN_POINT ( 'NONE',  ( 9.199999999999915801, 12.50000000000000000, -4.330127018922201643 ) ) ;
#101773 = DIRECTION ( 'NONE',  ( 0.000000000000000000, 0.000000000000000000, 1.000000000000000000 ) ) ;
#101774 = DIRECTION ( 'NONE',  ( 0.000000000000000000, 0.000000000000000000, 1.000000000000000000 ) ) ;
#101775 = DIRECTION ( 'NONE',  ( -0.000000000000000000, 1.000000000000000000, -0.000000000000000000 ) ) ;
#101776 = DIRECTION ( 'NONE',  ( 0.000000000000000000, 0.000000000000000000, -1.000000000000000000 ) ) ;
#101777 = DIRECTION ( 'NONE',  ( 0.000000000000000000, 1.000000000000000000, 0.000000000000000000 ) ) ;
#101779 = ORIENTED_EDGE ( 'NONE', *, *, #8141, .T. ) ;
#101778 = AXIS2_PLACEMENT_3D ( 'NONE', #127386, #57349, #37715 ) ;
#101781 = EDGE_CURVE ( 'NONE', #26275, #44931, #39853, .T. ) ;
#101780 = VECTOR ( 'NONE', #96289, 1000.000000000000000 ) ;
#101782 = AXIS2_PLACEMENT_3D ( 'NONE', #72171, #23059, #62979 ) ;
#101783 = ORIENTED_EDGE ( 'NONE', *, *, #27117, .F. ) ;
#101784 = ORIENTED_EDGE ( 'NONE', *, *, #118755, .F. ) ;
#101786 = VERTEX_POINT ( 'NONE', #100414 ) ;
#101785 = AXIS2_PLACEMENT_3D ( 'NONE', #18491, #19115, #17173 ) ;
#101787 = VERTEX_POINT ( 'NONE', #10711 ) ;
#101788 = ORIENTED_EDGE ( 'NONE', *, *, #18579, .T. ) ;
#101789 = ORIENTED_EDGE ( 'NONE', *, *, #8869, .T. ) ;
#101790 = DIRECTION ( 'NONE',  ( 0.000000000000000000, 0.000000000000000000, 1.000000000000000000 ) ) ;
#101791 = ORIENTED_EDGE ( 'NONE', *, *, #122283, .F. ) ;
#101793 = EDGE_LOOP ( 'NONE', ( #24677, #90333, #122324, #125652 ) ) ;
#101792 = CIRCLE ( 'NONE', #43305, 0.09999999999999982514 ) ;
#101794 = CIRCLE ( 'NONE', #118492, 0.06509327318403745899 ) ;
#101795 = CIRCLE ( 'NONE', #36951, 0.1000000000000000472 ) ;
#101796 = DIRECTION ( 'NONE',  ( 0.000000000000000000, 0.000000000000000000, -1.000000000000000000 ) ) ;
#101797 = CARTESIAN_POINT ( 'NONE',  ( -2.100000000000033396, 12.50000000000000000, -0.6277270498435167934 ) ) ;
#101798 = CARTESIAN_POINT ( 'NONE',  ( 1.699999999999951994, 12.50000000000000000, -2.276824562219559311E-15 ) ) ;
#101799 = DIRECTION ( 'NONE',  ( -0.000000000000000000, 1.000000000000000000, -0.000000000000000000 ) ) ;
#101800 = CIRCLE ( 'NONE', #32853, 0.1000000000000002554 ) ;
#101801 = ORIENTED_EDGE ( 'NONE', *, *, #29039, .F. ) ;
#101802 = DIRECTION ( 'NONE',  ( 0.000000000000000000, -0.9999939076577903929, 0.003490651415223739937 ) ) ;
#101803 = AXIS2_PLACEMENT_3D ( 'NONE', #24948, #53760, #102846 ) ;
#101804 = ORIENTED_EDGE ( 'NONE', *, *, #42323, .T. ) ;
#101806 = CIRCLE ( 'NONE', #49580, 0.06509327318403745899 ) ;
#101805 = AXIS2_PLACEMENT_3D ( 'NONE', #123374, #101167, #21979 ) ;
#101807 = ORIENTED_EDGE ( 'NONE', *, *, #46477, .F. ) ;
#101808 = LINE ( 'NONE', #92623, #61503 ) ;
#101809 = DIRECTION ( 'NONE',  ( -0.000000000000000000, -1.000000000000000000, -0.000000000000000000 ) ) ;
#101810 = ORIENTED_EDGE ( 'NONE', *, *, #51003, .F. ) ;
#101811 = ORIENTED_EDGE ( 'NONE', *, *, #128717, .F. ) ;
#101812 = CARTESIAN_POINT ( 'NONE',  ( -3.750000000000027534, 2.500000000000000000, -1.572243186433550211 ) ) ;
#101813 = ADVANCED_FACE ( 'NONE', ( #124570 ), #117078, .T. ) ;
#101814 = DIRECTION ( 'NONE',  ( 0.000000000000000000, 1.000000000000000000, 0.000000000000000000 ) ) ;
#101815 = PLANE ( 'NONE',  #12239 ) ;
#101816 = DIRECTION ( 'NONE',  ( 0.000000000000000000, 0.000000000000000000, 1.000000000000000000 ) ) ;
#101817 = PLANE ( 'NONE',  #123430 ) ;
#101818 = VECTOR ( 'NONE', #32586, 1000.000000000000000 ) ;
#101819 = VERTEX_POINT ( 'NONE', #23135 ) ;
#101820 = LINE ( 'NONE', #42257, #126332 ) ;
#101821 = EDGE_LOOP ( 'NONE', ( #96153, #115401, #5999, #42017 ) ) ;
#101822 = FACE_OUTER_BOUND ( 'NONE', #52111, .T. ) ;
#101823 = CARTESIAN_POINT ( 'NONE',  ( -6.850000000000013856, 2.500000000000000000, 6.248780366869521430 ) ) ;
#101824 = LINE ( 'NONE', #112927, #117988 ) ;
#101825 = DIRECTION ( 'NONE',  ( 0.000000000000000000, 0.000000000000000000, -1.000000000000000000 ) ) ;
#101826 = CARTESIAN_POINT ( 'NONE',  ( -9.350000000000008527, 12.50000000000000000, -6.841600689897072485 ) ) ;
#101827 = VERTEX_POINT ( 'NONE', #73515 ) ;
#101828 = FACE_OUTER_BOUND ( 'NONE', #52934, .T. ) ;
#101829 = VECTOR ( 'NONE', #41828, 1000.000000000000000 ) ;
#101830 = DIRECTION ( 'NONE',  ( 0.000000000000000000, 1.000000000000000000, 0.000000000000000000 ) ) ;
#101831 = EDGE_LOOP ( 'NONE', ( #42316, #76835, #50080, #17628 ) ) ;
#101832 = VERTEX_POINT ( 'NONE', #5419 ) ;
#101833 = ORIENTED_EDGE ( 'NONE', *, *, #59893, .T. ) ;
#101834 = CARTESIAN_POINT ( 'NONE',  ( 17.50000000000000000, 2.750000000000000000, 3.432456362931491700 ) ) ;
#101835 = CARTESIAN_POINT ( 'NONE',  ( -10.20000000000000284, 2.500000000000000000, -0.2464101615137782308 ) ) ;
#101836 = DIRECTION ( 'NONE',  ( 0.000000000000000000, 0.000000000000000000, 1.000000000000000000 ) ) ;
#101837 = CARTESIAN_POINT ( 'NONE',  ( -5.850000000000019185, 2.500000000000000000, 2.265063509461097357 ) ) ;
#101840 = AXIS2_PLACEMENT_3D ( 'NONE', #53562, #92181, #93489 ) ;
#101839 = CARTESIAN_POINT ( 'NONE',  ( 9.999999999999916511, 12.50000000000000000, -0.6928203230275541413 ) ) ;
#101838 = AXIS2_PLACEMENT_3D ( 'NONE', #45846, #6518, #85753 ) ;
#101841 = CARTESIAN_POINT ( 'NONE',  ( 1.249999999999953815, 2.500000000000000000, 1.472243186433545459 ) ) ;
#101842 = DIRECTION ( 'NONE',  ( 0.000000000000000000, 0.000000000000000000, 1.000000000000000000 ) ) ;
#101843 = DIRECTION ( 'NONE',  ( 0.000000000000000000, 1.000000000000000000, 0.000000000000000000 ) ) ;
#101845 = AXIS2_PLACEMENT_3D ( 'NONE', #71300, #41867, #121053 ) ;
#101844 = AXIS2_PLACEMENT_3D ( 'NONE', #22019, #121473, #10857 ) ;
#101847 = EDGE_CURVE ( 'NONE', #9468, #109985, #33490, .T. ) ;
#101846 = AXIS2_PLACEMENT_3D ( 'NONE', #81949, #20470, #818 ) ;
#101848 = ORIENTED_EDGE ( 'NONE', *, *, #59311, .T. ) ;
#101849 = DIRECTION ( 'NONE',  ( -0.000000000000000000, 1.000000000000000000, -0.000000000000000000 ) ) ;
#101850 = EDGE_CURVE ( 'NONE', #29463, #51752, #56540, .T. ) ;
#101851 = FACE_OUTER_BOUND ( 'NONE', #30928, .T. ) ;
#101852 = DIRECTION ( 'NONE',  ( 0.000000000000000000, 1.000000000000000000, 0.000000000000000000 ) ) ;
#101853 = DIRECTION ( 'NONE',  ( 0.000000000000000000, 0.000000000000000000, 1.000000000000000000 ) ) ;
#101854 = ADVANCED_FACE ( 'NONE', ( #4122 ), #29378, .T. ) ;
#101855 = EDGE_LOOP ( 'NONE', ( #124770, #84468, #22745, #9459 ) ) ;
#101856 = DIRECTION ( 'NONE',  ( -0.000000000000000000, 1.000000000000000000, -0.000000000000000000 ) ) ;
#101857 = DIRECTION ( 'NONE',  ( -0.000000000000000000, -1.000000000000000000, -0.000000000000000000 ) ) ;
#101859 = ORIENTED_EDGE ( 'NONE', *, *, #20516, .F. ) ;
#101858 = DIRECTION ( 'NONE',  ( -0.000000000000000000, 1.000000000000000000, -0.000000000000000000 ) ) ;
#101860 = EDGE_CURVE ( 'NONE', #48260, #66886, #102516, .T. ) ;
#101861 = ADVANCED_FACE ( 'NONE', ( #64978 ), #52340, .T. ) ;
#101862 = EDGE_CURVE ( 'NONE', #94029, #13624, #84637, .T. ) ;
#101863 = EDGE_CURVE ( 'NONE', #108453, #251, #104901, .T. ) ;
#101864 = EDGE_CURVE ( 'NONE', #99586, #70146, #104278, .T. ) ;
#101865 = CIRCLE ( 'NONE', #89251, 0.1000000000000000056 ) ;
#101866 = ORIENTED_EDGE ( 'NONE', *, *, #112203, .F. ) ;
#101867 = AXIS2_PLACEMENT_3D ( 'NONE', #15141, #125127, #15799 ) ;
#101868 = DIRECTION ( 'NONE',  ( 0.000000000000000000, -0.9999939076577903929, 0.003490651415223739937 ) ) ;
#101869 = ORIENTED_EDGE ( 'NONE', *, *, #33586, .F. ) ;
#101870 = ORIENTED_EDGE ( 'NONE', *, *, #14381, .F. ) ;
#101871 = CARTESIAN_POINT ( 'NONE',  ( 6.249999999999930722, 2.500000000000000000, -1.572243186433550211 ) ) ;
#101872 = EDGE_CURVE ( 'NONE', #125678, #21143, #74818, .T. ) ;
#101873 = VECTOR ( 'NONE', #79555, 1000.000000000000000 ) ;
#101874 = DIRECTION ( 'NONE',  ( 0.000000000000000000, 0.000000000000000000, 1.000000000000000000 ) ) ;
#101875 = CARTESIAN_POINT ( 'NONE',  ( -2.100000000000033840, 12.50000000000000000, 3.637306695894644726 ) ) ;
#101876 = CIRCLE ( 'NONE', #37039, 0.06509327318403741736 ) ;
#101877 = DIRECTION ( 'NONE',  ( -0.000000000000000000, -1.000000000000000000, -0.000000000000000000 ) ) ;
#101878 = EDGE_LOOP ( 'NONE', ( #13855, #122561 ) ) ;
#101879 = AXIS2_PLACEMENT_3D ( 'NONE', #64149, #73980, #66081 ) ;
#101880 = AXIS2_PLACEMENT_3D ( 'NONE', #128942, #71275, #119097 ) ;
#101881 = FACE_OUTER_BOUND ( 'NONE', #89248, .T. ) ;
#101882 = ORIENTED_EDGE ( 'NONE', *, *, #60312, .F. ) ;
#101883 = CARTESIAN_POINT ( 'NONE',  ( 17.50000000000000000, 2.500000000000000000, 2.922290670087886344 ) ) ;
#101884 = AXIS2_PLACEMENT_3D ( 'NONE', #121585, #52222, #113056 ) ;
#101885 = LINE ( 'NONE', #92051, #73952 ) ;
#101886 = VERTEX_POINT ( 'NONE', #34265 ) ;
#101888 = AXIS2_PLACEMENT_3D ( 'NONE', #63294, #111757, #103228 ) ;
#101887 = CONICAL_SURFACE ( 'NONE', #118605, 0.09999999999999982514, 0.003490658503988666988 ) ;
#101889 = ORIENTED_EDGE ( 'NONE', *, *, #93318, .T. ) ;
#101890 = ORIENTED_EDGE ( 'NONE', *, *, #35881, .F. ) ;
#101891 = VERTEX_POINT ( 'NONE', #125207 ) ;
#101892 = DIRECTION ( 'NONE',  ( 0.000000000000000000, 0.000000000000000000, 1.000000000000000000 ) ) ;
#101893 = CARTESIAN_POINT ( 'NONE',  ( 13.91976764310571824, 2.500000000000000444, 6.779443705067744297 ) ) ;
#101894 = PLANE ( 'NONE',  #62954 ) ;
#101895 = FACE_BOUND ( 'NONE', #41609, .T. ) ;
#101896 = ORIENTED_EDGE ( 'NONE', *, *, #107699, .F. ) ;
#101897 = PLANE ( 'NONE',  #97494 ) ;
#101898 = CARTESIAN_POINT ( 'NONE',  ( 185.2812500006828031, 0.000000000000000000, 7.700000000000000178 ) ) ;
#101899 = DIRECTION ( 'NONE',  ( 0.000000000000000000, 0.000000000000000000, -1.000000000000000000 ) ) ;
#101900 = CARTESIAN_POINT ( 'NONE',  ( -11.64999999999999680, 2.500000000000000000, 6.595190528383296780 ) ) ;
#101901 = DIRECTION ( 'NONE',  ( 0.000000000000000000, -0.000000000000000000, 1.000000000000000000 ) ) ;
#101902 = CARTESIAN_POINT ( 'NONE',  ( 107.5000000000000142, -1.500000000000000222, -1.322875655532295136 ) ) ;
#101903 = EDGE_CURVE ( 'NONE', #62359, #44343, #112168, .T. ) ;
#101904 = UNCERTAINTY_MEASURE_WITH_UNIT (LENGTH_MEASURE( 1.000000000000000082E-05 ), #110801, 'distance_accuracy_value', 'NONE');
#101905 = CARTESIAN_POINT ( 'NONE',  ( -6.249999999999984901, 2.500000000000000000, -2.265063509461101798 ) ) ;
#101906 = EDGE_CURVE ( 'NONE', #2854, #87563, #12654, .T. ) ;
#101907 = DIRECTION ( 'NONE',  ( 0.000000000000000000, 0.000000000000000000, -1.000000000000000000 ) ) ;
#101908 = EDGE_CURVE ( 'NONE', #128585, #72457, #94113, .T. ) ;
#101909 = EDGE_LOOP ( 'NONE', ( #116736, #28863 ) ) ;
#101910 = ORIENTED_EDGE ( 'NONE', *, *, #2530, .T. ) ;
#101911 = ORIENTED_EDGE ( 'NONE', *, *, #51906, .F. ) ;
#101912 = ORIENTED_EDGE ( 'NONE', *, *, #95178, .F. ) ;
#101913 = VERTEX_POINT ( 'NONE', #2850 ) ;
#101914 = DIRECTION ( 'NONE',  ( 0.000000000000000000, 1.000000000000000000, 0.000000000000000000 ) ) ;
#101915 = DIRECTION ( 'NONE',  ( 0.000000000000000000, 1.000000000000000000, 0.000000000000000000 ) ) ;
#101917 = EDGE_CURVE ( 'NONE', #3186, #78294, #110827, .T. ) ;
#101916 = ORIENTED_EDGE ( 'NONE', *, *, #50966, .F. ) ;
#101918 = FACE_BOUND ( 'NONE', #23074, .T. ) ;
#101919 = DIRECTION ( 'NONE',  ( -0.000000000000000000, -1.000000000000000000, -0.000000000000000000 ) ) ;
#101920 = EDGE_CURVE ( 'NONE', #13968, #125307, #114733, .T. ) ;
#101922 = ADVANCED_FACE ( 'NONE', ( #13950 ), #54515, .T. ) ;
#101921 = CIRCLE ( 'NONE', #5745, 0.06509327318403745899 ) ;
#101923 = CIRCLE ( 'NONE', #43354, 0.06509327318403745899 ) ;
#101924 = ADVANCED_FACE ( 'NONE', ( #123907 ), #113068, .T. ) ;
#101925 = ORIENTED_EDGE ( 'NONE', *, *, #41174, .T. ) ;
#101926 = CARTESIAN_POINT ( 'NONE',  ( 3.749999999999942268, 12.50000000000000000, 1.472243186433545459 ) ) ;
#101927 = CARTESIAN_POINT ( 'NONE',  ( 6.249999999999932498, 2.500000000000000000, 5.802370205355744659 ) ) ;
#101928 = CARTESIAN_POINT ( 'NONE',  ( -7.300000000000013145, 2.500000000000000000, 3.983716857408420076 ) ) ;
#101929 = ORIENTED_EDGE ( 'NONE', *, *, #86853, .T. ) ;
#101930 = CARTESIAN_POINT ( 'NONE',  ( -2.499999999999996003, 12.50000000000000000, -4.265033745738164406 ) ) ;
#101931 = EDGE_CURVE ( 'NONE', #1738, #43544, #44723, .T. ) ;
#101932 = CIRCLE ( 'NONE', #43364, 0.06509327318403745899 ) ;
#101933 = EDGE_LOOP ( 'NONE', ( #89510, #67569 ) ) ;
#101934 = VERTEX_POINT ( 'NONE', #36837 ) ;
#101935 = ORIENTED_EDGE ( 'NONE', *, *, #107985, .F. ) ;
#101936 = LINE ( 'NONE', #10328, #8935 ) ;
#101937 = DIRECTION ( 'NONE',  ( 0.000000000000000000, -0.9999939076577903929, 0.003490651415223739937 ) ) ;
#101938 = ORIENTED_EDGE ( 'NONE', *, *, #11314, .F. ) ;
#101939 = LINE ( 'NONE', #72487, #72652 ) ;
#101940 = CIRCLE ( 'NONE', #87340, 0.09999999999999982514 ) ;
#101941 = FACE_OUTER_BOUND ( 'NONE', #92764, .T. ) ;
#101942 = DIRECTION ( 'NONE',  ( 0.000000000000000000, 1.000000000000000000, 0.000000000000000000 ) ) ;
#101943 = DIRECTION ( 'NONE',  ( 0.000000000000000000, 0.000000000000000000, 1.000000000000000000 ) ) ;
#101944 = ORIENTED_EDGE ( 'NONE', *, *, #43053, .F. ) ;
#101945 = DIRECTION ( 'NONE',  ( 0.000000000000000000, -0.000000000000000000, 1.000000000000000000 ) ) ;
#101946 = EDGE_CURVE ( 'NONE', #125134, #125433, #50379, .T. ) ;
#101947 = EDGE_LOOP ( 'NONE', ( #10829, #58519, #112610, #19799 ) ) ;
#101948 = DIRECTION ( 'NONE',  ( 0.000000000000000000, 0.000000000000000000, 1.000000000000000000 ) ) ;
#101949 = VERTEX_POINT ( 'NONE', #117280 ) ;
#101950 = FACE_OUTER_BOUND ( 'NONE', #54909, .T. ) ;
#101951 = ORIENTED_EDGE ( 'NONE', *, *, #123783, .T. ) ;
#101952 = LINE ( 'NONE', #120939, #72221 ) ;
#101953 = AXIS2_PLACEMENT_3D ( 'NONE', #106752, #107408, #8540 ) ;
#101954 = DIRECTION ( 'NONE',  ( 0.000000000000000000, 1.000000000000000000, 0.000000000000000000 ) ) ;
#101955 = DIRECTION ( 'NONE',  ( 0.000000000000000000, 1.000000000000000000, 0.000000000000000000 ) ) ;
#101956 = LINE ( 'NONE', #72506, #65502 ) ;
#101958 = CIRCLE ( 'NONE', #106065, 0.1000000000000000472 ) ;
#101957 = CARTESIAN_POINT ( 'NONE',  ( 3.549999999999944755, 12.50000000000000000, -6.841600689897077814 ) ) ;
#101959 = ORIENTED_EDGE ( 'NONE', *, *, #20211, .T. ) ;
#101960 = VECTOR ( 'NONE', #101468, 1000.000000000000000 ) ;
#101961 = ORIENTED_EDGE ( 'NONE', *, *, #75564, .T. ) ;
#101962 = PLANE ( 'NONE',  #22491 ) ;
#101963 = AXIS2_PLACEMENT_3D ( 'NONE', #98311, #6686, #46655 ) ;
#101964 = EDGE_CURVE ( 'NONE', #16412, #14739, #48585, .T. ) ;
#101965 = CARTESIAN_POINT ( 'NONE',  ( 12.69999999999990159, 2.500000000000000000, -3.883716857408426648 ) ) ;
#101966 = DIRECTION ( 'NONE',  ( -0.000000000000000000, -1.000000000000000000, -0.000000000000000000 ) ) ;
#101968 = EDGE_LOOP ( 'NONE', ( #97239, #9556, #53018, #114594 ) ) ;
#101967 = ORIENTED_EDGE ( 'NONE', *, *, #14488, .F. ) ;
#101969 = EDGE_LOOP ( 'NONE', ( #75209, #69159 ) ) ;
#101970 = DIRECTION ( 'NONE',  ( 0.000000000000000000, 0.000000000000000000, 1.000000000000000000 ) ) ;
#101971 = AXIS2_PLACEMENT_3D ( 'NONE', #98374, #50572, #61040 ) ;
#101972 = AXIS2_PLACEMENT_3D ( 'NONE', #56526, #74895, #114174 ) ;
#101973 = VERTEX_POINT ( 'NONE', #107500 ) ;
#101974 = DIRECTION ( 'NONE',  ( 0.000000000000000000, 0.000000000000000000, 1.000000000000000000 ) ) ;
#101975 = DIRECTION ( 'NONE',  ( 0.000000000000000000, 0.000000000000000000, 1.000000000000000000 ) ) ;
#101976 = AXIS2_PLACEMENT_3D ( 'NONE', #114421, #92873, #103330 ) ;
#101977 = DIRECTION ( 'NONE',  ( -4.274815082592931898E-19, -0.9999939076577903929, -0.003490651415223739937 ) ) ;
#101978 = ORIENTED_EDGE ( 'NONE', *, *, #13180, .T. ) ;
#101979 = CARTESIAN_POINT ( 'NONE',  ( -9.800000000000006040, 12.50000000000000000, 0.3464101615137735735 ) ) ;
#101980 = DIRECTION ( 'NONE',  ( 0.000000000000000000, 1.000000000000000000, 0.000000000000000000 ) ) ;
#101981 = DIRECTION ( 'NONE',  ( -4.274815082592931898E-19, -0.9999939076577903929, -0.003490651415223739937 ) ) ;
#101982 = CARTESIAN_POINT ( 'NONE',  ( -10.00000000000000355, 12.50000000000000000, 3.637306695894644726 ) ) ;
#101983 = AXIS2_PLACEMENT_3D ( 'NONE', #1176, #70559, #110486 ) ;
#101984 = EDGE_CURVE ( 'NONE', #27644, #109941, #7996, .T. ) ;
#101985 = CARTESIAN_POINT ( 'NONE',  ( 7.899999999999923084, 12.50000000000000000, -0.6928203230275542523 ) ) ;
#101986 = ORIENTED_EDGE ( 'NONE', *, *, #102325, .T. ) ;
#101987 = FACE_OUTER_BOUND ( 'NONE', #25488, .T. ) ;
#101989 = AXIS2_PLACEMENT_3D ( 'NONE', #59955, #18051, #29823 ) ;
#101988 = AXIS2_PLACEMENT_3D ( 'NONE', #43396, #11341, #83316 ) ;
#101990 = CARTESIAN_POINT ( 'NONE',  ( 59.88499455099038471, -2.860410828927322680, 5.641292085222127106 ) ) ;
#101991 = ORIENTED_EDGE ( 'NONE', *, *, #17150, .T. ) ;
#101992 = ORIENTED_EDGE ( 'NONE', *, *, #10873, .T. ) ;
#101993 = CARTESIAN_POINT ( 'NONE',  ( 184.6093750003413732, 9.264065473108010111E-16, -7.564683531250000925 ) ) ;
#101994 = DIRECTION ( 'NONE',  ( -4.274815082592931898E-19, -0.9999939076577903929, -0.003490651415223739937 ) ) ;
#101995 = LINE ( 'NONE', #70597, #24890 ) ;
#101996 = DIRECTION ( 'NONE',  ( 0.000000000000000000, 0.000000000000000000, 1.000000000000000000 ) ) ;
#101997 = DIRECTION ( 'NONE',  ( 0.000000000000000000, 0.000000000000000000, -1.000000000000000000 ) ) ;
#101998 = DIRECTION ( 'NONE',  ( 0.000000000000000000, 0.000000000000000000, -1.000000000000000000 ) ) ;
#101999 = FACE_OUTER_BOUND ( 'NONE', #51507, .T. ) ;
#102000 = CARTESIAN_POINT ( 'NONE',  ( -2.300000000000033129, 2.500000000000000000, 3.983716857408420076 ) ) ;
#102001 = LINE ( 'NONE', #120993, #58381 ) ;
#102002 = EDGE_LOOP ( 'NONE', ( #104001, #26411 ) ) ;
#102003 = ORIENTED_EDGE ( 'NONE', *, *, #90837, .F. ) ;
#102004 = ADVANCED_FACE ( 'NONE', ( #106835 ), #108136, .T. ) ;
#102005 = ORIENTED_EDGE ( 'NONE', *, *, #80856, .F. ) ;
#102006 = AXIS2_PLACEMENT_3D ( 'NONE', #79712, #20153, #60094 ) ;
#102007 = ORIENTED_EDGE ( 'NONE', *, *, #20560, .F. ) ;
#102008 = LINE ( 'NONE', #12328, #12737 ) ;
#102009 = DIRECTION ( 'NONE',  ( -0.000000000000000000, 1.000000000000000000, -0.000000000000000000 ) ) ;
#102010 = EDGE_LOOP ( 'NONE', ( #90985, #121314 ) ) ;
#102011 = CIRCLE ( 'NONE', #129230, 0.1000000000000002554 ) ;
#102012 = CARTESIAN_POINT ( 'NONE',  ( 11.24999999999991118, 12.50000000000000000, 5.737276932171707422 ) ) ;
#102013 = CIRCLE ( 'NONE', #58105, 0.06509327318403745899 ) ;
#102014 = DIRECTION ( 'NONE',  ( -0.000000000000000000, -1.000000000000000000, -0.000000000000000000 ) ) ;
#102016 = ORIENTED_EDGE ( 'NONE', *, *, #105638, .T. ) ;
#102015 = DIRECTION ( 'NONE',  ( 0.000000000000000000, -0.9999939076577903929, 0.003490651415223739937 ) ) ;
#102017 = ADVANCED_FACE ( 'NONE', ( #116666 ), #97033, .T. ) ;
#102018 = EDGE_CURVE ( 'NONE', #44623, #37437, #66998, .T. ) ;
#102019 = EDGE_CURVE ( 'NONE', #83059, #51134, #27291, .T. ) ;
#102020 = CARTESIAN_POINT ( 'NONE',  ( 9.149999999999918643, 12.50000000000000000, 2.230156782645134950 ) ) ;
#102021 = ADVANCED_FACE ( 'NONE', ( #77395 ), #46172, .T. ) ;
#102022 = AXIS2_PLACEMENT_3D ( 'NONE', #49360, #29698, #81839 ) ;
#102023 = DIRECTION ( 'NONE',  ( -0.000000000000000000, 1.000000000000000000, -0.000000000000000000 ) ) ;
#102024 = EDGE_LOOP ( 'NONE', ( #12582, #123764, #111707, #86596 ) ) ;
#102025 = AXIS2_PLACEMENT_3D ( 'NONE', #91580, #81747, #41215 ) ;
#102026 = ORIENTED_EDGE ( 'NONE', *, *, #119197, .F. ) ;
#102027 = ORIENTED_EDGE ( 'NONE', *, *, #50038, .F. ) ;
#102028 = VERTEX_POINT ( 'NONE', #26371 ) ;
#102029 = FACE_OUTER_BOUND ( 'NONE', #74590, .T. ) ;
#102030 = ADVANCED_FACE ( 'NONE', ( #105568 ), #12704, .T. ) ;
#102031 = DIRECTION ( 'NONE',  ( -0.000000000000000000, -1.000000000000000000, -0.000000000000000000 ) ) ;
#102032 = CARTESIAN_POINT ( 'NONE',  ( -11.24999999999996447, 12.50000000000000000, -6.495190528383298911 ) ) ;
#102033 = EDGE_CURVE ( 'NONE', #108138, #106136, #50297, .T. ) ;
#102034 = CARTESIAN_POINT ( 'NONE',  ( -6.850000000000017408, 12.50000000000000000, -1.753560074763288457 ) ) ;
#102035 = CIRCLE ( 'NONE', #64367, 0.06509327318403745899 ) ;
#102037 = ORIENTED_EDGE ( 'NONE', *, *, #112640, .T. ) ;
#102036 = ADVANCED_FACE ( 'NONE', ( #47943 ), #83740, .T. ) ;
#102038 = DIRECTION ( 'NONE',  ( 0.000000000000000000, 1.000000000000000000, 0.000000000000000000 ) ) ;
#102039 = ORIENTED_EDGE ( 'NONE', *, *, #92576, .T. ) ;
#102040 = CARTESIAN_POINT ( 'NONE',  ( 184.5000000000000000, 0.000000000000000000, 7.700000000000000178 ) ) ;
#102041 = DIRECTION ( 'NONE',  ( 0.000000000000000000, 0.000000000000000000, -1.000000000000000000 ) ) ;
#102042 = DIRECTION ( 'NONE',  ( 0.000000000000000000, 0.000000000000000000, 1.000000000000000000 ) ) ;
#102043 = DIRECTION ( 'NONE',  ( -0.000000000000000000, -1.000000000000000000, -0.000000000000000000 ) ) ;
#102044 = ORIENTED_EDGE ( 'NONE', *, *, #13973, .F. ) ;
#102045 = AXIS2_PLACEMENT_3D ( 'NONE', #40737, #10581, #51829 ) ;
#102046 = CONICAL_SURFACE ( 'NONE', #53922, 0.09999999999999982514, 0.003490658503988666988 ) ;
#102047 = VERTEX_POINT ( 'NONE', #98307 ) ;
#102048 = ORIENTED_EDGE ( 'NONE', *, *, #106127, .T. ) ;
#102049 = CARTESIAN_POINT ( 'NONE',  ( -9.150000000000009237, 2.500000000000000000, -1.572243186433550211 ) ) ;
#102050 = CARTESIAN_POINT ( 'NONE',  ( -6.450000000000016165, 2.500000000000000000, 6.941600689897073018 ) ) ;
#102051 = DIRECTION ( 'NONE',  ( 0.000000000000000000, 0.000000000000000000, -1.000000000000000000 ) ) ;
#102052 = FACE_BOUND ( 'NONE', #4638, .T. ) ;
#102053 = VECTOR ( 'NONE', #7443, 1000.000000000000000 ) ;
#102054 = CARTESIAN_POINT ( 'NONE',  ( -2.500000000000032863, 12.50000000000000000, 4.957854068765711553 ) ) ;
#102055 = CARTESIAN_POINT ( 'NONE',  ( -6.249999999999981348, 2.500000000000000000, 2.165063509461097713 ) ) ;
#102056 = CIRCLE ( 'NONE', #14202, 0.09999999999999982514 ) ;
#102057 = CARTESIAN_POINT ( 'NONE',  ( -4.999999999999986677, 12.50000000000000000, -2.276824562219559311E-15 ) ) ;
#102058 = AXIS2_PLACEMENT_3D ( 'NONE', #11864, #40719, #89793 ) ;
#102059 = MANIFOLD_SOLID_BREP ( 'Extrude-Thin1', #112600 ) ;
#102060 = DIRECTION ( 'NONE',  ( 0.000000000000000000, 1.000000000000000000, 0.000000000000000000 ) ) ;
#102062 = CARTESIAN_POINT ( 'NONE',  ( 184.0833333333333144, -6.668395609140180369, 3.849999999999994760 ) ) ;
#102061 = CIRCLE ( 'NONE', #45638, 0.06509327318403745899 ) ;
#102063 = LINE ( 'NONE', #2543, #7212 ) ;
#102064 = EDGE_LOOP ( 'NONE', ( #35949, #65366, #54883, #61830 ) ) ;
#102065 = DIRECTION ( 'NONE',  ( 0.000000000000000000, 0.000000000000000000, -1.000000000000000000 ) ) ;
#102066 = DIRECTION ( 'NONE',  ( 0.000000000000000000, 0.000000000000000000, 1.000000000000000000 ) ) ;
#102067 = VERTEX_POINT ( 'NONE', #28952 ) ;
#102068 = VERTEX_POINT ( 'NONE', #70792 ) ;
#102069 = CARTESIAN_POINT ( 'NONE',  ( -7.050000000000016698, 2.500000000000000000, -6.495190528383302464 ) ) ;
#102070 = CONICAL_SURFACE ( 'NONE', #26847, 0.09999999999999982514, 0.003490658503988666988 ) ;
#102071 = CARTESIAN_POINT ( 'NONE',  ( -14.59999999999998366, 2.500000000000000000, -0.1000000000000001166 ) ) ;
#102072 = FACE_BOUND ( 'NONE', #25950, .T. ) ;
#102073 = DIRECTION ( 'NONE',  ( 0.000000000000000000, -0.000000000000000000, 1.000000000000000000 ) ) ;
#102074 = EDGE_CURVE ( 'NONE', #67061, #73868, #29460, .T. ) ;
#102076 = CIRCLE ( 'NONE', #62379, 0.1000000000000002554 ) ;
#102075 = AXIS2_PLACEMENT_3D ( 'NONE', #103279, #103917, #32633 ) ;
#102077 = ADVANCED_FACE ( 'NONE', ( #99622 ), #51170, .T. ) ;
#102078 = ORIENTED_EDGE ( 'NONE', *, *, #42693, .F. ) ;
#102079 = FACE_OUTER_BOUND ( 'NONE', #72626, .T. ) ;
#102080 = DIRECTION ( 'NONE',  ( 0.000000000000000000, 1.000000000000000000, 0.000000000000000000 ) ) ;
#102081 = EDGE_LOOP ( 'NONE', ( #119660, #56476 ) ) ;
#102082 = CARTESIAN_POINT ( 'NONE',  ( 0.3999999999999568345, 12.50000000000000000, -3.637306695894650055 ) ) ;
#102083 = CARTESIAN_POINT ( 'NONE',  ( -11.64999999999999680, 12.50000000000000000, 1.472243186433545459 ) ) ;
#102084 = EDGE_CURVE ( 'NONE', #112645, #21459, #117159, .T. ) ;
#102085 = ORIENTED_EDGE ( 'NONE', *, *, #55766, .T. ) ;
#102086 = AXIS2_PLACEMENT_3D ( 'NONE', #124936, #113173, #23504 ) ;
#102087 = DIRECTION ( 'NONE',  ( -0.000000000000000000, 1.000000000000000000, -0.000000000000000000 ) ) ;
#102088 = DIRECTION ( 'NONE',  ( 0.000000000000000000, 1.000000000000000000, 0.000000000000000000 ) ) ;
#102089 = VERTEX_POINT ( 'NONE', #128452 ) ;
#102090 = CARTESIAN_POINT ( 'NONE',  ( 10.19999999999991225, 12.50000000000000000, -4.611443907251940644 ) ) ;
#102091 = CIRCLE ( 'NONE', #66858, 0.1000000000000002554 ) ;
#102092 = CARTESIAN_POINT ( 'NONE',  ( 11.24999999999990763, 2.500000000000000000, -7.188010851410854052 ) ) ;
#102093 = CIRCLE ( 'NONE', #93682, 0.09999999999999982514 ) ;
#102094 = CONICAL_SURFACE ( 'NONE', #77242, 0.1000000000000002554, 0.003490658503988666988 ) ;
#102095 = DIRECTION ( 'NONE',  ( -4.274815082592931898E-19, -0.9999939076577903929, -0.003490651415223739937 ) ) ;
#102096 = EDGE_LOOP ( 'NONE', ( #7985, #57549, #78252, #6076 ) ) ;
#102097 = ORIENTED_EDGE ( 'NONE', *, *, #95925, .F. ) ;
#102098 = CARTESIAN_POINT ( 'NONE',  ( -3.300000000000028244, 12.50000000000000000, 4.330127018922196314 ) ) ;
#102100 = ORIENTED_EDGE ( 'NONE', *, *, #55526, .T. ) ;
#102099 = CIRCLE ( 'NONE', #8094, 0.1000000000000002554 ) ;
#102101 = CARTESIAN_POINT ( 'NONE',  ( -14.79999999999998472, 12.50000000000000000, 0.3464101615137758494 ) ) ;
#102102 = CARTESIAN_POINT ( 'NONE',  ( -4.350000000000023626, 2.500000000000000000, 6.148780366869520897 ) ) ;
#102103 = VECTOR ( 'NONE', #65418, 1000.000000000000000 ) ;
#102104 = CIRCLE ( 'NONE', #110408, 0.1000000000000002554 ) ;
#102105 = CARTESIAN_POINT ( 'NONE',  ( -3.300000000000027800, 2.500000000000000000, -2.276824562219559311E-15 ) ) ;
#102106 = ORIENTED_EDGE ( 'NONE', *, *, #17478, .F. ) ;
#102107 = FACE_OUTER_BOUND ( 'NONE', #67329, .T. ) ;
#102108 = LINE ( 'NONE', #99540, #7989 ) ;
#102109 = CARTESIAN_POINT ( 'NONE',  ( 4.399999999999939071, 2.500000000000000000, 0.3464101615137736845 ) ) ;
#102110 = CARTESIAN_POINT ( 'NONE',  ( 7.949999999999925571, 12.50000000000000000, 2.099970236277060032 ) ) ;
#102111 = DIRECTION ( 'NONE',  ( 0.000000000000000000, 1.000000000000000000, 0.000000000000000000 ) ) ;
#102112 = CARTESIAN_POINT ( 'NONE',  ( -9.400000000000007461, 2.500000000000000000, -0.2464101615137783419 ) ) ;
#102113 = AXIS2_PLACEMENT_3D ( 'NONE', #99320, #9642, #88172 ) ;
#102114 = EDGE_LOOP ( 'NONE', ( #71467, #101446, #82316, #111489 ) ) ;
#102116 = VERTEX_POINT ( 'NONE', #110079 ) ;
#102115 = CIRCLE ( 'NONE', #89597, 0.1000000000000000056 ) ;
#102117 = CARTESIAN_POINT ( 'NONE',  ( 9.999999999999916511, 12.50000000000000000, -0.6277270498435166823 ) ) ;
#102118 = ORIENTED_EDGE ( 'NONE', *, *, #126855, .F. ) ;
#102119 = ADVANCED_FACE ( 'NONE', ( #10566 ), #127650, .T. ) ;
#102120 = CARTESIAN_POINT ( 'NONE',  ( 107.3227259355851402, 5.885842102929867536, -4.965337704341070690 ) ) ;
#102122 = ORIENTED_EDGE ( 'NONE', *, *, #106463, .F. ) ;
#102121 = VERTEX_POINT ( 'NONE', #110707 ) ;
#102123 = VERTEX_POINT ( 'NONE', #31517 ) ;
#102124 = CARTESIAN_POINT ( 'NONE',  ( 9.199999999999915801, 2.500000000000000000, -4.230127018922201998 ) ) ;
#102125 = CARTESIAN_POINT ( 'NONE',  ( 11.44999999999991047, 12.50000000000000000, 6.148780366869520009 ) ) ;
#102126 = DIRECTION ( 'NONE',  ( 0.000000000000000000, 0.000000000000000000, 1.000000000000000000 ) ) ;
#102127 =( NAMED_UNIT ( * ) SI_UNIT ( $, .STERADIAN. ) SOLID_ANGLE_UNIT ( ) );
#102128 = PLANE ( 'NONE',  #43190 ) ;
#102129 = CARTESIAN_POINT ( 'NONE',  ( -11.84999999999999787, 2.500000000000000000, -2.511473670974873951 ) ) ;
#102130 = CIRCLE ( 'NONE', #118844, 0.06509327318403745899 ) ;
#102131 = CARTESIAN_POINT ( 'NONE',  ( -2.100000000000033396, 2.500000000000000000, -5.022947341949754119 ) ) ;
#102132 = ADVANCED_FACE ( 'NONE', ( #758 ), #62904, .T. ) ;
#102133 = FACE_OUTER_BOUND ( 'NONE', #57863, .T. ) ;
#102134 = CIRCLE ( 'NONE', #79064, 0.09999999999999999167 ) ;
#102135 = DIRECTION ( 'NONE',  ( 0.000000000000000000, 0.000000000000000000, 1.000000000000000000 ) ) ;
#102136 = EDGE_CURVE ( 'NONE', #18789, #119556, #119330, .T. ) ;
#102137 = PLANE ( 'NONE',  #66585 ) ;
#102138 = AXIS2_PLACEMENT_3D ( 'NONE', #69294, #7805, #17622 ) ;
#102139 = ORIENTED_EDGE ( 'NONE', *, *, #25916, .F. ) ;
#102140 = STYLED_ITEM ( 'NONE', ( #47237 ), #25840 ) ;
#102141 = PLANE ( 'NONE',  #23511 ) ;
#102142 = ORIENTED_EDGE ( 'NONE', *, *, #7231, .T. ) ;
#102143 = EDGE_CURVE ( 'NONE', #35473, #8018, #6425, .T. ) ;
#102144 = ORIENTED_EDGE ( 'NONE', *, *, #25911, .F. ) ;
#102145 = CARTESIAN_POINT ( 'NONE',  ( 6.449999999999931788, 2.500000000000000000, -2.611473670974877592 ) ) ;
#102146 = DIRECTION ( 'NONE',  ( 0.000000000000000000, 0.000000000000000000, 1.000000000000000000 ) ) ;
#102147 = AXIS2_PLACEMENT_3D ( 'NONE', #13412, #63165, #15336 ) ;
#102148 = DIRECTION ( 'NONE',  ( -0.000000000000000000, -1.000000000000000000, -0.000000000000000000 ) ) ;
#102149 = CARTESIAN_POINT ( 'NONE',  ( 4.399999999999940847, 12.50000000000000000, -3.983716857408426293 ) ) ;
#102150 = LINE ( 'NONE', #9899, #8774 ) ;
#102151 = DIRECTION ( 'NONE',  ( -0.000000000000000000, -1.000000000000000000, -0.000000000000000000 ) ) ;
#102152 = DIRECTION ( 'NONE',  ( -4.274815082592931898E-19, -0.9999939076577903929, -0.003490651415223739937 ) ) ;
#102153 = ORIENTED_EDGE ( 'NONE', *, *, #41618, .F. ) ;
#102154 = CIRCLE ( 'NONE', #20584, 0.09999999999999982514 ) ;
#102155 = EDGE_LOOP ( 'NONE', ( #118710, #127254, #10465, #32961 ) ) ;
#102156 = VERTEX_POINT ( 'NONE', #21044 ) ;
#102157 = EDGE_CURVE ( 'NONE', #69509, #81044, #90073, .T. ) ;
#102158 = CIRCLE ( 'NONE', #96167, 0.06509327318403745899 ) ;
#102159 = ORIENTED_EDGE ( 'NONE', *, *, #1377, .T. ) ;
#102160 = CONICAL_SURFACE ( 'NONE', #100108, 0.1000000000000002554, 0.003490658503988666988 ) ;
#102161 = VERTEX_POINT ( 'NONE', #9941 ) ;
#102162 = DIRECTION ( 'NONE',  ( 0.000000000000000000, 1.000000000000000000, 0.000000000000000000 ) ) ;
#102163 = LINE ( 'NONE', #12483, #83349 ) ;
#102164 = EDGE_CURVE ( 'NONE', #249, #25677, #37772, .T. ) ;
#102166 = CIRCLE ( 'NONE', #54046, 0.1000000000000002554 ) ;
#102165 = CONICAL_SURFACE ( 'NONE', #120934, 0.1000000000000002554, 0.003490658503988666988 ) ;
#102167 = CARTESIAN_POINT ( 'NONE',  ( -12.29999999999999361, 12.50000000000000000, 3.983716857408420076 ) ) ;
#102168 = DIRECTION ( 'NONE',  ( 0.000000000000000000, -0.9999939076577903929, 0.003490651415223739937 ) ) ;
#102169 = CARTESIAN_POINT ( 'NONE',  ( -8.950000000000008171, 2.500000000000000000, -2.611473670974877592 ) ) ;
#102170 = VERTEX_POINT ( 'NONE', #11861 ) ;
#102171 = CARTESIAN_POINT ( 'NONE',  ( 1.449999999999951328, 12.50000000000000000, 2.511473670974873507 ) ) ;
#102172 = CARTESIAN_POINT ( 'NONE',  ( 1.449999999999950440, 2.500000000000000000, 6.148780366869520009 ) ) ;
#102173 = EDGE_CURVE ( 'NONE', #28294, #1556, #25227, .T. ) ;
#102174 = EDGE_CURVE ( 'NONE', #126006, #43603, #9297, .T. ) ;
#102175 = CARTESIAN_POINT ( 'NONE',  ( -1.250000000000037970, 2.500000000000000000, 2.957883832488649389 ) ) ;
#102176 = EDGE_CURVE ( 'NONE', #95189, #67065, #49886, .T. ) ;
#102177 = DIRECTION ( 'NONE',  ( 0.000000000000000000, 1.000000000000000000, 0.000000000000000000 ) ) ;
#102178 = EDGE_CURVE ( 'NONE', #27833, #105130, #123528, .T. ) ;
#102179 = DIRECTION ( 'NONE',  ( -0.000000000000000000, -1.000000000000000000, -0.000000000000000000 ) ) ;
#102180 = ORIENTED_EDGE ( 'NONE', *, *, #124846, .T. ) ;
#102181 = EDGE_LOOP ( 'NONE', ( #103919, #71795, #113500, #117915 ) ) ;
#102183 = ORIENTED_EDGE ( 'NONE', *, *, #98326, .F. ) ;
#102182 = EDGE_CURVE ( 'NONE', #91287, #115300, #121384, .T. ) ;
#102184 = LINE ( 'NONE', #90405, #6993 ) ;
#102185 = ADVANCED_FACE ( 'NONE', ( #21705 ), #129102, .T. ) ;
#102186 = VERTEX_POINT ( 'NONE', #40052 ) ;
#102187 = DIRECTION ( 'NONE',  ( 0.000000000000000000, 0.000000000000000000, 1.000000000000000000 ) ) ;
#102188 = DIRECTION ( 'NONE',  ( 0.000000000000000000, 0.000000000000000000, 1.000000000000000000 ) ) ;
#102189 = EDGE_CURVE ( 'NONE', #124289, #44948, #101547, .T. ) ;
#102190 = CIRCLE ( 'NONE', #16565, 0.1000000000000002554 ) ;
#102191 = EDGE_CURVE ( 'NONE', #115959, #41978, #58701, .T. ) ;
#102192 = AXIS2_PLACEMENT_3D ( 'NONE', #48070, #97160, #7479 ) ;
#102193 = AXIS2_PLACEMENT_3D ( 'NONE', #79746, #119663, #69931 ) ;
#102194 = ORIENTED_EDGE ( 'NONE', *, *, #82364, .F. ) ;
#102195 = DIRECTION ( 'NONE',  ( 0.000000000000000000, -0.9999939076577903929, 0.003490651415223739937 ) ) ;
#102196 = DIRECTION ( 'NONE',  ( -0.000000000000000000, -1.000000000000000000, -0.000000000000000000 ) ) ;
#102197 = EDGE_CURVE ( 'NONE', #83000, #42689, #25324, .T. ) ;
#102198 = DIRECTION ( 'NONE',  ( -0.000000000000000000, 1.000000000000000000, -0.000000000000000000 ) ) ;
#102199 = DIRECTION ( 'NONE',  ( 0.000000000000000000, -0.9999939076577903929, 0.003490651415223739937 ) ) ;
#102200 = EDGE_CURVE ( 'NONE', #13735, #109941, #54564, .T. ) ;
#102201 = AXIS2_PLACEMENT_3D ( 'NONE', #127920, #55952, #6195 ) ;
#102202 = AXIS2_PLACEMENT_3D ( 'NONE', #91512, #100668, #60145 ) ;
#102203 = CONICAL_SURFACE ( 'NONE', #114705, 0.09999999999999982514, 0.003490658503988666988 ) ;
#102204 = DIRECTION ( 'NONE',  ( -0.000000000000000000, 1.000000000000000000, -0.000000000000000000 ) ) ;
#102205 = VERTEX_POINT ( 'NONE', #113285 ) ;
#102206 = EDGE_LOOP ( 'NONE', ( #26840, #82051 ) ) ;
#102207 = LINE ( 'NONE', #23000, #39732 ) ;
#102208 = CARTESIAN_POINT ( 'NONE',  ( -9.350000000000006750, 2.500000000000000000, 2.411473670974873862 ) ) ;
#102209 = LINE ( 'NONE', #12517, #30434 ) ;
#102210 = DIRECTION ( 'NONE',  ( 0.000000000000000000, 0.000000000000000000, -1.000000000000000000 ) ) ;
#102211 = AXIS2_PLACEMENT_3D ( 'NONE', #43118, #103304, #13611 ) ;
#102212 = ORIENTED_EDGE ( 'NONE', *, *, #40226, .F. ) ;
#102213 = VERTEX_POINT ( 'NONE', #104740 ) ;
#102214 = DIRECTION ( 'NONE',  ( 0.000000000000000000, 0.000000000000000000, -1.000000000000000000 ) ) ;
#102215 = DIRECTION ( 'NONE',  ( 0.000000000000000000, 0.000000000000000000, 1.000000000000000000 ) ) ;
#102216 = CARTESIAN_POINT ( 'NONE',  ( 6.449999999999930012, 2.500000000000000000, 6.741600689897071952 ) ) ;
#102217 = DIRECTION ( 'NONE',  ( 0.000000000000000000, 0.000000000000000000, -1.000000000000000000 ) ) ;
#102218 = ORIENTED_EDGE ( 'NONE', *, *, #49773, .T. ) ;
#102219 = CONICAL_SURFACE ( 'NONE', #118934, 0.1000000000000002554, 0.003490658503988666988 ) ;
#102220 = DIRECTION ( 'NONE',  ( 0.000000000000000000, 1.000000000000000000, 0.000000000000000000 ) ) ;
#102221 = DIRECTION ( 'NONE',  ( 0.000000000000000000, 0.000000000000000000, 1.000000000000000000 ) ) ;
#102222 = AXIS2_PLACEMENT_3D ( 'NONE', #41335, #111315, #124227 ) ;
#102223 = VERTEX_POINT ( 'NONE', #24268 ) ;
#102224 = DIRECTION ( 'NONE',  ( 0.000000000000000000, -0.000000000000000000, 1.000000000000000000 ) ) ;
#102225 = ORIENTED_EDGE ( 'NONE', *, *, #114548, .F. ) ;
#102226 = CARTESIAN_POINT ( 'NONE',  ( 11.69999999999990870, 2.500000000000000000, -4.330127018922201643 ) ) ;
#102227 = EDGE_CURVE ( 'NONE', #54972, #55284, #101555, .T. ) ;
#102228 = ORIENTED_EDGE ( 'NONE', *, *, #85250, .F. ) ;
#102229 = AXIS2_PLACEMENT_3D ( 'NONE', #120828, #22005, #51460 ) ;
#102230 = CARTESIAN_POINT ( 'NONE',  ( 12.04999999999990834, 2.500000000000000000, 6.495190528383297135 ) ) ;
#102231 = CARTESIAN_POINT ( 'NONE',  ( 0.5999999999999555689, 2.500000000000000000, 4.676537180435972552 ) ) ;
#102232 = EDGE_CURVE ( 'NONE', #57293, #21757, #3343, .T. ) ;
#102233 = ORIENTED_EDGE ( 'NONE', *, *, #129605, .T. ) ;
#102234 = ORIENTED_EDGE ( 'NONE', *, *, #124509, .T. ) ;
#102235 = CARTESIAN_POINT ( 'NONE',  ( 187.3385416670080872, 6.551208109652274736, 3.782341765625001351 ) ) ;
#102236 = PLANE ( 'NONE',  #110374 ) ;
#102237 = VECTOR ( 'NONE', #112915, 1000.000000000000000 ) ;
#102238 = DIRECTION ( 'NONE',  ( -0.000000000000000000, 1.000000000000000000, -0.000000000000000000 ) ) ;
#102239 = CARTESIAN_POINT ( 'NONE',  ( 183.9843750003414016, -8.734944146203032389, -1.604583208406767949E-15 ) ) ;
#102240 = VECTOR ( 'NONE', #33774, 1000.000000000000000 ) ;
#102241 = DIRECTION ( 'NONE',  ( 0.000000000000000000, -0.000000000000000000, 1.000000000000000000 ) ) ;
#102242 = CARTESIAN_POINT ( 'NONE',  ( -0.4500000000000397571, 2.500000000000000000, -2.265063509461101798 ) ) ;
#102243 = DIRECTION ( 'NONE',  ( 0.000000000000000000, 0.000000000000000000, -1.000000000000000000 ) ) ;
#102244 = DIRECTION ( 'NONE',  ( 0.000000000000000000, -0.9999939076577903929, 0.003490651415223739937 ) ) ;
#102245 = DIRECTION ( 'NONE',  ( 0.000000000000000000, 1.000000000000000000, 0.000000000000000000 ) ) ;
#102246 = AXIS2_PLACEMENT_3D ( 'NONE', #14675, #63150, #84721 ) ;
#102247 = ORIENTED_EDGE ( 'NONE', *, *, #22729, .F. ) ;
#102248 = ORIENTED_EDGE ( 'NONE', *, *, #26535, .F. ) ;
#102249 = LINE ( 'NONE', #91774, #38166 ) ;
#102250 = CONICAL_SURFACE ( 'NONE', #112715, 0.09999999999999999167, 0.003490658503988666988 ) ;
#102251 = VERTEX_POINT ( 'NONE', #121819 ) ;
#102252 = PLANE ( 'NONE',  #62155 ) ;
#102253 = CARTESIAN_POINT ( 'NONE',  ( -7.100000000000013856, 2.500000000000000000, 5.022947341949748790 ) ) ;
#102254 = DIRECTION ( 'NONE',  ( 0.000000000000000000, 0.000000000000000000, 1.000000000000000000 ) ) ;
#102255 = CIRCLE ( 'NONE', #64589, 0.1000000000000002554 ) ;
#102257 = VERTEX_POINT ( 'NONE', #53730 ) ;
#102256 = ORIENTED_EDGE ( 'NONE', *, *, #83534, .T. ) ;
#102258 = FACE_BOUND ( 'NONE', #6897, .T. ) ;
#102259 = ORIENTED_EDGE ( 'NONE', *, *, #31418, .F. ) ;
#102260 = DIRECTION ( 'NONE',  ( 0.000000000000000000, 0.000000000000000000, 1.000000000000000000 ) ) ;
#102261 = DIRECTION ( 'NONE',  ( 0.000000000000000000, 0.000000000000000000, -1.000000000000000000 ) ) ;
#102262 = DIRECTION ( 'NONE',  ( 0.000000000000000000, -0.000000000000000000, 1.000000000000000000 ) ) ;
#102264 = CARTESIAN_POINT ( 'NONE',  ( 6.649999999999928413, 2.500000000000000000, 1.372243186433545370 ) ) ;
#102263 = AXIS2_PLACEMENT_3D ( 'NONE', #24721, #43737, #33270 ) ;
#102265 = DIRECTION ( 'NONE',  ( -0.000000000000000000, 1.000000000000000000, -0.000000000000000000 ) ) ;
#102266 = CARTESIAN_POINT ( 'NONE',  ( -3.750000000000029310, 2.500000000000000000, -7.188010851410854052 ) ) ;
#102267 = CARTESIAN_POINT ( 'NONE',  ( 9.199999999999919353, 12.50000000000000000, 0.06509327318403515528 ) ) ;
#102268 = DIRECTION ( 'NONE',  ( -4.274815082592931898E-19, -0.9999939076577903929, -0.003490651415223739937 ) ) ;
#102269 = DIRECTION ( 'NONE',  ( -0.000000000000000000, -1.000000000000000000, -0.000000000000000000 ) ) ;
#102270 = DIRECTION ( 'NONE',  ( 0.000000000000000000, 1.000000000000000000, 0.000000000000000000 ) ) ;
#102271 = FACE_OUTER_BOUND ( 'NONE', #73909, .T. ) ;
#102272 = ADVANCED_FACE ( 'NONE', ( #32823 ), #127746, .T. ) ;
#102273 = ORIENTED_EDGE ( 'NONE', *, *, #101908, .T. ) ;
#102274 = VERTEX_POINT ( 'NONE', #64830 ) ;
#102275 = EDGE_LOOP ( 'NONE', ( #40547, #77314 ) ) ;
#102276 = DIRECTION ( 'NONE',  ( -0.000000000000000000, 1.000000000000000000, -0.000000000000000000 ) ) ;
#102277 = VERTEX_POINT ( 'NONE', #22359 ) ;
#102278 = CARTESIAN_POINT ( 'NONE',  ( 12.89999999999990266, 2.500000000000000000, -5.022947341949754119 ) ) ;
#102279 = AXIS2_PLACEMENT_3D ( 'NONE', #104958, #5474, #85341 ) ;
#102280 = DIRECTION ( 'NONE',  ( -0.000000000000000000, 1.000000000000000000, -0.000000000000000000 ) ) ;
#102282 = VERTEX_POINT ( 'NONE', #3976 ) ;
#102281 = ORIENTED_EDGE ( 'NONE', *, *, #34648, .F. ) ;
#102283 = ORIENTED_EDGE ( 'NONE', *, *, #77731, .T. ) ;
#102284 = DIRECTION ( 'NONE',  ( 0.000000000000000000, 1.000000000000000000, 0.000000000000000000 ) ) ;
#102285 = AXIS2_PLACEMENT_3D ( 'NONE', #60807, #62750, #123575 ) ;
#102286 = AXIS2_PLACEMENT_3D ( 'NONE', #48387, #8439, #79154 ) ;
#102287 = CARTESIAN_POINT ( 'NONE',  ( 4.399999999999937295, 12.50000000000000000, 4.676537180435972552 ) ) ;
#102288 = FACE_OUTER_BOUND ( 'NONE', #116984, .T. ) ;
#102289 = CARTESIAN_POINT ( 'NONE',  ( 185.4479166673494603, -6.668395609140176816, -3.850000000000003642 ) ) ;
#102290 = EDGE_CURVE ( 'NONE', #102251, #86684, #44117, .T. ) ;
#102291 = CARTESIAN_POINT ( 'NONE',  ( -1.900000000000034106, 2.500000000000000000, -4.083716857408426826 ) ) ;
#102292 = EDGE_CURVE ( 'NONE', #111573, #54835, #4589, .T. ) ;
#102293 = EDGE_LOOP ( 'NONE', ( #3989, #110492 ) ) ;
#102294 = CIRCLE ( 'NONE', #77238, 0.1000000000000002554 ) ;
#102296 = CARTESIAN_POINT ( 'NONE',  ( -3.950000000000029932, 12.50000000000000000, -6.148780366869526226 ) ) ;
#102295 = VECTOR ( 'NONE', #77025, 1000.000000000000000 ) ;
#102297 = ORIENTED_EDGE ( 'NONE', *, *, #35571, .T. ) ;
#102298 = VECTOR ( 'NONE', #35479, 1000.000000000000000 ) ;
#102299 = EDGE_LOOP ( 'NONE', ( #89188, #23615 ) ) ;
#102300 = EDGE_LOOP ( 'NONE', ( #31348, #53863 ) ) ;
#102301 = DIRECTION ( 'NONE',  ( -0.000000000000000000, -1.000000000000000000, -0.000000000000000000 ) ) ;
#102302 = ORIENTED_EDGE ( 'NONE', *, *, #14671, .T. ) ;
#102303 = EDGE_CURVE ( 'NONE', #124247, #75500, #98478, .T. ) ;
#102304 = ORIENTED_EDGE ( 'NONE', *, *, #78094, .F. ) ;
#102305 = VERTEX_POINT ( 'NONE', #103479 ) ;
#102306 = AXIS2_PLACEMENT_3D ( 'NONE', #80160, #99806, #50696 ) ;
#102307 = FILL_AREA_STYLE_COLOUR ( '', #102920 ) ;
#102308 = CIRCLE ( 'NONE', #114891, 0.1000000000000002554 ) ;
#102309 = PLANE ( 'NONE',  #101988 ) ;
#102310 = CARTESIAN_POINT ( 'NONE',  ( 6.649999999999929301, 2.500000000000000000, 6.495190528383297135 ) ) ;
#102311 = CIRCLE ( 'NONE', #54272, 0.1000000000000002554 ) ;
#102312 = CARTESIAN_POINT ( 'NONE',  ( -9.600000000000008527, 12.50000000000000000, -5.022947341949749678 ) ) ;
#102313 = DIRECTION ( 'NONE',  ( 0.000000000000000000, 1.000000000000000000, 0.000000000000000000 ) ) ;
#102314 = CARTESIAN_POINT ( 'NONE',  ( 9.349999999999919709, 2.500000000000000000, 1.818653347947321475 ) ) ;
#102315 = CARTESIAN_POINT ( 'NONE',  ( 5.849999999999933031, 12.50000000000000000, -1.472243186433550122 ) ) ;
#102316 = ORIENTED_EDGE ( 'NONE', *, *, #5818, .F. ) ;
#102317 = FACE_OUTER_BOUND ( 'NONE', #52470, .T. ) ;
#102318 = ORIENTED_EDGE ( 'NONE', *, *, #129283, .T. ) ;
#102319 = DIRECTION ( 'NONE',  ( -4.274815082592931898E-19, -0.9999939076577903929, -0.003490651415223739937 ) ) ;
#102320 = CIRCLE ( 'NONE', #112784, 0.06509327318403743123 ) ;
#102321 = VERTEX_POINT ( 'NONE', #34756 ) ;
#102322 = CARTESIAN_POINT ( 'NONE',  ( 0.1999999999999576006, 12.50000000000000000, -4.741630453620016006 ) ) ;
#102323 = VERTEX_POINT ( 'NONE', #83204 ) ;
#102324 = CARTESIAN_POINT ( 'NONE',  ( 184.2343750003414016, 8.734944146203032389, 5.348610694689227483E-16 ) ) ;
#102325 = EDGE_CURVE ( 'NONE', #74675, #33200, #112656, .T. ) ;
#102326 = DIRECTION ( 'NONE',  ( -0.000000000000000000, -1.000000000000000000, -0.000000000000000000 ) ) ;
#102327 = VERTEX_POINT ( 'NONE', #64188 ) ;
#102328 = EDGE_LOOP ( 'NONE', ( #2366, #52599, #92780, #2452 ) ) ;
#102329 = CARTESIAN_POINT ( 'NONE',  ( -2.499999999999996447, 2.500000000000000000, 4.330127018922196314 ) ) ;
#102330 = DIRECTION ( 'NONE',  ( 0.000000000000000000, -0.000000000000000000, 1.000000000000000000 ) ) ;
#102331 = EDGE_CURVE ( 'NONE', #81523, #51798, #67162, .T. ) ;
#102332 = DIRECTION ( 'NONE',  ( 0.000000000000000000, 0.000000000000000000, -1.000000000000000000 ) ) ;
#102334 = AXIS2_PLACEMENT_3D ( 'NONE', #103599, #51923, #91840 ) ;
#102333 = FACE_OUTER_BOUND ( 'NONE', #49626, .T. ) ;
#102335 = ADVANCED_FACE ( 'NONE', ( #91723 ), #93660, .T. ) ;
#102336 = CARTESIAN_POINT ( 'NONE',  ( 9.599999999999914380, 2.500000000000000000, 4.330127018922196314 ) ) ;
#102337 = ORIENTED_EDGE ( 'NONE', *, *, #92082, .T. ) ;
#102338 = DIRECTION ( 'NONE',  ( -0.000000000000000000, 1.000000000000000000, -0.000000000000000000 ) ) ;
#102339 = EDGE_CURVE ( 'NONE', #89915, #34182, #27371, .T. ) ;
#102340 = ADVANCED_FACE ( 'NONE', ( #33464 ), #50470, .T. ) ;
#102341 = CONICAL_SURFACE ( 'NONE', #35442, 0.1000000000000002554, 0.003490658503988666988 ) ;
#102342 = EDGE_CURVE ( 'NONE', #62801, #123416, #46260, .T. ) ;
#102343 = ORIENTED_EDGE ( 'NONE', *, *, #26649, .T. ) ;
#102344 = PLANE ( 'NONE',  #13015 ) ;
#102345 = CARTESIAN_POINT ( 'NONE',  ( -7.950000000000016165, 2.500000000000000000, -6.495190528383297135 ) ) ;
#102348 = ADVANCED_FACE ( 'NONE', ( #115869 ), #123615, .T. ) ;
#102347 = CIRCLE ( 'NONE', #62639, 0.06509327318403741736 ) ;
#102346 = AXIS2_PLACEMENT_3D ( 'NONE', #68515, #99283, #46965 ) ;
#102349 = CIRCLE ( 'NONE', #20866, 0.06509327318403745899 ) ;
#102350 = CARTESIAN_POINT ( 'NONE',  ( 6.449999999999931788, 2.500000000000000000, 6.148780366869520009 ) ) ;
#102351 = LINE ( 'NONE', #91879, #122139 ) ;
#102352 = PLANE ( 'NONE',  #113467 ) ;
#102353 = DIRECTION ( 'NONE',  ( 0.000000000000000000, 0.000000000000000000, 1.000000000000000000 ) ) ;
#102354 = CARTESIAN_POINT ( 'NONE',  ( 13.74999999999993072, 2.500000000000000000, -2.165063509461101710 ) ) ;
#102355 = ORIENTED_EDGE ( 'NONE', *, *, #39428, .T. ) ;
#102356 = EDGE_CURVE ( 'NONE', #107669, #87317, #100549, .T. ) ;
#102358 = AXIS2_PLACEMENT_3D ( 'NONE', #15403, #55352, #25890 ) ;
#102357 = AXIS2_PLACEMENT_3D ( 'NONE', #6330, #118896, #16796 ) ;
#102359 = DIRECTION ( 'NONE',  ( 0.000000000000000000, 0.000000000000000000, -1.000000000000000000 ) ) ;
#102360 = LINE ( 'NONE', #72893, #67253 ) ;
#102361 = CARTESIAN_POINT ( 'NONE',  ( -8.150000000000012790, 2.500000000000000000, 1.818653347947321475 ) ) ;
#102362 = ORIENTED_EDGE ( 'NONE', *, *, #121513, .T. ) ;
#102363 = ORIENTED_EDGE ( 'NONE', *, *, #37209, .F. ) ;
#102364 = CARTESIAN_POINT ( 'NONE',  ( -12.09999999999999432, 2.500000000000000000, 5.022947341949748790 ) ) ;
#102365 = ORIENTED_EDGE ( 'NONE', *, *, #100227, .F. ) ;
#102366 = EDGE_LOOP ( 'NONE', ( #49001, #75027 ) ) ;
#102367 = FACE_OUTER_BOUND ( 'NONE', #41834, .T. ) ;
#102368 = AXIS2_PLACEMENT_3D ( 'NONE', #2101, #825, #11285 ) ;
#102369 = ORIENTED_EDGE ( 'NONE', *, *, #65125, .F. ) ;
#102370 = CARTESIAN_POINT ( 'NONE',  ( 19.21290572970430333, -2.587129408759125226, -2.394140119533374911 ) ) ;
#102371 = DIRECTION ( 'NONE',  ( 0.000000000000000000, 0.000000000000000000, -1.000000000000000000 ) ) ;
#102372 = FACE_OUTER_BOUND ( 'NONE', #2060, .T. ) ;
#102373 = ORIENTED_EDGE ( 'NONE', *, *, #25813, .F. ) ;
#102374 = CIRCLE ( 'NONE', #62669, 0.09999999999999999167 ) ;
#102375 = CARTESIAN_POINT ( 'NONE',  ( -3.350000000000029399, 12.50000000000000000, 6.495190528383297135 ) ) ;
#102376 = CONICAL_SURFACE ( 'NONE', #45947, 0.1000000000000000472, 0.003490658503988666988 ) ;
#102377 = DIRECTION ( 'NONE',  ( 0.000000000000000000, 0.000000000000000000, -1.000000000000000000 ) ) ;
#102378 = AXIS2_PLACEMENT_3D ( 'NONE', #108120, #8611, #9925 ) ;
#102379 = ORIENTED_EDGE ( 'NONE', *, *, #62035, .F. ) ;
#102381 = AXIS2_PLACEMENT_3D ( 'NONE', #6616, #26947, #76689 ) ;
#102380 = AXIS2_PLACEMENT_3D ( 'NONE', #21996, #69129, #71715 ) ;
#102383 = ORIENTED_EDGE ( 'NONE', *, *, #80457, .T. ) ;
#102382 = ADVANCED_FACE ( 'NONE', ( #127624 ), #23272, .T. ) ;
#102384 = ORIENTED_EDGE ( 'NONE', *, *, #67373, .F. ) ;
#102385 = CARTESIAN_POINT ( 'NONE',  ( 7.899999999999924860, 12.50000000000000000, 5.022947341949748790 ) ) ;
#102386 = DIRECTION ( 'NONE',  ( 0.000000000000000000, 1.000000000000000000, 0.000000000000000000 ) ) ;
#102387 = FACE_BOUND ( 'NONE', #5716, .T. ) ;
#102388 = ORIENTED_EDGE ( 'NONE', *, *, #48959, .T. ) ;
#102389 = AXIS2_PLACEMENT_3D ( 'NONE', #112049, #11904, #11253 ) ;
#102390 = DIRECTION ( 'NONE',  ( 0.000000000000000000, -0.000000000000000000, 1.000000000000000000 ) ) ;
#102391 = DIRECTION ( 'NONE',  ( 0.000000000000000000, 1.000000000000000000, 0.000000000000000000 ) ) ;
#102392 = ORIENTED_EDGE ( 'NONE', *, *, #92132, .T. ) ;
#102393 = EDGE_CURVE ( 'NONE', #51917, #59583, #26206, .T. ) ;
#102394 = DIRECTION ( 'NONE',  ( 0.000000000000000000, 0.000000000000000000, 1.000000000000000000 ) ) ;
#102395 = DIRECTION ( 'NONE',  ( 0.000000000000000000, 1.000000000000000000, 0.000000000000000000 ) ) ;
#102396 = AXIS2_PLACEMENT_3D ( 'NONE', #70807, #110092, #32839 ) ;
#102397 = DIRECTION ( 'NONE',  ( -4.274815082592931898E-19, -0.9999939076577903929, -0.003490651415223739937 ) ) ;
#102398 = CARTESIAN_POINT ( 'NONE',  ( -9.600000000000006750, 12.50000000000000000, 5.022947341949748790 ) ) ;
#102399 = DIRECTION ( 'NONE',  ( 0.000000000000000000, 0.000000000000000000, 1.000000000000000000 ) ) ;
#102400 = CARTESIAN_POINT ( 'NONE',  ( -9.200000000000006395, 12.50000000000000000, 4.330127018922196314 ) ) ;
#102401 = DIRECTION ( 'NONE',  ( -0.000000000000000000, -1.000000000000000000, -0.000000000000000000 ) ) ;
#102402 = AXIS2_PLACEMENT_3D ( 'NONE', #37152, #27300, #85589 ) ;
#102403 = ORIENTED_EDGE ( 'NONE', *, *, #106338, .T. ) ;
#102404 = VERTEX_POINT ( 'NONE', #57607 ) ;
#102405 = VERTEX_POINT ( 'NONE', #85755 ) ;
#102406 = ORIENTED_EDGE ( 'NONE', *, *, #49462, .T. ) ;
#102407 = CONICAL_SURFACE ( 'NONE', #106508, 0.1000000000000000472, 0.003490658503988666988 ) ;
#102408 = DIRECTION ( 'NONE',  ( -0.000000000000000000, 1.000000000000000000, -0.000000000000000000 ) ) ;
#102409 = LINE ( 'NONE', #82117, #118890 ) ;
#102410 = DIRECTION ( 'NONE',  ( 0.000000000000000000, -0.9999939076577903929, 0.003490651415223739937 ) ) ;
#102411 = EDGE_LOOP ( 'NONE', ( #21949, #54618, #76421, #108183 ) ) ;
#102412 = FACE_BOUND ( 'NONE', #113960, .T. ) ;
#102413 = PLANE ( 'NONE',  #100217 ) ;
#102414 = CARTESIAN_POINT ( 'NONE',  ( -1.450000000000035927, 2.500000000000000000, -1.818653347947326138 ) ) ;
#102415 = CARTESIAN_POINT ( 'NONE',  ( 129.5000000000000000, 0.9999999999999985567, 7.634788798650556707 ) ) ;
#102416 = FACE_OUTER_BOUND ( 'NONE', #31162, .T. ) ;
#102417 = DIRECTION ( 'NONE',  ( 0.000000000000000000, 1.000000000000000000, 0.000000000000000000 ) ) ;
#102418 = CARTESIAN_POINT ( 'NONE',  ( 185.5000000000000000, 0.000000000000000000, 7.700000000000000178 ) ) ;
#102419 = CARTESIAN_POINT ( 'NONE',  ( 10.84999999999991260, 2.500000000000000000, -2.757883832488654097 ) ) ;
#102420 = DIRECTION ( 'NONE',  ( 0.000000000000000000, 0.000000000000000000, -1.000000000000000000 ) ) ;
#102421 = DIRECTION ( 'NONE',  ( 0.000000000000000000, 1.000000000000000000, 0.000000000000000000 ) ) ;
#102422 = EDGE_LOOP ( 'NONE', ( #83669, #87365 ) ) ;
#102423 = EDGE_CURVE ( 'NONE', #110342, #27555, #75496, .T. ) ;
#102424 = EDGE_LOOP ( 'NONE', ( #78704, #31080 ) ) ;
#102425 = EDGE_LOOP ( 'NONE', ( #3704, #45741 ) ) ;
#102426 = VERTEX_POINT ( 'NONE', #26848 ) ;
#102427 = ORIENTED_EDGE ( 'NONE', *, *, #112739, .F. ) ;
#102428 = VERTEX_POINT ( 'NONE', #45849 ) ;
#102429 = DIRECTION ( 'NONE',  ( -0.000000000000000000, -1.000000000000000000, -0.000000000000000000 ) ) ;
#102430 = AXIS2_PLACEMENT_3D ( 'NONE', #18237, #68627, #129521 ) ;
#102431 = ORIENTED_EDGE ( 'NONE', *, *, #42125, .F. ) ;
#102432 = VERTEX_POINT ( 'NONE', #5259 ) ;
#102433 = EDGE_CURVE ( 'NONE', #114003, #57219, #96420, .T. ) ;
#102436 = AXIS2_PLACEMENT_3D ( 'NONE', #97867, #48136, #88021 ) ;
#102435 = CARTESIAN_POINT ( 'NONE',  ( 4.149999999999941735, 2.500000000000000000, -7.188010851410854052 ) ) ;
#102434 = AXIS2_PLACEMENT_3D ( 'NONE', #17302, #56597, #96517 ) ;
#102437 = CARTESIAN_POINT ( 'NONE',  ( 13.80679872386857276, -1.499999999999904077, 7.946844943073641865 ) ) ;
#102438 = CARTESIAN_POINT ( 'NONE',  ( -2.300000000000033129, 2.500000000000000000, 4.083716857408420609 ) ) ;
#102439 = DIRECTION ( 'NONE',  ( 0.000000000000000000, -0.000000000000000000, 1.000000000000000000 ) ) ;
#102440 = ADVANCED_FACE ( 'NONE', ( #36025 ), #58793, .T. ) ;
#102441 = EDGE_CURVE ( 'NONE', #14735, #42734, #4379, .T. ) ;
#102442 = ORIENTED_EDGE ( 'NONE', *, *, #27397, .F. ) ;
#102443 = DIRECTION ( 'NONE',  ( 0.000000000000000000, 1.000000000000000000, 0.000000000000000000 ) ) ;
#102445 = AXIS2_PLACEMENT_3D ( 'NONE', #15738, #54379, #114583 ) ;
#102444 = CIRCLE ( 'NONE', #100388, 0.1000000000000000472 ) ;
#102446 = ORIENTED_EDGE ( 'NONE', *, *, #1160, .F. ) ;
#102447 = ORIENTED_EDGE ( 'NONE', *, *, #48257, .F. ) ;
#102448 = DIRECTION ( 'NONE',  ( -4.274815082592931898E-19, -0.9999939076577903929, -0.003490651415223739937 ) ) ;
#102449 = EDGE_CURVE ( 'NONE', #101033, #64350, #77556, .T. ) ;
#102450 = DIRECTION ( 'NONE',  ( 0.000000000000000000, 0.000000000000000000, 1.000000000000000000 ) ) ;
#102451 = EDGE_CURVE ( 'NONE', #20100, #106061, #48323, .T. ) ;
#102452 = ORIENTED_EDGE ( 'NONE', *, *, #51656, .F. ) ;
#102453 = ORIENTED_EDGE ( 'NONE', *, *, #25311, .T. ) ;
#102454 = DIRECTION ( 'NONE',  ( -0.000000000000000000, 1.000000000000000000, -0.000000000000000000 ) ) ;
#102455 = DIRECTION ( 'NONE',  ( 0.000000000000000000, 0.000000000000000000, 1.000000000000000000 ) ) ;
#102456 = FACE_OUTER_BOUND ( 'NONE', #55344, .T. ) ;
#102457 = DIRECTION ( 'NONE',  ( -0.000000000000000000, -1.000000000000000000, -0.000000000000000000 ) ) ;
#102458 = CARTESIAN_POINT ( 'NONE',  ( -6.650000000000014566, 2.500000000000000000, 6.495190528383297135 ) ) ;
#102459 = ORIENTED_EDGE ( 'NONE', *, *, #128163, .T. ) ;
#102460 = CARTESIAN_POINT ( 'NONE',  ( 10.19999999999991580, 12.50000000000000000, -0.3464101615137783474 ) ) ;
#102461 = AXIS2_PLACEMENT_3D ( 'NONE', #26149, #97460, #45794 ) ;
#102462 = VECTOR ( 'NONE', #80411, 1000.000000000000000 ) ;
#102463 = ORIENTED_EDGE ( 'NONE', *, *, #82727, .F. ) ;
#102464 = CARTESIAN_POINT ( 'NONE',  ( 87.50000000000001421, 3.974992050023848922, -6.359987280038160051 ) ) ;
#102465 = LINE ( 'NONE', #54013, #12853 ) ;
#102466 = CARTESIAN_POINT ( 'NONE',  ( -7.700000000000016165, 2.500000000000000000, -3.883716857408426648 ) ) ;
#102467 = DIRECTION ( 'NONE',  ( -0.000000000000000000, 1.000000000000000000, -0.000000000000000000 ) ) ;
#102468 = CARTESIAN_POINT ( 'NONE',  ( -7.499999999999980460, 2.500000000000000000, -4.330127018922201643 ) ) ;
#102469 = ORIENTED_EDGE ( 'NONE', *, *, #111776, .T. ) ;
#102470 = CIRCLE ( 'NONE', #79496, 0.06509327318403745899 ) ;
#102471 = CARTESIAN_POINT ( 'NONE',  ( 11.44999999999991047, 12.50000000000000000, -2.511473670974877948 ) ) ;
#102472 = PLANE ( 'NONE',  #79982 ) ;
#102473 = ORIENTED_EDGE ( 'NONE', *, *, #126674, .T. ) ;
#102474 = EDGE_LOOP ( 'NONE', ( #86109, #106914 ) ) ;
#102475 = ORIENTED_EDGE ( 'NONE', *, *, #74269, .T. ) ;
#102476 = DIRECTION ( 'NONE',  ( -0.000000000000000000, -1.000000000000000000, -0.000000000000000000 ) ) ;
#102477 = DIRECTION ( 'NONE',  ( 0.000000000000000000, 1.000000000000000000, 0.000000000000000000 ) ) ;
#102478 = CARTESIAN_POINT ( 'NONE',  ( 186.7760416670080588, 6.551208109652274736, 3.782341765625001351 ) ) ;
#102479 = AXIS2_PLACEMENT_3D ( 'NONE', #9664, #129470, #79688 ) ;
#102480 = CARTESIAN_POINT ( 'NONE',  ( -5.000000000000022204, 2.500000000000000000, 3.637306695894644726 ) ) ;
#102482 = EDGE_CURVE ( 'NONE', #46048, #21956, #21132, .T. ) ;
#102481 = DIRECTION ( 'NONE',  ( 0.000000000000000000, -0.9999939076577903929, 0.003490651415223739937 ) ) ;
#102483 = CIRCLE ( 'NONE', #18931, 0.09999999999999982514 ) ;
#102484 = CARTESIAN_POINT ( 'NONE',  ( 10.84999999999991260, 12.50000000000000000, -2.857883832488653741 ) ) ;
#102485 = PLANE ( 'NONE',  #562 ) ;
#102486 = EDGE_CURVE ( 'NONE', #129134, #44639, #126344, .T. ) ;
#102487 = ADVANCED_FACE ( 'NONE', ( #95591 ), #2330, .T. ) ;
#102488 = EDGE_CURVE ( 'NONE', #114610, #109551, #65021, .T. ) ;
#102490 = ADVANCED_FACE ( 'NONE', ( #126987 ), #17662, .T. ) ;
#102489 = VECTOR ( 'NONE', #24136, 1000.000000000000000 ) ;
#102491 = CARTESIAN_POINT ( 'NONE',  ( -11.64999999999999680, 2.500000000000000000, 2.957883832488649389 ) ) ;
#102492 = ORIENTED_EDGE ( 'NONE', *, *, #58004, .T. ) ;
#102493 = EDGE_CURVE ( 'NONE', #102028, #56755, #92225, .T. ) ;
#102494 = AXIS2_PLACEMENT_3D ( 'NONE', #128978, #127026, #68082 ) ;
#102495 = DIRECTION ( 'NONE',  ( 0.000000000000000000, 1.000000000000000000, 0.000000000000000000 ) ) ;
#102496 = DIRECTION ( 'NONE',  ( 0.000000000000000000, 1.000000000000000000, 0.000000000000000000 ) ) ;
#102497 = CARTESIAN_POINT ( 'NONE',  ( -0.6000000000000323963, 12.50000000000000000, 0.3464101615137759604 ) ) ;
#102498 = PLANE ( 'NONE',  #104395 ) ;
#102499 = ORIENTED_EDGE ( 'NONE', *, *, #91357, .F. ) ;
#102500 = ADVANCED_FACE ( 'NONE', ( #7839 ), #97514, .T. ) ;
#102501 = DIRECTION ( 'NONE',  ( 0.000000000000000000, -0.000000000000000000, 1.000000000000000000 ) ) ;
#102502 = EDGE_CURVE ( 'NONE', #66522, #63978, #118442, .T. ) ;
#102503 = DIRECTION ( 'NONE',  ( 0.000000000000000000, -0.9999939076577903929, 0.003490651415223739937 ) ) ;
#102505 = ORIENTED_EDGE ( 'NONE', *, *, #50400, .T. ) ;
#102504 = CARTESIAN_POINT ( 'NONE',  ( 6.899999999999928413, 2.500000000000000000, 3.983716857408420964 ) ) ;
#102506 = VERTEX_POINT ( 'NONE', #19609 ) ;
#102507 = DIRECTION ( 'NONE',  ( 0.000000000000000000, 1.000000000000000000, 0.000000000000000000 ) ) ;
#102508 = ORIENTED_EDGE ( 'NONE', *, *, #55509, .F. ) ;
#102509 = ORIENTED_EDGE ( 'NONE', *, *, #36877, .F. ) ;
#102510 = CARTESIAN_POINT ( 'NONE',  ( -4.150000000000028777, 2.500000000000000000, -5.802370205355749988 ) ) ;
#102511 = AXIS2_PLACEMENT_3D ( 'NONE', #112438, #20830, #22138 ) ;
#102512 = CARTESIAN_POINT ( 'NONE',  ( -2.950000000000033484, 12.50000000000000000, -6.560283801567339701 ) ) ;
#102513 = CARTESIAN_POINT ( 'NONE',  ( -12.69999999999999396, 2.500000000000000000, -3.883716857408423984 ) ) ;
#102514 = DIRECTION ( 'NONE',  ( 0.000000000000000000, 1.000000000000000000, 0.000000000000000000 ) ) ;
#102515 = EDGE_LOOP ( 'NONE', ( #59448, #115400 ) ) ;
#102516 = CIRCLE ( 'NONE', #2165, 0.06509327318403745899 ) ;
#102517 = CARTESIAN_POINT ( 'NONE',  ( -9.550000000000002487, 12.50000000000000000, 6.560283801567334372 ) ) ;
#102519 = ORIENTED_EDGE ( 'NONE', *, *, #41005, .T. ) ;
#102518 = CARTESIAN_POINT ( 'NONE',  ( 129.5000000000000000, 1.500000000000000000, 0.000000000000000000 ) ) ;
#102520 = CARTESIAN_POINT ( 'NONE',  ( 17.48307833624052066, 2.102402844588128428, 4.293715869771017601 ) ) ;
#102521 = DIRECTION ( 'NONE',  ( 0.000000000000000000, -0.000000000000000000, 1.000000000000000000 ) ) ;
#102522 = VERTEX_POINT ( 'NONE', #90928 ) ;
#102523 = EDGE_LOOP ( 'NONE', ( #98886, #26844 ) ) ;
#102524 = ORIENTED_EDGE ( 'NONE', *, *, #116953, .F. ) ;
#102525 = VERTEX_POINT ( 'NONE', #70006 ) ;
#102526 = PLANE ( 'NONE',  #64987 ) ;
#102527 = CARTESIAN_POINT ( 'NONE',  ( -10.85000000000000142, 2.500000000000000000, -6.395190528383298378 ) ) ;
#102528 = CARTESIAN_POINT ( 'NONE',  ( -3.350000000000028511, 2.500000000000000000, 2.957883832488649389 ) ) ;
#102529 = FACE_BOUND ( 'NONE', #104855, .T. ) ;
#102530 = ORIENTED_EDGE ( 'NONE', *, *, #55775, .T. ) ;
#102531 = CARTESIAN_POINT ( 'NONE',  ( 184.5729166673494603, 4.445597072760120838, -7.699999999999998401 ) ) ;
#102532 = DIRECTION ( 'NONE',  ( -0.000000000000000000, 1.000000000000000000, -0.000000000000000000 ) ) ;
#102533 = DIRECTION ( 'NONE',  ( 0.000000000000000000, -0.000000000000000000, 1.000000000000000000 ) ) ;
#102534 = EDGE_CURVE ( 'NONE', #19850, #122843, #125668, .T. ) ;
#102535 = DIRECTION ( 'NONE',  ( 0.000000000000000000, 1.000000000000000000, 0.000000000000000000 ) ) ;
#102536 = DIRECTION ( 'NONE',  ( -0.7336674352944539956, 0.000000000000000000, -0.6795087154617358571 ) ) ;
#102537 = LINE ( 'NONE', #120889, #103578 ) ;
#102538 = VECTOR ( 'NONE', #78332, 1000.000000000000000 ) ;
#102539 = CARTESIAN_POINT ( 'NONE',  ( -1.650000000000035216, 2.500000000000000000, -1.472243186433550122 ) ) ;
#102540 = VERTEX_POINT ( 'NONE', #59568 ) ;
#102541 = EDGE_LOOP ( 'NONE', ( #55088, #113017, #18750, #75542 ) ) ;
#102542 = VERTEX_POINT ( 'NONE', #128288 ) ;
#102543 = VERTEX_POINT ( 'NONE', #49090 ) ;
#102544 = ORIENTED_EDGE ( 'NONE', *, *, #85776, .F. ) ;
#102545 = CARTESIAN_POINT ( 'NONE',  ( 179.5000000000000000, 1.375000000000000000, 7.634788798650556707 ) ) ;
#102546 = DIRECTION ( 'NONE',  ( 0.000000000000000000, 0.000000000000000000, 1.000000000000000000 ) ) ;
#102547 = ORIENTED_EDGE ( 'NONE', *, *, #32460, .T. ) ;
#102548 = FACE_BOUND ( 'NONE', #2491, .T. ) ;
#102549 = CIRCLE ( 'NONE', #48271, 0.06509327318403745899 ) ;
#102550 = FACE_OUTER_BOUND ( 'NONE', #14713, .T. ) ;
#102551 = EDGE_LOOP ( 'NONE', ( #44040, #25787, #42222, #63946 ) ) ;
#102552 = CARTESIAN_POINT ( 'NONE',  ( 6.449999999999931788, 2.500000000000000000, 6.048780366869520364 ) ) ;
#102553 = FACE_OUTER_BOUND ( 'NONE', #124998, .T. ) ;
#102554 = DIRECTION ( 'NONE',  ( 0.000000000000000000, -0.9999939076577903929, 0.003490651415223739937 ) ) ;
#102555 = ORIENTED_EDGE ( 'NONE', *, *, #65579, .F. ) ;
#102556 = CARTESIAN_POINT ( 'NONE',  ( 1.899999999999949507, 2.500000000000000000, 4.676537180435972552 ) ) ;
#102557 = CIRCLE ( 'NONE', #56581, 0.1000000000000002554 ) ;
#102558 = ORIENTED_EDGE ( 'NONE', *, *, #87417, .F. ) ;
#102559 = CIRCLE ( 'NONE', #6391, 0.06509327318403745899 ) ;
#102560 = ORIENTED_EDGE ( 'NONE', *, *, #25263, .F. ) ;
#102561 = EDGE_LOOP ( 'NONE', ( #119821, #126170, #71454, #109851 ) ) ;
#102562 = PLANE ( 'NONE',  #77895 ) ;
#102563 = CARTESIAN_POINT ( 'NONE',  ( -5.600000000000020073, 2.500000000000000000, 3.983716857408420964 ) ) ;
#102564 = CARTESIAN_POINT ( 'NONE',  ( -11.69999999999999929, 2.500000000000000000, 0.1000000000000017403 ) ) ;
#102565 = VERTEX_POINT ( 'NONE', #98797 ) ;
#102566 = CARTESIAN_POINT ( 'NONE',  ( 2.899999999999943956, 12.50000000000000000, 4.330127018922196314 ) ) ;
#102567 = EDGE_CURVE ( 'NONE', #81614, #20666, #11056, .T. ) ;
#102568 = DIRECTION ( 'NONE',  ( 0.000000000000000000, 0.000000000000000000, 1.000000000000000000 ) ) ;
#102569 = CARTESIAN_POINT ( 'NONE',  ( 4.149999999999939959, 2.500000000000000000, -2.265063509461101798 ) ) ;
#102570 = CONICAL_SURFACE ( 'NONE', #87890, 0.09999999999999982514, 0.003490658503988666988 ) ;
#102571 = CARTESIAN_POINT ( 'NONE',  ( 187.0729166673494319, 4.445597072760120838, -7.699999999999998401 ) ) ;
#102572 = ORIENTED_EDGE ( 'NONE', *, *, #74352, .T. ) ;
#102573 = EDGE_CURVE ( 'NONE', #65666, #39808, #18307, .T. ) ;
#102574 = DIRECTION ( 'NONE',  ( -0.000000000000000000, -1.000000000000000000, -0.000000000000000000 ) ) ;
#102575 = ADVANCED_FACE ( 'NONE', ( #89641 ), #73534, .T. ) ;
#102576 = ORIENTED_EDGE ( 'NONE', *, *, #53407, .F. ) ;
#102577 = FACE_OUTER_BOUND ( 'NONE', #104823, .T. ) ;
#102578 = ORIENTED_EDGE ( 'NONE', *, *, #77326, .F. ) ;
#102579 = ORIENTED_EDGE ( 'NONE', *, *, #123015, .T. ) ;
#102580 = DIRECTION ( 'NONE',  ( 0.000000000000000000, 0.000000000000000000, 1.000000000000000000 ) ) ;
#102581 = CARTESIAN_POINT ( 'NONE',  ( 6.049999999999932321, 12.50000000000000000, -1.818653347947326138 ) ) ;
#102582 = EDGE_CURVE ( 'NONE', #103695, #50900, #48414, .T. ) ;
#102583 = EDGE_CURVE ( 'NONE', #10632, #23431, #25408, .T. ) ;
#102584 = LINE ( 'NONE', #121578, #113490 ) ;
#102585 = EDGE_CURVE ( 'NONE', #1863, #101462, #17077, .T. ) ;
#102586 = DIRECTION ( 'NONE',  ( -4.274815082592931898E-19, -0.9999939076577903929, -0.003490651415223739937 ) ) ;
#102587 = EDGE_CURVE ( 'NONE', #101787, #57283, #54657, .T. ) ;
#102588 = DIRECTION ( 'NONE',  ( 0.000000000000000000, 1.000000000000000000, 0.000000000000000000 ) ) ;
#102589 = EDGE_LOOP ( 'NONE', ( #62425, #30626 ) ) ;
#102590 = ORIENTED_EDGE ( 'NONE', *, *, #99079, .T. ) ;
#102591 = DIRECTION ( 'NONE',  ( 0.000000000000000000, 1.000000000000000000, 0.000000000000000000 ) ) ;
#102592 = CARTESIAN_POINT ( 'NONE',  ( -10.40000000000000213, 2.500000000000000000, 4.330127018922196314 ) ) ;
#102594 = DIRECTION ( 'NONE',  ( -0.000000000000000000, 1.000000000000000000, -0.000000000000000000 ) ) ;
#102593 = CIRCLE ( 'NONE', #96328, 0.06509327318403745899 ) ;
#102595 = EDGE_LOOP ( 'NONE', ( #107329, #111784 ) ) ;
#102596 = ORIENTED_EDGE ( 'NONE', *, *, #72429, .T. ) ;
#102597 = CONICAL_SURFACE ( 'NONE', #119323, 0.1000000000000000472, 0.003490658503988666988 ) ;
#102598 = EDGE_CURVE ( 'NONE', #63617, #86820, #33835, .T. ) ;
#102599 = DIRECTION ( 'NONE',  ( 0.000000000000000000, 1.000000000000000000, 0.000000000000000000 ) ) ;
#102600 = ORIENTED_EDGE ( 'NONE', *, *, #126679, .T. ) ;
#102601 = DIRECTION ( 'NONE',  ( 0.000000000000000000, 0.000000000000000000, 1.000000000000000000 ) ) ;
#102602 = DIRECTION ( 'NONE',  ( 0.000000000000000000, -0.000000000000000000, 1.000000000000000000 ) ) ;
#102603 = VECTOR ( 'NONE', #28297, 1000.000000000000000 ) ;
#102604 = DIRECTION ( 'NONE',  ( -0.000000000000000000, -1.000000000000000000, -0.000000000000000000 ) ) ;
#102605 = VERTEX_POINT ( 'NONE', #80484 ) ;
#102606 = LINE ( 'NONE', #84253, #121326 ) ;
#102607 = DIRECTION ( 'NONE',  ( -0.000000000000000000, 1.000000000000000000, -0.000000000000000000 ) ) ;
#102608 = DIRECTION ( 'NONE',  ( 0.000000000000000000, 0.000000000000000000, 1.000000000000000000 ) ) ;
#102609 = DIRECTION ( 'NONE',  ( 0.000000000000000000, 1.000000000000000000, 0.000000000000000000 ) ) ;
#102610 = AXIS2_PLACEMENT_3D ( 'NONE', #67822, #29842, #27904 ) ;
#102611 = CARTESIAN_POINT ( 'NONE',  ( 4.149999999999938183, 2.500000000000000000, 5.702370205355745014 ) ) ;
#102612 = ORIENTED_EDGE ( 'NONE', *, *, #35367, .T. ) ;
#102613 = CARTESIAN_POINT ( 'NONE',  ( 5.199999999999933564, 2.500000000000000000, 3.883716857408420431 ) ) ;
#102614 = CARTESIAN_POINT ( 'NONE',  ( 48.67919755208251331, -3.179368040553702812, 5.083101272021607997 ) ) ;
#102615 = ORIENTED_EDGE ( 'NONE', *, *, #42855, .F. ) ;
#102616 = ORIENTED_EDGE ( 'NONE', *, *, #79472, .T. ) ;
#102617 = ADVANCED_FACE ( 'NONE', ( #128943 ), #129589, .T. ) ;
#102618 = CARTESIAN_POINT ( 'NONE',  ( 184.4427083336747160, -6.551208109652278289, 3.782341765624995134 ) ) ;
#102619 = DIRECTION ( 'NONE',  ( -0.000000000000000000, 1.000000000000000000, -0.000000000000000000 ) ) ;
#102620 = CARTESIAN_POINT ( 'NONE',  ( 12.89999999999989733, 2.500000000000000000, -2.385244779468109755E-15 ) ) ;
#102621 = DIRECTION ( 'NONE',  ( 0.000000000000000000, 0.000000000000000000, 1.000000000000000000 ) ) ;
#102622 = CARTESIAN_POINT ( 'NONE',  ( -10.65000000000000213, 2.500000000000000000, 6.148780366869520009 ) ) ;
#102623 = AXIS2_PLACEMENT_3D ( 'NONE', #115785, #26128, #66039 ) ;
#102624 = CARTESIAN_POINT ( 'NONE',  ( 11.84999999999990727, 2.500000000000000000, 6.741600689897071952 ) ) ;
#102625 = DIRECTION ( 'NONE',  ( 0.000000000000000000, 0.000000000000000000, -1.000000000000000000 ) ) ;
#102626 = DIRECTION ( 'NONE',  ( 0.000000000000000000, -0.9999939076577903929, 0.003490651415223739937 ) ) ;
#102627 = EDGE_CURVE ( 'NONE', #108936, #107284, #88321, .T. ) ;
#102628 = ADVANCED_FACE ( 'NONE', ( #71276 ), #119729, .T. ) ;
#102629 = CARTESIAN_POINT ( 'NONE',  ( -8.150000000000014566, 12.50000000000000000, -6.083687093685483660 ) ) ;
#102630 = AXIS2_PLACEMENT_3D ( 'NONE', #68028, #117753, #39249 ) ;
#102631 = ORIENTED_EDGE ( 'NONE', *, *, #4619, .T. ) ;
#102633 = ORIENTED_EDGE ( 'NONE', *, *, #50269, .F. ) ;
#102632 = AXIS2_PLACEMENT_3D ( 'NONE', #2305, #13422, #83481 ) ;
#102634 = EDGE_CURVE ( 'NONE', #115112, #82663, #113254, .T. ) ;
#102635 = ORIENTED_EDGE ( 'NONE', *, *, #91982, .F. ) ;
#102636 = EDGE_LOOP ( 'NONE', ( #77976, #56934, #91, #77698 ) ) ;
#102637 = ADVANCED_FACE ( 'NONE', ( #9783 ), #50548, .T. ) ;
#102638 = CARTESIAN_POINT ( 'NONE',  ( 12.49999999999990230, 2.500000000000000000, -0.6928203230275541413 ) ) ;
#102639 = CARTESIAN_POINT ( 'NONE',  ( 4.599999999999940137, 2.500000000000000000, -4.922947341949753586 ) ) ;
#102640 = CONICAL_SURFACE ( 'NONE', #6466, 0.1000000000000000472, 0.003490658503988666988 ) ;
#102641 = EDGE_CURVE ( 'NONE', #30880, #62242, #30742, .T. ) ;
#102642 = CIRCLE ( 'NONE', #21172, 0.09999999999999982514 ) ;
#102643 = EDGE_LOOP ( 'NONE', ( #55982, #489, #9127, #78668 ) ) ;
#102644 = EDGE_CURVE ( 'NONE', #10609, #116681, #20898, .T. ) ;
#102645 = DIRECTION ( 'NONE',  ( 0.000000000000000000, 0.000000000000000000, 1.000000000000000000 ) ) ;
#102646 = ADVANCED_FACE ( 'NONE', ( #124259 ), #43144, .T. ) ;
#102647 = FACE_OUTER_BOUND ( 'NONE', #114196, .T. ) ;
#102649 = EDGE_LOOP ( 'NONE', ( #78437, #37391, #123778, #23850 ) ) ;
#102648 = CARTESIAN_POINT ( 'NONE',  ( 2.499999999999948930, 2.500000000000000000, -5.022947341949754119 ) ) ;
#102650 = CARTESIAN_POINT ( 'NONE',  ( -12.04999999999999716, 2.500000000000000000, -2.065063509461098068 ) ) ;
#102651 = ADVANCED_FACE ( 'NONE', ( #22855 ), #115283, .T. ) ;
#102652 = DIRECTION ( 'NONE',  ( -1.000000000000000000, -0.000000000000000000, -0.000000000000000000 ) ) ;
#102653 = VECTOR ( 'NONE', #67893, 1000.000000000000000 ) ;
#102654 = ORIENTED_EDGE ( 'NONE', *, *, #67633, .F. ) ;
#102655 = AXIS2_PLACEMENT_3D ( 'NONE', #97856, #18654, #59901 ) ;
#102656 = EDGE_LOOP ( 'NONE', ( #55999, #88841 ) ) ;
#102657 = ORIENTED_EDGE ( 'NONE', *, *, #124902, .F. ) ;
#102658 = ORIENTED_EDGE ( 'NONE', *, *, #43777, .T. ) ;
#102659 = CARTESIAN_POINT ( 'NONE',  ( -14.79999999999998295, 12.50000000000000000, -0.4115034346978134749 ) ) ;
#102660 = DIRECTION ( 'NONE',  ( -0.000000000000000000, 1.000000000000000000, -0.000000000000000000 ) ) ;
#102661 = DIRECTION ( 'NONE',  ( 0.000000000000000000, 0.000000000000000000, -1.000000000000000000 ) ) ;
#102662 = DIRECTION ( 'NONE',  ( 0.000000000000000000, 0.000000000000000000, -1.000000000000000000 ) ) ;
#102663 = ORIENTED_EDGE ( 'NONE', *, *, #119492, .T. ) ;
#102664 = AXIS2_PLACEMENT_3D ( 'NONE', #69060, #108967, #19308 ) ;
#102665 = AXIS2_PLACEMENT_3D ( 'NONE', #65249, #105188, #15510 ) ;
#102666 = CARTESIAN_POINT ( 'NONE',  ( -7.499999999999980460, 12.50000000000000000, -2.276824562219559311E-15 ) ) ;
#102667 = ORIENTED_EDGE ( 'NONE', *, *, #49910, .T. ) ;
#102668 = CARTESIAN_POINT ( 'NONE',  ( 3.099999999999943245, 2.500000000000000000, 4.083716857408420609 ) ) ;
#102669 = CARTESIAN_POINT ( 'NONE',  ( -1.700000000000034817, 2.500000000000000000, -4.330127018922201643 ) ) ;
#102670 = DIRECTION ( 'NONE',  ( 0.000000000000000000, 0.000000000000000000, -1.000000000000000000 ) ) ;
#102671 = CARTESIAN_POINT ( 'NONE',  ( 9.799999999999913669, 12.50000000000000000, -3.918623584224389056 ) ) ;
#102672 = EDGE_LOOP ( 'NONE', ( #51898, #76836, #27141, #84792 ) ) ;
#102673 = VERTEX_POINT ( 'NONE', #51663 ) ;
#102674 = EDGE_LOOP ( 'NONE', ( #4498, #108545 ) ) ;
#102675 = DIRECTION ( 'NONE',  ( -0.000000000000000000, 1.000000000000000000, -0.000000000000000000 ) ) ;
#102676 = DIRECTION ( 'NONE',  ( 0.000000000000000000, -0.9999939076577903929, 0.003490651415223739937 ) ) ;
#102677 = CARTESIAN_POINT ( 'NONE',  ( 3.349999999999941913, 2.500000000000000000, 5.902370205355745192 ) ) ;
#102678 = FACE_BOUND ( 'NONE', #67692, .T. ) ;
#102679 = DIRECTION ( 'NONE',  ( 0.000000000000000000, 0.000000000000000000, 1.000000000000000000 ) ) ;
#102680 = CARTESIAN_POINT ( 'NONE',  ( -13.74999999999998934, 2.500000000000000000, 2.957883832488652942 ) ) ;
#102681 = CARTESIAN_POINT ( 'NONE',  ( -4.350000000000027178, 12.50000000000000000, -6.148780366869526226 ) ) ;
#102682 = EDGE_CURVE ( 'NONE', #47303, #116756, #113796, .T. ) ;
#102683 = AXIS2_PLACEMENT_3D ( 'NONE', #35340, #25492, #65426 ) ;
#102684 = AXIS2_PLACEMENT_3D ( 'NONE', #108102, #117919, #18438 ) ;
#102686 = VECTOR ( 'NONE', #93279, 1000.000000000000000 ) ;
#102685 = DIRECTION ( 'NONE',  ( 0.000000000000000000, 1.000000000000000000, 0.000000000000000000 ) ) ;
#102687 = CARTESIAN_POINT ( 'NONE',  ( 0.000000000000000000, 0.000000000000000000, -5.000000000000004441 ) ) ;
#102688 = CARTESIAN_POINT ( 'NONE',  ( 3.299999999999942979, 2.500000000000000000, 4.430127018922196847 ) ) ;
#102689 = ORIENTED_EDGE ( 'NONE', *, *, #57739, .T. ) ;
#102690 = DIRECTION ( 'NONE',  ( 0.000000000000000000, 0.000000000000000000, 1.000000000000000000 ) ) ;
#102691 = AXIS2_PLACEMENT_3D ( 'NONE', #68452, #29836, #69753 ) ;
#102692 = ORIENTED_EDGE ( 'NONE', *, *, #49902, .T. ) ;
#102693 = EDGE_LOOP ( 'NONE', ( #90439, #82746 ) ) ;
#102694 = CONICAL_SURFACE ( 'NONE', #46267, 0.09999999999999982514, 0.003490658503988666988 ) ;
#102695 = DIRECTION ( 'NONE',  ( -0.000000000000000000, 1.000000000000000000, -0.000000000000000000 ) ) ;
#102696 = EDGE_CURVE ( 'NONE', #55696, #49092, #44404, .T. ) ;
#102697 = DIRECTION ( 'NONE',  ( -0.000000000000000000, -1.000000000000000000, -0.000000000000000000 ) ) ;
#102698 = FACE_BOUND ( 'NONE', #79515, .T. ) ;
#102699 = CARTESIAN_POINT ( 'NONE',  ( 11.64999999999990798, 2.500000000000000000, 5.702370205355745014 ) ) ;
#102700 = EDGE_LOOP ( 'NONE', ( #76905, #41617 ) ) ;
#102701 = LINE ( 'NONE', #637, #6886 ) ;
#102702 = CARTESIAN_POINT ( 'NONE',  ( -9.150000000000009237, 2.500000000000000000, 1.372243186433545370 ) ) ;
#102703 = ORIENTED_EDGE ( 'NONE', *, *, #90955, .F. ) ;
#102704 = DIRECTION ( 'NONE',  ( 0.000000000000000000, 0.000000000000000000, 1.000000000000000000 ) ) ;
#102705 = DIRECTION ( 'NONE',  ( 0.000000000000000000, 0.000000000000000000, 1.000000000000000000 ) ) ;
#102706 = ORIENTED_EDGE ( 'NONE', *, *, #53473, .T. ) ;
#102707 = CARTESIAN_POINT ( 'NONE',  ( -0.6500000000000389910, 2.500000000000000000, -1.918653347947326004 ) ) ;
#102708 = LINE ( 'NONE', #111235, #59424 ) ;
#102709 = CIRCLE ( 'NONE', #77676, 0.06509327318403745899 ) ;
#102710 = AXIS2_PLACEMENT_3D ( 'NONE', #103607, #121303, #23104 ) ;
#102711 = ORIENTED_EDGE ( 'NONE', *, *, #24430, .F. ) ;
#102712 = ADVANCED_FACE ( 'NONE', ( #73225 ), #106979, .T. ) ;
#102713 = DIRECTION ( 'NONE',  ( 0.000000000000000000, 1.000000000000000000, 0.000000000000000000 ) ) ;
#102714 = DIRECTION ( 'NONE',  ( 0.000000000000000000, 0.000000000000000000, -1.000000000000000000 ) ) ;
#102715 = LINE ( 'NONE', #53637, #53479 ) ;
#102716 = ORIENTED_EDGE ( 'NONE', *, *, #110636, .F. ) ;
#102717 = ORIENTED_EDGE ( 'NONE', *, *, #45706, .T. ) ;
#102718 = CYLINDRICAL_SURFACE ( 'NONE', #5433, 5.200000000000000178 ) ;
#102719 = AXIS2_PLACEMENT_3D ( 'NONE', #1259, #62125, #52297 ) ;
#102720 = EDGE_CURVE ( 'NONE', #86983, #74378, #53591, .T. ) ;
#102721 = ORIENTED_EDGE ( 'NONE', *, *, #39790, .F. ) ;
#102722 = DIRECTION ( 'NONE',  ( -0.000000000000000000, -1.000000000000000000, -0.000000000000000000 ) ) ;
#102723 = AXIS2_PLACEMENT_3D ( 'NONE', #71371, #83786, #123689 ) ;
#102724 = CARTESIAN_POINT ( 'NONE',  ( 107.5000000000000142, -1.500000000000000222, -1.322875655532295136 ) ) ;
#102725 = ORIENTED_EDGE ( 'NONE', *, *, #57511, .T. ) ;
#102726 = AXIS2_PLACEMENT_3D ( 'NONE', #48899, #37775, #18120 ) ;
#102727 = CARTESIAN_POINT ( 'NONE',  ( -6.900000000000019007, 12.50000000000000000, -0.3464101615137783474 ) ) ;
#102728 = DIRECTION ( 'NONE',  ( 0.000000000000000000, -0.9999939076577903929, 0.003490651415223739937 ) ) ;
#102729 = CARTESIAN_POINT ( 'NONE',  ( 165.4999999999999716, 6.123233995736768501E-17, -1.500000000000000000 ) ) ;
#102730 = EDGE_CURVE ( 'NONE', #20150, #113637, #32682, .T. ) ;
#102731 = EDGE_CURVE ( 'NONE', #119576, #56267, #61486, .T. ) ;
#102732 = CARTESIAN_POINT ( 'NONE',  ( -11.89999999999999680, 12.50000000000000000, -0.4115034346978116431 ) ) ;
#102733 = ADVANCED_FACE ( 'NONE', ( #122971 ), #8676, .T. ) ;
#102734 = EDGE_CURVE ( 'NONE', #129244, #128672, #63403, .T. ) ;
#102735 = EDGE_CURVE ( 'NONE', #87361, #69532, #100629, .T. ) ;
#102736 = DIRECTION ( 'NONE',  ( -0.000000000000000000, 1.000000000000000000, -0.000000000000000000 ) ) ;
#102737 = AXIS2_PLACEMENT_3D ( 'NONE', #14275, #14896, #6365 ) ;
#102738 = ORIENTED_EDGE ( 'NONE', *, *, #56602, .F. ) ;
#102739 = VECTOR ( 'NONE', #7538, 1000.000000000000000 ) ;
#102740 = ORIENTED_EDGE ( 'NONE', *, *, #60573, .F. ) ;
#102741 = FACE_OUTER_BOUND ( 'NONE', #606, .T. ) ;
#102742 = ORIENTED_EDGE ( 'NONE', *, *, #97187, .F. ) ;
#102743 = CARTESIAN_POINT ( 'NONE',  ( 103.5236730166301697, 7.370027598015842507, -2.251927279840987506 ) ) ;
#102744 = CONICAL_SURFACE ( 'NONE', #23322, 0.1000000000000002554, 0.003490658503988666988 ) ;
#102746 = ORIENTED_EDGE ( 'NONE', *, *, #74408, .F. ) ;
#102745 = ORIENTED_EDGE ( 'NONE', *, *, #86352, .F. ) ;
#102747 = ORIENTED_EDGE ( 'NONE', *, *, #40293, .F. ) ;
#102748 = ADVANCED_FACE ( 'NONE', ( #1893 ), #19141, .T. ) ;
#102749 = CARTESIAN_POINT ( 'NONE',  ( 0.6499999999999566125, 2.500000000000000000, -6.841600689897077814 ) ) ;
#102750 = AXIS2_PLACEMENT_3D ( 'NONE', #21902, #70340, #101739 ) ;
#102751 = EDGE_CURVE ( 'NONE', #95146, #17807, #103975, .T. ) ;
#102752 = CARTESIAN_POINT ( 'NONE',  ( -12.49999999999995737, 12.50000000000000000, 4.330127018922196314 ) ) ;
#102753 = ADVANCED_FACE ( 'NONE', ( #24126 ), #88095, .T. ) ;
#102754 = CARTESIAN_POINT ( 'NONE',  ( -7.100000000000018296, 12.50000000000000000, -4.330127018922201643 ) ) ;
#102755 = CARTESIAN_POINT ( 'NONE',  ( -5.400000000000024336, 2.500000000000000000, -3.637306695894650055 ) ) ;
#102756 = VECTOR ( 'NONE', #1670, 1000.000000000000000 ) ;
#102757 = DIRECTION ( 'NONE',  ( 0.000000000000000000, 0.000000000000000000, 1.000000000000000000 ) ) ;
#102758 = DIRECTION ( 'NONE',  ( 0.000000000000000000, 1.000000000000000000, 0.000000000000000000 ) ) ;
#102759 = DIRECTION ( 'NONE',  ( 0.000000000000000000, -0.000000000000000000, 1.000000000000000000 ) ) ;
#102760 = DIRECTION ( 'NONE',  ( 0.000000000000000000, 0.000000000000000000, -1.000000000000000000 ) ) ;
#102761 = CARTESIAN_POINT ( 'NONE',  ( -11.84999999999999609, 12.50000000000000000, 1.753560074763284016 ) ) ;
#102762 = VERTEX_POINT ( 'NONE', #84324 ) ;
#102763 = DIRECTION ( 'NONE',  ( 0.000000000000000000, 0.000000000000000000, -1.000000000000000000 ) ) ;
#102764 = ORIENTED_EDGE ( 'NONE', *, *, #77296, .T. ) ;
#102765 = ORIENTED_EDGE ( 'NONE', *, *, #91527, .F. ) ;
#102766 = CARTESIAN_POINT ( 'NONE',  ( -2.050000000000033129, 2.500000000000000000, 6.595190528383296780 ) ) ;
#102767 = CARTESIAN_POINT ( 'NONE',  ( 11.04999999999990656, 2.500000000000000000, 2.411473670974873862 ) ) ;
#102768 = CARTESIAN_POINT ( 'NONE',  ( -7.300000000000016698, 12.50000000000000000, -0.3464101615137783474 ) ) ;
#102769 = FACE_OUTER_BOUND ( 'NONE', #7924, .T. ) ;
#102770 = CARTESIAN_POINT ( 'NONE',  ( 12.29999999999990656, 2.500000000000000000, 3.983716857408420964 ) ) ;
#102771 = DIRECTION ( 'NONE',  ( 0.000000000000000000, 0.000000000000000000, 1.000000000000000000 ) ) ;
#102772 = DIRECTION ( 'NONE',  ( 0.000000000000000000, 0.000000000000000000, 1.000000000000000000 ) ) ;
#102773 = EDGE_LOOP ( 'NONE', ( #50608, #27249, #26006, #59666 ) ) ;
#102774 = VECTOR ( 'NONE', #1057, 1000.000000000000000 ) ;
#102775 = AXIS2_PLACEMENT_3D ( 'NONE', #11979, #70268, #31634 ) ;
#102776 = EDGE_LOOP ( 'NONE', ( #40458, #23780 ) ) ;
#102777 = CONICAL_SURFACE ( 'NONE', #27463, 0.09999999999999982514, 0.003490658503988666988 ) ;
#102778 = ORIENTED_EDGE ( 'NONE', *, *, #75489, .F. ) ;
#102779 = CONICAL_SURFACE ( 'NONE', #77733, 0.09999999999999999167, 0.003490658503988666988 ) ;
#102780 = ORIENTED_EDGE ( 'NONE', *, *, #14820, .F. ) ;
#102781 = CONICAL_SURFACE ( 'NONE', #48416, 0.1000000000000002554, 0.003490658503988666988 ) ;
#102782 = AXIS2_PLACEMENT_3D ( 'NONE', #23798, #2198, #121996 ) ;
#102783 = EDGE_CURVE ( 'NONE', #31905, #60176, #81851, .T. ) ;
#102784 = VERTEX_POINT ( 'NONE', #33945 ) ;
#102785 = DIRECTION ( 'NONE',  ( 0.000000000000000000, -0.9999939076577903929, 0.003490651415223739937 ) ) ;
#102786 = DIRECTION ( 'NONE',  ( -4.274815082592931898E-19, -0.9999939076577903929, -0.003490651415223739937 ) ) ;
#102787 = CIRCLE ( 'NONE', #17088, 7.699999999999999289 ) ;
#102788 = EDGE_CURVE ( 'NONE', #127817, #120673, #98566, .T. ) ;
#102789 = LINE ( 'NONE', #3954, #69633 ) ;
#102790 = DIRECTION ( 'NONE',  ( 0.000000000000000000, 0.000000000000000000, 1.000000000000000000 ) ) ;
#102791 = EDGE_CURVE ( 'NONE', #127159, #104514, #83912, .T. ) ;
#102792 = LINE ( 'NONE', #84461, #86893 ) ;
#102793 = ORIENTED_EDGE ( 'NONE', *, *, #95531, .F. ) ;
#102794 = CARTESIAN_POINT ( 'NONE',  ( 21.24754738303277080, -0.7337760880902354232, 4.182111650399362723 ) ) ;
#102795 = CARTESIAN_POINT ( 'NONE',  ( 1.649999999999949729, 2.500000000000000000, 5.902370205355745192 ) ) ;
#102796 = DIRECTION ( 'NONE',  ( 0.000000000000000000, 0.000000000000000000, 1.000000000000000000 ) ) ;
#102797 = ADVANCED_FACE ( 'NONE', ( #72586 ), #27318, .T. ) ;
#102798 = DIRECTION ( 'NONE',  ( 0.000000000000000000, 1.000000000000000000, 0.000000000000000000 ) ) ;
#102799 = ORIENTED_EDGE ( 'NONE', *, *, #28127, .T. ) ;
#102800 = VERTEX_POINT ( 'NONE', #105253 ) ;
#102801 = VERTEX_POINT ( 'NONE', #66612 ) ;
#102802 = DIRECTION ( 'NONE',  ( 0.000000000000000000, 0.000000000000000000, -1.000000000000000000 ) ) ;
#102803 = EDGE_CURVE ( 'NONE', #93446, #69877, #96709, .T. ) ;
#102804 = DIRECTION ( 'NONE',  ( -4.274815082592931898E-19, -0.9999939076577903929, -0.003490651415223739937 ) ) ;
#102805 = VECTOR ( 'NONE', #54040, 1000.000000000000000 ) ;
#102806 = LINE ( 'NONE', #43281, #106673 ) ;
#102807 = AXIS2_PLACEMENT_3D ( 'NONE', #2164, #92482, #44039 ) ;
#102808 = ORIENTED_EDGE ( 'NONE', *, *, #64687, .T. ) ;
#102809 = CARTESIAN_POINT ( 'NONE',  ( 14.14999999999989200, 2.500000000000000000, -2.065063509461102065 ) ) ;
#102810 = DIRECTION ( 'NONE',  ( 0.000000000000000000, 0.000000000000000000, -1.000000000000000000 ) ) ;
#102811 = DIRECTION ( 'NONE',  ( 0.000000000000000000, 0.000000000000000000, -1.000000000000000000 ) ) ;
#102812 = EDGE_CURVE ( 'NONE', #5452, #64674, #29631, .T. ) ;
#102813 = DIRECTION ( 'NONE',  ( -0.000000000000000000, 1.000000000000000000, -0.000000000000000000 ) ) ;
#102814 = CIRCLE ( 'NONE', #113287, 0.06509327318403745899 ) ;
#102815 = VECTOR ( 'NONE', #15333, 1000.000000000000000 ) ;
#102816 = VECTOR ( 'NONE', #66246, 1000.000000000000000 ) ;
#102817 = CARTESIAN_POINT ( 'NONE',  ( 5.399999999999935518, 2.500000000000000000, -4.330127018922201643 ) ) ;
#102818 = ORIENTED_EDGE ( 'NONE', *, *, #119379, .F. ) ;
#102819 = ORIENTED_EDGE ( 'NONE', *, *, #15628, .T. ) ;
#102820 = DIRECTION ( 'NONE',  ( 0.000000000000000000, 0.000000000000000000, 1.000000000000000000 ) ) ;
#102821 = CARTESIAN_POINT ( 'NONE',  ( -9.600000000000006750, 12.50000000000000000, 3.637306695894644726 ) ) ;
#102822 = DIRECTION ( 'NONE',  ( 0.000000000000000000, 0.000000000000000000, -1.000000000000000000 ) ) ;
#102823 = AXIS2_PLACEMENT_3D ( 'NONE', #68381, #9473, #27173 ) ;
#102825 = DIRECTION ( 'NONE',  ( 0.000000000000000000, 0.000000000000000000, 1.000000000000000000 ) ) ;
#102824 = AXIS2_PLACEMENT_3D ( 'NONE', #91268, #122023, #71624 ) ;
#102826 = ORIENTED_EDGE ( 'NONE', *, *, #59533, .F. ) ;
#102827 = ADVANCED_FACE ( 'NONE', ( #6374 ), #102777, .T. ) ;
#102828 = AXIS2_PLACEMENT_3D ( 'NONE', #127816, #21081, #20450 ) ;
#102829 = AXIS2_PLACEMENT_3D ( 'NONE', #56403, #128401, #116611 ) ;
#102830 = CIRCLE ( 'NONE', #88151, 0.06509327318403745899 ) ;
#102831 = ORIENTED_EDGE ( 'NONE', *, *, #128228, .T. ) ;
#102832 = FACE_OUTER_BOUND ( 'NONE', #41746, .T. ) ;
#102833 = CARTESIAN_POINT ( 'NONE',  ( 3.349999999999941913, 2.500000000000000000, 6.595190528383296780 ) ) ;
#102834 = CIRCLE ( 'NONE', #117486, 0.06509327318403741736 ) ;
#102835 = DIRECTION ( 'NONE',  ( -0.000000000000000000, 1.000000000000000000, -0.000000000000000000 ) ) ;
#102836 = DIRECTION ( 'NONE',  ( 0.000000000000000000, 0.000000000000000000, 1.000000000000000000 ) ) ;
#102837 = ORIENTED_EDGE ( 'NONE', *, *, #54823, .T. ) ;
#102838 = CARTESIAN_POINT ( 'NONE',  ( -10.65000000000000391, 2.500000000000000000, -2.511473670974873951 ) ) ;
#102839 = CARTESIAN_POINT ( 'NONE',  ( 3.299999999999944755, 2.500000000000000000, 0.09999999999999761857 ) ) ;
#102840 = CIRCLE ( 'NONE', #63148, 0.06509327318403745899 ) ;
#102841 = EDGE_LOOP ( 'NONE', ( #23206, #66200 ) ) ;
#102842 = DIRECTION ( 'NONE',  ( -0.000000000000000000, 1.000000000000000000, -0.000000000000000000 ) ) ;
#102843 = EDGE_CURVE ( 'NONE', #48868, #90822, #119511, .T. ) ;
#102844 = VERTEX_POINT ( 'NONE', #77088 ) ;
#102845 = B_SPLINE_CURVE_WITH_KNOTS ( 'NONE', 3,
 ( #82034, #71575, #72874, #121977, #82708, #112157 ),
 .UNSPECIFIED., .F., .F.,
 ( 4, 2, 4 ),
 ( 0.000000000000000000, 0.5000000000000000000, 1.000000000000000000 ),
 .UNSPECIFIED. ) ;
#102846 = DIRECTION ( 'NONE',  ( 0.000000000000000000, 0.000000000000000000, 1.000000000000000000 ) ) ;
#102847 = VERTEX_POINT ( 'NONE', #116987 ) ;
#102848 = DIRECTION ( 'NONE',  ( 0.000000000000000000, 1.000000000000000000, 0.000000000000000000 ) ) ;
#102849 = LINE ( 'NONE', #13174, #25102 ) ;
#102850 = VERTEX_POINT ( 'NONE', #87538 ) ;
#102851 = ADVANCED_FACE ( 'NONE', ( #55520 ), #58981, .T. ) ;
#102852 = ORIENTED_EDGE ( 'NONE', *, *, #21665, .T. ) ;
#102853 = CARTESIAN_POINT ( 'NONE',  ( 186.6718750003414016, 9.264065473108010111E-16, -7.564683531250000925 ) ) ;
#102854 = DIRECTION ( 'NONE',  ( -0.000000000000000000, 1.000000000000000000, -0.000000000000000000 ) ) ;
#102855 = CARTESIAN_POINT ( 'NONE',  ( 186.5468750003414300, -8.734944146203032389, -1.604583208406767949E-15 ) ) ;
#102856 = PLANE ( 'NONE',  #30449 ) ;
#102857 = CARTESIAN_POINT ( 'NONE',  ( 4.999999999999938716, 12.50000000000000000, -5.022947341949754119 ) ) ;
#102858 = CARTESIAN_POINT ( 'NONE',  ( -4.150000000000024336, 2.500000000000000000, -2.265063509461101798 ) ) ;
#102859 = DIRECTION ( 'NONE',  ( 0.000000000000000000, 0.000000000000000000, -1.000000000000000000 ) ) ;
#102860 = VECTOR ( 'NONE', #118515, 1000.000000000000000 ) ;
#102861 = CONICAL_SURFACE ( 'NONE', #42254, 0.1000000000000002554, 0.003490658503988666988 ) ;
#102862 = DIRECTION ( 'NONE',  ( -4.274815082592931898E-19, -0.9999939076577903929, -0.003490651415223739937 ) ) ;
#102863 = LINE ( 'NONE', #3389, #12852 ) ;
#102864 = CIRCLE ( 'NONE', #73627, 0.09999999999999982514 ) ;
#102865 = VERTEX_POINT ( 'NONE', #16837 ) ;
#102868 = VERTEX_POINT ( 'NONE', #57449 ) ;
#102867 = ADVANCED_FACE ( 'NONE', ( #5742 ), #107075, .T. ) ;
#102866 = AXIS2_PLACEMENT_3D ( 'NONE', #22925, #33400, #62215 ) ;
#102869 = DIRECTION ( 'NONE',  ( -0.000000000000000000, 1.000000000000000000, -0.000000000000000000 ) ) ;
#102870 = ORIENTED_EDGE ( 'NONE', *, *, #86744, .T. ) ;
#102871 = CARTESIAN_POINT ( 'NONE',  ( 0.3999999999999628852, 2.500000000000000000, 0.5928203230275517210 ) ) ;
#102872 = CARTESIAN_POINT ( 'NONE',  ( 4.349999999999938360, 2.500000000000000000, 1.918653347947321564 ) ) ;
#102873 = AXIS2_PLACEMENT_3D ( 'NONE', #56534, #96451, #46731 ) ;
#102874 = DIRECTION ( 'NONE',  ( -0.000000000000000000, 1.000000000000000000, -0.000000000000000000 ) ) ;
#102877 = VERTEX_POINT ( 'NONE', #45704 ) ;
#102876 = ORIENTED_EDGE ( 'NONE', *, *, #26912, .T. ) ;
#102875 = AXIS2_PLACEMENT_3D ( 'NONE', #100041, #18885, #99402 ) ;
#102878 = FACE_BOUND ( 'NONE', #23143, .T. ) ;
#102879 = ORIENTED_EDGE ( 'NONE', *, *, #5676, .T. ) ;
#102880 = FACE_OUTER_BOUND ( 'NONE', #41115, .T. ) ;
#102881 = DIRECTION ( 'NONE',  ( -0.000000000000000000, -1.000000000000000000, -0.000000000000000000 ) ) ;
#102882 = AXIS2_PLACEMENT_3D ( 'NONE', #5068, #96034, #116303 ) ;
#102884 = ADVANCED_FACE ( 'NONE', ( #97367 ), #65214, .T. ) ;
#102883 = DIRECTION ( 'NONE',  ( 0.000000000000000000, 0.000000000000000000, -1.000000000000000000 ) ) ;
#102885 = DIRECTION ( 'NONE',  ( -0.000000000000000000, 1.000000000000000000, -0.000000000000000000 ) ) ;
#102886 = CARTESIAN_POINT ( 'NONE',  ( 184.4895833340161460, -4.445597072760175017, -7.699999999999898037 ) ) ;
#102887 = DIRECTION ( 'NONE',  ( -0.000000000000000000, -1.000000000000000000, -0.000000000000000000 ) ) ;
#102888 = CARTESIAN_POINT ( 'NONE',  ( -3.749999999999991562, 12.50000000000000000, 6.560283801567334372 ) ) ;
#102889 = CARTESIAN_POINT ( 'NONE',  ( -0.6500000000000398792, 2.500000000000000000, -2.511473670974877948 ) ) ;
#102890 = ADVANCED_FACE ( 'NONE', ( #56143 ), #15026, .T. ) ;
#102891 = ADVANCED_FACE ( 'NONE', ( #126833 ), #61019, .T. ) ;
#102892 = DIRECTION ( 'NONE',  ( -0.000000000000000000, -1.000000000000000000, -0.000000000000000000 ) ) ;
#102893 = DIRECTION ( 'NONE',  ( -4.274815082592931898E-19, -0.9999939076577903929, -0.003490651415223739937 ) ) ;
#102894 = ADVANCED_FACE ( 'NONE', ( #36536 ), #84966, .T. ) ;
#102895 = EDGE_CURVE ( 'NONE', #44517, #22601, #4558, .T. ) ;
#102896 = DIRECTION ( 'NONE',  ( -0.000000000000000000, -1.000000000000000000, -0.000000000000000000 ) ) ;
#102897 = ORIENTED_EDGE ( 'NONE', *, *, #38518, .F. ) ;
#102898 = VERTEX_POINT ( 'NONE', #65316 ) ;
#102899 = ORIENTED_EDGE ( 'NONE', *, *, #51542, .T. ) ;
#102900 = DIRECTION ( 'NONE',  ( -0.000000000000000000, -1.000000000000000000, -0.000000000000000000 ) ) ;
#102901 = ORIENTED_EDGE ( 'NONE', *, *, #129538, .T. ) ;
#102902 = EDGE_CURVE ( 'NONE', #100484, #72434, #86897, .T. ) ;
#102903 = FACE_OUTER_BOUND ( 'NONE', #26175, .T. ) ;
#102906 = EDGE_LOOP ( 'NONE', ( #5902, #93405 ) ) ;
#102905 = ORIENTED_EDGE ( 'NONE', *, *, #97709, .T. ) ;
#102904 = EDGE_CURVE ( 'NONE', #41615, #125433, #115708, .T. ) ;
#102907 = ORIENTED_EDGE ( 'NONE', *, *, #5228, .F. ) ;
#102908 = ADVANCED_FACE ( 'NONE', ( #65975 ), #48512, .T. ) ;
#102909 = DIRECTION ( 'NONE',  ( -0.000000000000000000, -1.000000000000000000, -0.000000000000000000 ) ) ;
#102910 = CIRCLE ( 'NONE', #42378, 0.06509327318403741736 ) ;
#102911 = ADVANCED_FACE ( 'NONE', ( #69177 ), #29727, .T. ) ;
#102912 = EDGE_CURVE ( 'NONE', #108868, #38667, #102864, .T. ) ;
#102913 = DIRECTION ( 'NONE',  ( -0.000000000000000000, 1.000000000000000000, -0.000000000000000000 ) ) ;
#102914 = CARTESIAN_POINT ( 'NONE',  ( -11.04999999999999893, 12.50000000000000000, 6.213873640053558134 ) ) ;
#102915 = DIRECTION ( 'NONE',  ( 0.000000000000000000, 0.000000000000000000, 1.000000000000000000 ) ) ;
#102916 = DIRECTION ( 'NONE',  ( 0.000000000000000000, -0.000000000000000000, 1.000000000000000000 ) ) ;
#102917 = ORIENTED_EDGE ( 'NONE', *, *, #59039, .F. ) ;
#102919 = ADVANCED_FACE ( 'NONE', ( #102372 ), #112122, .T. ) ;
#102918 = VECTOR ( 'NONE', #93993, 1000.000000000000000 ) ;
#102920 = COLOUR_RGB ( '', 0.31764706, 0.68627451, 0.89019608) ;
#102921 = DIRECTION ( 'NONE',  ( 0.000000000000000000, -0.000000000000000000, 1.000000000000000000 ) ) ;
#102922 = EDGE_LOOP ( 'NONE', ( #21411, #18934, #50430, #101267 ) ) ;
#102923 = CIRCLE ( 'NONE', #25649, 0.09999999999999982514 ) ;
#102924 = ORIENTED_EDGE ( 'NONE', *, *, #77597, .T. ) ;
#102925 = CIRCLE ( 'NONE', #44437, 0.06509327318403745899 ) ;
#102926 = ORIENTED_EDGE ( 'NONE', *, *, #41608, .F. ) ;
#102927 = DIRECTION ( 'NONE',  ( 0.000000000000000000, 1.000000000000000000, 0.000000000000000000 ) ) ;
#102928 = SHAPE_REPRESENTATION ( 'BR-831', ( #12841, #83365, #58845, #94426, #38001, #2379, #6569, #75552, #79772 ), #90216 ) ;
#102929 = VERTEX_POINT ( 'NONE', #39124 ) ;
#102930 = ORIENTED_EDGE ( 'NONE', *, *, #64061, .F. ) ;
#102931 = EDGE_LOOP ( 'NONE', ( #70991, #35119 ) ) ;
#102932 = AXIS2_PLACEMENT_3D ( 'NONE', #23635, #60529, #93031 ) ;
#102933 = DIRECTION ( 'NONE',  ( 0.000000000000000000, -0.000000000000000000, 1.000000000000000000 ) ) ;
#102934 = AXIS2_PLACEMENT_3D ( 'NONE', #53130, #102848, #43320 ) ;
#102935 = CARTESIAN_POINT ( 'NONE',  ( -8.749999999999975131, 2.500000000000000000, 2.165063509461097713 ) ) ;
#102936 = CARTESIAN_POINT ( 'NONE',  ( 13.29999999999990301, 2.500000000000000000, -4.330127018922201643 ) ) ;
#102937 = CARTESIAN_POINT ( 'NONE',  ( 5.199999999999931788, 12.50000000000000000, 4.676537180435972552 ) ) ;
#102938 = AXIS2_PLACEMENT_3D ( 'NONE', #31463, #52382, #64129 ) ;
#102939 = DIRECTION ( 'NONE',  ( 0.000000000000000000, 0.000000000000000000, 1.000000000000000000 ) ) ;
#102940 = AXIS2_PLACEMENT_3D ( 'NONE', #58365, #88437, #38737 ) ;
#102941 = CIRCLE ( 'NONE', #109188, 0.09999999999999982514 ) ;
#102942 = CARTESIAN_POINT ( 'NONE',  ( -4.350000000000027178, 2.500000000000000000, -6.941600689897077459 ) ) ;
#102943 = VECTOR ( 'NONE', #13010, 1000.000000000000000 ) ;
#102944 = DIRECTION ( 'NONE',  ( 0.000000000000000000, 1.000000000000000000, 0.000000000000000000 ) ) ;
#102945 = ORIENTED_EDGE ( 'NONE', *, *, #128472, .T. ) ;
#102946 = PLANE ( 'NONE',  #121596 ) ;
#102947 = ORIENTED_EDGE ( 'NONE', *, *, #49919, .F. ) ;
#102948 = CARTESIAN_POINT ( 'NONE',  ( 4.399999999999939071, 12.50000000000000000, 0.4115034346978110880 ) ) ;
#102949 = VERTEX_POINT ( 'NONE', #22538 ) ;
#102950 = VERTEX_POINT ( 'NONE', #51988 ) ;
#102951 = CARTESIAN_POINT ( 'NONE',  ( 184.0677083336747160, -4.367472073101514418, -7.564683531250002702 ) ) ;
#102952 = ADVANCED_FACE ( 'NONE', ( #78390 ), #10910, .T. ) ;
#102953 = DIRECTION ( 'NONE',  ( 0.000000000000000000, 0.000000000000000000, 1.000000000000000000 ) ) ;
#102954 = EDGE_CURVE ( 'NONE', #1645, #124183, #2515, .T. ) ;
#102955 = VERTEX_POINT ( 'NONE', #77711 ) ;
#102956 = ORIENTED_EDGE ( 'NONE', *, *, #14254, .F. ) ;
#102957 = DIRECTION ( 'NONE',  ( -0.000000000000000000, 1.000000000000000000, -0.000000000000000000 ) ) ;
#102958 = DIRECTION ( 'NONE',  ( 0.000000000000000000, 1.000000000000000000, 0.000000000000000000 ) ) ;
#102959 = AXIS2_PLACEMENT_3D ( 'NONE', #32154, #81862, #52413 ) ;
#102960 = CARTESIAN_POINT ( 'NONE',  ( -5.000000000000026645, 12.50000000000000000, -3.572213422710612374 ) ) ;
#102961 = CARTESIAN_POINT ( 'NONE',  ( -11.24999999999996270, 2.500000000000000000, 6.495190528383297135 ) ) ;
#102962 = ADVANCED_FACE ( 'NONE', ( #108468 ), #54752, .T. ) ;
#102963 = LINE ( 'NONE', #113435, #68736 ) ;
#102964 = ORIENTED_EDGE ( 'NONE', *, *, #102904, .F. ) ;
#102965 = DIRECTION ( 'NONE',  ( 1.000000000000000000, -0.000000000000000000, -0.000000000000000000 ) ) ;
#102966 = CONICAL_SURFACE ( 'NONE', #61211, 0.1000000000000002554, 0.003490658503988666988 ) ;
#102967 = VECTOR ( 'NONE', #71338, 1000.000000000000000 ) ;
#102968 = AXIS2_PLACEMENT_3D ( 'NONE', #57566, #106650, #96822 ) ;
#102969 = ORIENTED_EDGE ( 'NONE', *, *, #12703, .T. ) ;
#102970 = DIRECTION ( 'NONE',  ( 0.000000000000000000, -0.000000000000000000, -1.000000000000000000 ) ) ;
#102971 = DIRECTION ( 'NONE',  ( 0.000000000000000000, 0.000000000000000000, -1.000000000000000000 ) ) ;
#102972 = CIRCLE ( 'NONE', #50754, 0.06509327318403745899 ) ;
#102973 = AXIS2_PLACEMENT_3D ( 'NONE', #14260, #122309, #43121 ) ;
#102974 = AXIS2_PLACEMENT_3D ( 'NONE', #5557, #36972, #65770 ) ;
#102975 = VECTOR ( 'NONE', #7110, 1000.000000000000000 ) ;
#102976 = VECTOR ( 'NONE', #19298, 1000.000000000000000 ) ;
#102977 = CARTESIAN_POINT ( 'NONE',  ( 185.2968750003414300, 8.734944146203032389, 5.348610694689227483E-16 ) ) ;
#102978 = DIRECTION ( 'NONE',  ( -0.000000000000000000, 1.000000000000000000, -0.000000000000000000 ) ) ;
#102979 = CARTESIAN_POINT ( 'NONE',  ( -7.100000000000017408, 12.50000000000000000, -5.022947341949754119 ) ) ;
#102980 = DIRECTION ( 'NONE',  ( 0.000000000000000000, 0.000000000000000000, -1.000000000000000000 ) ) ;
#102981 = CARTESIAN_POINT ( 'NONE',  ( 195.0000000000000000, 0.000000000000000000, 0.000000000000000000 ) ) ;
#102982 = ORIENTED_EDGE ( 'NONE', *, *, #80140, .F. ) ;
#102983 = DIRECTION ( 'NONE',  ( 0.000000000000000000, 1.000000000000000000, 0.000000000000000000 ) ) ;
#102984 = FACE_OUTER_BOUND ( 'NONE', #6781, .T. ) ;
#102985 = DIRECTION ( 'NONE',  ( 0.000000000000000000, 0.000000000000000000, 1.000000000000000000 ) ) ;
#102986 = ORIENTED_EDGE ( 'NONE', *, *, #75973, .F. ) ;
#102987 = CARTESIAN_POINT ( 'NONE',  ( -7.300000000000016698, 12.50000000000000000, -4.676537180435978769 ) ) ;
#102988 = AXIS2_PLACEMENT_3D ( 'NONE', #15241, #62455, #13965 ) ;
#102989 = EDGE_CURVE ( 'NONE', #46118, #54643, #71479, .T. ) ;
#102990 = EDGE_LOOP ( 'NONE', ( #52277, #82824, #53900, #65069 ) ) ;
#102991 = EDGE_LOOP ( 'NONE', ( #31514, #8411, #9467, #25626 ) ) ;
#102992 = DIRECTION ( 'NONE',  ( -0.000000000000000000, -1.000000000000000000, -0.000000000000000000 ) ) ;
#102993 = EDGE_LOOP ( 'NONE', ( #85796, #32322 ) ) ;
#102994 = CARTESIAN_POINT ( 'NONE',  ( 16.09541403887941158, -2.463474929527615487, -3.723514363715260789 ) ) ;
#102995 = CARTESIAN_POINT ( 'NONE',  ( 11.44999999999990870, 2.500000000000000000, -1.818653347947326138 ) ) ;
#102996 = DIRECTION ( 'NONE',  ( 0.000000000000000000, 0.000000000000000000, -1.000000000000000000 ) ) ;
#102997 = CIRCLE ( 'NONE', #107204, 0.1000000000000000056 ) ;
#102998 = ORIENTED_EDGE ( 'NONE', *, *, #120349, .T. ) ;
#102999 = AXIS2_PLACEMENT_3D ( 'NONE', #47498, #39637, #99825 ) ;
#103000 = CIRCLE ( 'NONE', #46565, 0.1000000000000000472 ) ;
#103001 = FACE_OUTER_BOUND ( 'NONE', #79637, .T. ) ;
#103002 = CARTESIAN_POINT ( 'NONE',  ( -5.650000000000023448, 2.500000000000000000, -1.718653347947326049 ) ) ;
#103003 = ADVANCED_FACE ( 'NONE', ( #64994 ), #33629, .T. ) ;
#103004 = EDGE_CURVE ( 'NONE', #92191, #74205, #4137, .T. ) ;
#103005 = AXIS2_PLACEMENT_3D ( 'NONE', #17004, #97533, #56950 ) ;
#103006 = ORIENTED_EDGE ( 'NONE', *, *, #79398, .F. ) ;
#103007 = AXIS2_PLACEMENT_3D ( 'NONE', #55768, #29389, #90206 ) ;
#103008 = AXIS2_PLACEMENT_3D ( 'NONE', #85824, #125739, #127063 ) ;
#103009 = ORIENTED_EDGE ( 'NONE', *, *, #19844, .F. ) ;
#103010 = VERTEX_POINT ( 'NONE', #63082 ) ;
#103011 = CARTESIAN_POINT ( 'NONE',  ( -6.050000000000018474, 12.50000000000000000, 6.841600689897072485 ) ) ;
#103012 = PLANE ( 'NONE',  #129514 ) ;
#103013 = CARTESIAN_POINT ( 'NONE',  ( 186.5000000000000000, 0.000000000000000000, 0.000000000000000000 ) ) ;
#103014 = ADVANCED_FACE ( 'NONE', ( #5437 ), #33934, .T. ) ;
#103015 = EDGE_LOOP ( 'NONE', ( #64844, #102027 ) ) ;
#103016 = DIRECTION ( 'NONE',  ( 0.000000000000000000, 0.000000000000000000, -1.000000000000000000 ) ) ;
#103017 = CARTESIAN_POINT ( 'NONE',  ( -1.650000000000034772, 12.50000000000000000, 1.472243186433545459 ) ) ;
#103018 = ORIENTED_EDGE ( 'NONE', *, *, #41068, .F. ) ;
#103019 = CONICAL_SURFACE ( 'NONE', #80047, 0.09999999999999982514, 0.003490658503988666988 ) ;
#103020 = CARTESIAN_POINT ( 'NONE',  ( 2.499999999999947153, 12.50000000000000000, 0.7579135962115869374 ) ) ;
#103021 = DIRECTION ( 'NONE',  ( 0.000000000000000000, 1.000000000000000000, 0.000000000000000000 ) ) ;
#103022 = AXIS2_PLACEMENT_3D ( 'NONE', #33255, #12291, #73162 ) ;
#103023 = AXIS2_PLACEMENT_3D ( 'NONE', #43853, #124327, #125593 ) ;
#103024 = DIRECTION ( 'NONE',  ( 0.000000000000000000, 1.000000000000000000, 0.000000000000000000 ) ) ;
#103025 = DIRECTION ( 'NONE',  ( -1.000000000000000000, -0.000000000000000000, -0.000000000000000000 ) ) ;
#103026 = LINE ( 'NONE', #121378, #117646 ) ;
#103027 = DIRECTION ( 'NONE',  ( -0.000000000000000000, -1.000000000000000000, -0.000000000000000000 ) ) ;
#103028 = VECTOR ( 'NONE', #39155, 1000.000000000000000 ) ;
#103029 = CARTESIAN_POINT ( 'NONE',  ( 6.249999999999934275, 12.50000000000000000, -7.253104124594891289 ) ) ;
#103030 = EDGE_LOOP ( 'NONE', ( #94547, #44646, #107048, #24926 ) ) ;
#103031 = CIRCLE ( 'NONE', #23620, 0.06509327318403745899 ) ;
#103032 = ORIENTED_EDGE ( 'NONE', *, *, #65670, .T. ) ;
#103033 = ORIENTED_EDGE ( 'NONE', *, *, #66101, .F. ) ;
#103034 = EDGE_LOOP ( 'NONE', ( #53023, #91002 ) ) ;
#103035 = CARTESIAN_POINT ( 'NONE',  ( -3.100000000000028511, 2.500000000000000000, -0.4464101615137782142 ) ) ;
#103036 = CARTESIAN_POINT ( 'NONE',  ( -0.4000000000000396572, 2.500000000000000000, 3.737306695894644371 ) ) ;
#103037 = CARTESIAN_POINT ( 'NONE',  ( 6.649999999999930189, 2.500000000000000000, -1.572243186433550211 ) ) ;
#103038 = ORIENTED_EDGE ( 'NONE', *, *, #119478, .F. ) ;
#103039 = FACE_BOUND ( 'NONE', #42105, .T. ) ;
#103040 = DIRECTION ( 'NONE',  ( 0.000000000000000000, 0.000000000000000000, -1.000000000000000000 ) ) ;
#103041 = CARTESIAN_POINT ( 'NONE',  ( -10.45000000000000107, 2.500000000000000000, 6.495190528383297135 ) ) ;
#103043 = ADVANCED_FACE ( 'NONE', ( #73532 ), #104919, .T. ) ;
#103042 = DIRECTION ( 'NONE',  ( 0.000000000000000000, 0.000000000000000000, 1.000000000000000000 ) ) ;
#103044 = DIRECTION ( 'NONE',  ( -0.000000000000000000, -1.000000000000000000, -0.000000000000000000 ) ) ;
#103045 = CARTESIAN_POINT ( 'NONE',  ( -6.250000000000021316, 12.50000000000000000, -1.537336459617587581 ) ) ;
#103046 = DIRECTION ( 'NONE',  ( 0.000000000000000000, 0.000000000000000000, 1.000000000000000000 ) ) ;
#103047 = DIRECTION ( 'NONE',  ( 0.000000000000000000, -0.9999939076577903929, 0.003490651415223739937 ) ) ;
#103048 = CARTESIAN_POINT ( 'NONE',  ( 10.39999999999990976, 2.500000000000000000, -4.330127018922201643 ) ) ;
#103049 = CONICAL_SURFACE ( 'NONE', #76156, 0.1000000000000002554, 0.003490658503988666988 ) ;
#103050 = AXIS2_PLACEMENT_3D ( 'NONE', #126966, #117116, #98135 ) ;
#103051 = ADVANCED_FACE ( 'NONE', ( #113466 ), #81941, .T. ) ;
#103052 = DIRECTION ( 'NONE',  ( 0.000000000000000000, 0.000000000000000000, 1.000000000000000000 ) ) ;
#103053 = EDGE_CURVE ( 'NONE', #1029, #82577, #63177, .T. ) ;
#103054 = ORIENTED_EDGE ( 'NONE', *, *, #25571, .T. ) ;
#103055 = CIRCLE ( 'NONE', #46624, 0.1000000000000002554 ) ;
#103056 = ORIENTED_EDGE ( 'NONE', *, *, #43821, .F. ) ;
#103057 = ORIENTED_EDGE ( 'NONE', *, *, #125513, .T. ) ;
#103058 = EDGE_LOOP ( 'NONE', ( #55851, #68260, #117234, #70861 ) ) ;
#103059 = AXIS2_PLACEMENT_3D ( 'NONE', #49776, #90968, #101431 ) ;
#103060 = ORIENTED_EDGE ( 'NONE', *, *, #41554, .T. ) ;
#103061 = CIRCLE ( 'NONE', #40487, 0.1000000000000002554 ) ;
#103062 = EDGE_CURVE ( 'NONE', #69482, #16861, #25506, .T. ) ;
#103063 = ORIENTED_EDGE ( 'NONE', *, *, #20464, .F. ) ;
#103064 = CIRCLE ( 'NONE', #52902, 0.06509327318403745899 ) ;
#103066 = EDGE_CURVE ( 'NONE', #24243, #83715, #12977, .T. ) ;
#103065 = DIRECTION ( 'NONE',  ( 0.000000000000000000, 1.000000000000000000, 0.000000000000000000 ) ) ;
#103068 = ORIENTED_EDGE ( 'NONE', *, *, #19381, .F. ) ;
#103067 = EDGE_CURVE ( 'NONE', #54959, #72089, #42258, .T. ) ;
#103069 = ORIENTED_EDGE ( 'NONE', *, *, #53001, .T. ) ;
#103070 = AXIS2_PLACEMENT_3D ( 'NONE', #79143, #119057, #69285 ) ;
#103071 = CIRCLE ( 'NONE', #82149, 0.09999999999999982514 ) ;
#103072 = CIRCLE ( 'NONE', #44585, 0.09999999999999982514 ) ;
#103073 = EDGE_CURVE ( 'NONE', #122978, #117692, #75680, .T. ) ;
#103074 = CARTESIAN_POINT ( 'NONE',  ( 13.34999999999989662, 2.500000000000000000, -2.857883832488653741 ) ) ;
#103075 = CARTESIAN_POINT ( 'NONE',  ( 5.399999999999931966, 2.500000000000000000, 4.330127018922196314 ) ) ;
#103076 = DIRECTION ( 'NONE',  ( 0.000000000000000000, -0.9999939076577903929, 0.003490651415223739937 ) ) ;
#103077 = AXIS2_PLACEMENT_3D ( 'NONE', #79735, #127549, #37874 ) ;
#103078 = AXIS2_PLACEMENT_3D ( 'NONE', #11651, #12916, #32617 ) ;
#103079 = VERTEX_POINT ( 'NONE', #104299 ) ;
#103080 = DIRECTION ( 'NONE',  ( -0.000000000000000000, 1.000000000000000000, -0.000000000000000000 ) ) ;
#103081 = EDGE_CURVE ( 'NONE', #62968, #50779, #44297, .T. ) ;
#103082 = CIRCLE ( 'NONE', #67554, 2.000000000000000000 ) ;
#103083 = ORIENTED_EDGE ( 'NONE', *, *, #19427, .T. ) ;
#103084 = VERTEX_POINT ( 'NONE', #44745 ) ;
#103085 = DIRECTION ( 'NONE',  ( 0.000000000000000000, 0.000000000000000000, 1.000000000000000000 ) ) ;
#103086 = CARTESIAN_POINT ( 'NONE',  ( -5.850000000000021849, 2.500000000000000000, -5.702370205355749455 ) ) ;
#103087 = EDGE_LOOP ( 'NONE', ( #65476, #94682 ) ) ;
#103088 = UNCERTAINTY_MEASURE_WITH_UNIT (LENGTH_MEASURE( 1.000000000000000082E-05 ), #18362, 'distance_accuracy_value', 'NONE');
#103089 = VERTEX_POINT ( 'NONE', #84657 ) ;
#103090 = AXIS2_PLACEMENT_3D ( 'NONE', #4136, #64364, #12674 ) ;
#103091 = CARTESIAN_POINT ( 'NONE',  ( -6.250000000000015987, 2.500000000000000000, 1.472243186433545459 ) ) ;
#103092 = FACE_OUTER_BOUND ( 'NONE', #25507, .T. ) ;
#103093 = PLANE ( 'NONE',  #24871 ) ;
#103094 = LINE ( 'NONE', #63167, #60843 ) ;
#103095 = CARTESIAN_POINT ( 'NONE',  ( -7.100000000000018296, 2.500000000000000000, 0.09999999999999761857 ) ) ;
#103097 = ORIENTED_EDGE ( 'NONE', *, *, #69363, .T. ) ;
#103096 = CONICAL_SURFACE ( 'NONE', #4877, 0.1000000000000002554, 0.003490658503988666988 ) ;
#103098 = DIRECTION ( 'NONE',  ( -0.000000000000000000, -1.000000000000000000, -0.000000000000000000 ) ) ;
#103099 = AXIS2_PLACEMENT_3D ( 'NONE', #22563, #122672, #62485 ) ;
#103100 = AXIS2_PLACEMENT_3D ( 'NONE', #35445, #106106, #25596 ) ;
#103101 = ORIENTED_EDGE ( 'NONE', *, *, #25448, .T. ) ;
#103102 = CARTESIAN_POINT ( 'NONE',  ( 87.50000000000002842, 7.500000000000000000, -0.6928095518838441880 ) ) ;
#103103 = EDGE_LOOP ( 'NONE', ( #14192, #93346 ) ) ;
#103104 = DIRECTION ( 'NONE',  ( -4.274815082592931898E-19, -0.9999939076577903929, -0.003490651415223739937 ) ) ;
#103105 = DIRECTION ( 'NONE',  ( 0.000000000000000000, 1.000000000000000000, 0.000000000000000000 ) ) ;
#103106 = CARTESIAN_POINT ( 'NONE',  ( 8.749999999999957367, 2.500000000000000000, 2.265063509461097357 ) ) ;
#103108 = CIRCLE ( 'NONE', #109369, 0.1000000000000000472 ) ;
#103107 = LINE ( 'NONE', #53379, #73133 ) ;
#103109 = ORIENTED_EDGE ( 'NONE', *, *, #85309, .T. ) ;
#103110 = AXIS2_PLACEMENT_3D ( 'NONE', #109721, #29237, #39718 ) ;
#103111 = CONICAL_SURFACE ( 'NONE', #52945, 0.1000000000000002554, 0.003490658503988666988 ) ;
#103112 = DIRECTION ( 'NONE',  ( 0.000000000000000000, 1.000000000000000000, 0.000000000000000000 ) ) ;
#103113 = CONICAL_SURFACE ( 'NONE', #9117, 0.1000000000000000472, 0.003490658503988666988 ) ;
#103114 = EDGE_CURVE ( 'NONE', #82944, #23590, #82743, .T. ) ;
#103115 = CARTESIAN_POINT ( 'NONE',  ( -1.250000000000036193, 2.500000000000000000, 1.472243186433545459 ) ) ;
#103116 = EDGE_LOOP ( 'NONE', ( #119450, #64098 ) ) ;
#103117 = ORIENTED_EDGE ( 'NONE', *, *, #81081, .F. ) ;
#103118 = ORIENTED_EDGE ( 'NONE', *, *, #89463, .F. ) ;
#103119 = DIRECTION ( 'NONE',  ( 0.000000000000000000, 0.000000000000000000, 1.000000000000000000 ) ) ;
#103120 = CARTESIAN_POINT ( 'NONE',  ( -12.49999999999999467, 12.50000000000000000, 0.6928203230275535862 ) ) ;
#103121 = CARTESIAN_POINT ( 'NONE',  ( 186.6927083336747160, 6.551208109652275624, -3.782341765624998686 ) ) ;
#103122 = CARTESIAN_POINT ( 'NONE',  ( 3.349999999999941913, 2.500000000000000000, 5.802370205355744659 ) ) ;
#103123 = DIRECTION ( 'NONE',  ( 0.000000000000000000, -0.9999939076577903929, 0.003490651415223739937 ) ) ;
#103124 = EDGE_CURVE ( 'NONE', #43713, #29164, #114749, .T. ) ;
#103125 = CARTESIAN_POINT ( 'NONE',  ( 16.56576425165006583, 1.500000000000000888, -6.084390597445814564 ) ) ;
#103126 = AXIS2_PLACEMENT_3D ( 'NONE', #51379, #127984, #28478 ) ;
#103127 = CIRCLE ( 'NONE', #19493, 0.09999999999999982514 ) ;
#103128 = CIRCLE ( 'NONE', #46693, 0.09999999999999999167 ) ;
#103129 = LINE ( 'NONE', #12158, #88376 ) ;
#103130 = AXIS2_PLACEMENT_3D ( 'NONE', #72946, #10764, #91941 ) ;
#103131 = ORIENTED_EDGE ( 'NONE', *, *, #94919, .F. ) ;
#103132 = DIRECTION ( 'NONE',  ( 0.000000000000000000, 0.000000000000000000, 1.000000000000000000 ) ) ;
#103133 = ORIENTED_EDGE ( 'NONE', *, *, #60515, .F. ) ;
#103134 = DIRECTION ( 'NONE',  ( -0.000000000000000000, -1.000000000000000000, -0.000000000000000000 ) ) ;
#103135 = DIRECTION ( 'NONE',  ( 0.000000000000000000, 1.000000000000000000, 0.000000000000000000 ) ) ;
#103136 = DIRECTION ( 'NONE',  ( 0.000000000000000000, 1.000000000000000000, 0.000000000000000000 ) ) ;
#103137 = DIRECTION ( 'NONE',  ( 0.000000000000000000, -0.000000000000000000, 1.000000000000000000 ) ) ;
#103138 = VERTEX_POINT ( 'NONE', #110664 ) ;
#103139 = DIRECTION ( 'NONE',  ( -0.000000000000000000, 1.000000000000000000, -0.000000000000000000 ) ) ;
#103140 = CARTESIAN_POINT ( 'NONE',  ( 9.349999999999919709, 2.500000000000000000, -6.148780366869526226 ) ) ;
#103142 = ORIENTED_EDGE ( 'NONE', *, *, #119280, .T. ) ;
#103141 = DIRECTION ( 'NONE',  ( 0.000000000000000000, 0.000000000000000000, 1.000000000000000000 ) ) ;
#103143 = AXIS2_PLACEMENT_3D ( 'NONE', #7784, #36631, #5840 ) ;
#103144 = AXIS2_PLACEMENT_3D ( 'NONE', #7597, #47540, #28542 ) ;
#103145 = EDGE_LOOP ( 'NONE', ( #15537, #27003, #1613, #61599 ) ) ;
#103146 = DIRECTION ( 'NONE',  ( -4.274815082592931898E-19, -0.9999939076577903929, -0.003490651415223739937 ) ) ;
#103147 = ADVANCED_FACE ( 'NONE', ( #81840 ), #52709, .T. ) ;
#103148 = AXIS2_PLACEMENT_3D ( 'NONE', #127949, #37651, #58582 ) ;
#103149 = AXIS2_PLACEMENT_3D ( 'NONE', #39396, #89752, #79308 ) ;
#103150 = ORIENTED_EDGE ( 'NONE', *, *, #111799, .T. ) ;
#103151 = AXIS2_PLACEMENT_3D ( 'NONE', #123629, #125564, #73898 ) ;
#103152 = EDGE_LOOP ( 'NONE', ( #60566, #54898, #36692, #88671 ) ) ;
#103153 = CARTESIAN_POINT ( 'NONE',  ( -3.550000000000028688, 2.500000000000000000, 6.841600689897072485 ) ) ;
#103154 = AXIS2_PLACEMENT_3D ( 'NONE', #39566, #119369, #79474 ) ;
#103155 = VERTEX_POINT ( 'NONE', #101505 ) ;
#103156 = DIRECTION ( 'NONE',  ( 0.000000000000000000, 1.000000000000000000, 0.000000000000000000 ) ) ;
#103157 = DIRECTION ( 'NONE',  ( -0.000000000000000000, 1.000000000000000000, -0.000000000000000000 ) ) ;
#103158 = DIRECTION ( 'NONE',  ( 0.000000000000000000, 0.000000000000000000, 1.000000000000000000 ) ) ;
#103159 = ADVANCED_FACE ( 'NONE', ( #90369 ), #710, .T. ) ;
#103161 = ORIENTED_EDGE ( 'NONE', *, *, #51647, .T. ) ;
#103160 = CONICAL_SURFACE ( 'NONE', #71774, 0.1000000000000000472, 0.003490658503988666988 ) ;
#103162 = AXIS2_PLACEMENT_3D ( 'NONE', #38159, #59756, #29618 ) ;
#103163 = DIRECTION ( 'NONE',  ( 0.000000000000000000, 0.000000000000000000, 1.000000000000000000 ) ) ;
#103166 = VERTEX_POINT ( 'NONE', #30199 ) ;
#103165 = CIRCLE ( 'NONE', #2821, 0.09999999999999982514 ) ;
#103164 = CARTESIAN_POINT ( 'NONE',  ( -0.4000000000000392131, 12.50000000000000000, -5.022947341949754119 ) ) ;
#103167 = AXIS2_PLACEMENT_3D ( 'NONE', #17101, #88447, #37442 ) ;
#103168 = EDGE_CURVE ( 'NONE', #85752, #104158, #52797, .T. ) ;
#103169 = FACE_OUTER_BOUND ( 'NONE', #128796, .T. ) ;
#103170 = CARTESIAN_POINT ( 'NONE',  ( -9.150000000000005684, 2.500000000000000000, 5.702370205355745014 ) ) ;
#103171 = EDGE_CURVE ( 'NONE', #94866, #76, #71584, .T. ) ;
#103172 = ORIENTED_EDGE ( 'NONE', *, *, #32022, .F. ) ;
#103173 = EDGE_LOOP ( 'NONE', ( #46883, #115652 ) ) ;
#103174 = EDGE_CURVE ( 'NONE', #120297, #91598, #60923, .T. ) ;
#103175 = EDGE_LOOP ( 'NONE', ( #118373, #33301, #48044, #102725 ) ) ;
#103176 = VERTEX_POINT ( 'NONE', #32136 ) ;
#103177 = DIRECTION ( 'NONE',  ( 0.000000000000000000, 1.000000000000000000, 0.000000000000000000 ) ) ;
#103178 = CARTESIAN_POINT ( 'NONE',  ( 11.84999999999990372, 2.500000000000000000, 1.818653347947321475 ) ) ;
#103179 = DIRECTION ( 'NONE',  ( -0.000000000000000000, 1.000000000000000000, -0.000000000000000000 ) ) ;
#103180 = EDGE_CURVE ( 'NONE', #44047, #32237, #92977, .T. ) ;
#103181 = FACE_BOUND ( 'NONE', #18881, .T. ) ;
#103182 = VERTEX_POINT ( 'NONE', #61592 ) ;
#103183 = CARTESIAN_POINT ( 'NONE',  ( 185.0729166673494888, 4.445597072760120838, -7.699999999999998401 ) ) ;
#103184 = DIRECTION ( 'NONE',  ( 0.000000000000000000, 1.000000000000000000, 0.000000000000000000 ) ) ;
#103185 = FACE_OUTER_BOUND ( 'NONE', #41281, .T. ) ;
#103186 = DIRECTION ( 'NONE',  ( -0.000000000000000000, 1.000000000000000000, -0.000000000000000000 ) ) ;
#103187 = DIRECTION ( 'NONE',  ( 0.000000000000000000, -0.9999939076577903929, 0.003490651415223739937 ) ) ;
#103188 = CARTESIAN_POINT ( 'NONE',  ( -0.2000000000000408673, 2.500000000000000000, -3.883716857408426648 ) ) ;
#103189 = CONICAL_SURFACE ( 'NONE', #63488, 0.1000000000000002554, 0.003490658503988666988 ) ;
#103190 = VECTOR ( 'NONE', #59097, 1000.000000000000000 ) ;
#103191 = DIRECTION ( 'NONE',  ( 0.000000000000000000, 0.000000000000000000, -1.000000000000000000 ) ) ;
#103192 = ORIENTED_EDGE ( 'NONE', *, *, #8522, .T. ) ;
#103193 = ORIENTED_EDGE ( 'NONE', *, *, #8627, .F. ) ;
#103194 = ORIENTED_EDGE ( 'NONE', *, *, #118879, .T. ) ;
#103195 = ORIENTED_EDGE ( 'NONE', *, *, #68797, .T. ) ;
#103196 = ORIENTED_EDGE ( 'NONE', *, *, #97036, .T. ) ;
#103197 = CARTESIAN_POINT ( 'NONE',  ( 13.94999999999989271, 2.500000000000000000, -1.818653347947326138 ) ) ;
#103198 = CARTESIAN_POINT ( 'NONE',  ( -0.8500000000000382805, 2.500000000000000000, -7.188010851410854052 ) ) ;
#103199 = ORIENTED_EDGE ( 'NONE', *, *, #47244, .T. ) ;
#103200 = FACE_BOUND ( 'NONE', #72009, .T. ) ;
#103201 = CIRCLE ( 'NONE', #92747, 0.1000000000000002554 ) ;
#103202 = CONICAL_SURFACE ( 'NONE', #27986, 0.1000000000000002554, 0.003490658503988666988 ) ;
#103203 = CARTESIAN_POINT ( 'NONE',  ( 1.049999999999954525, 2.500000000000000000, 1.718653347947321386 ) ) ;
#103204 = AXIS2_PLACEMENT_3D ( 'NONE', #3587, #15320, #65724 ) ;
#103205 = AXIS2_PLACEMENT_3D ( 'NONE', #79639, #71110, #39748 ) ;
#103206 = EDGE_CURVE ( 'NONE', #95333, #119700, #48605, .T. ) ;
#103207 = EDGE_LOOP ( 'NONE', ( #32268, #124958, #94696, #94366 ) ) ;
#103208 = DIRECTION ( 'NONE',  ( 0.000000000000000000, 0.000000000000000000, 1.000000000000000000 ) ) ;
#103209 = CARTESIAN_POINT ( 'NONE',  ( 2.049999999999950084, 2.500000000000000000, -6.495190528383302464 ) ) ;
#103210 = FACE_OUTER_BOUND ( 'NONE', #65372, .T. ) ;
#103211 = CIRCLE ( 'NONE', #117866, 1.000000000000000888 ) ;
#103212 = ORIENTED_EDGE ( 'NONE', *, *, #110128, .F. ) ;
#103213 = DIRECTION ( 'NONE',  ( 1.000000000000000000, 0.000000000000000000, 0.000000000000000000 ) ) ;
#103214 = EDGE_CURVE ( 'NONE', #42019, #17427, #62230, .T. ) ;
#103215 = ORIENTED_EDGE ( 'NONE', *, *, #97095, .T. ) ;
#103216 = CIRCLE ( 'NONE', #38492, 0.1000000000000000472 ) ;
#103217 = AXIS2_PLACEMENT_3D ( 'NONE', #91206, #122604, #90555 ) ;
#103218 = CIRCLE ( 'NONE', #94811, 0.06509327318403745899 ) ;
#103219 = ORIENTED_EDGE ( 'NONE', *, *, #103821, .T. ) ;
#103220 = ORIENTED_EDGE ( 'NONE', *, *, #11316, .T. ) ;
#103221 = EDGE_CURVE ( 'NONE', #70284, #31342, #19339, .T. ) ;
#103222 = DIRECTION ( 'NONE',  ( 0.000000000000000000, -0.000000000000000000, 1.000000000000000000 ) ) ;
#103223 = CARTESIAN_POINT ( 'NONE',  ( -6.250000000000017764, 12.50000000000000000, 2.922977105672686982 ) ) ;
#103225 = AXIS2_PLACEMENT_3D ( 'NONE', #116084, #26427, #99028 ) ;
#103224 = CARTESIAN_POINT ( 'NONE',  ( 3.349999999999945466, 2.500000000000000000, -7.288010851410854585 ) ) ;
#103227 = ORIENTED_EDGE ( 'NONE', *, *, #42544, .T. ) ;
#103226 = EDGE_CURVE ( 'NONE', #79060, #100871, #86231, .T. ) ;
#103228 = DIRECTION ( 'NONE',  ( 0.000000000000000000, 0.000000000000000000, -1.000000000000000000 ) ) ;
#103229 = ADVANCED_FACE ( 'NONE', ( #50455 ), #29825, .T. ) ;
#103230 = AXIS2_PLACEMENT_3D ( 'NONE', #49283, #77429, #117316 ) ;
#103231 = CARTESIAN_POINT ( 'NONE',  ( 1.649999999999951505, 12.50000000000000000, -1.472243186433550122 ) ) ;
#103233 = EDGE_CURVE ( 'NONE', #890, #75136, #41946, .T. ) ;
#103232 = CARTESIAN_POINT ( 'NONE',  ( 11.24999999999991118, 2.500000000000000000, -2.857883832488653741 ) ) ;
#103234 = CARTESIAN_POINT ( 'NONE',  ( 186.5312500006828031, 9.429780353434619030E-16, -7.700000000000000178 ) ) ;
#103235 = ORIENTED_EDGE ( 'NONE', *, *, #53619, .T. ) ;
#103236 = CARTESIAN_POINT ( 'NONE',  ( 5.799999999999931433, 12.50000000000000000, 4.330127018922196314 ) ) ;
#103237 = ORIENTED_EDGE ( 'NONE', *, *, #40794, .T. ) ;
#103238 = FACE_OUTER_BOUND ( 'NONE', #9982, .T. ) ;
#103239 = EDGE_CURVE ( 'NONE', #14537, #11624, #102972, .T. ) ;
#103240 = ADVANCED_FACE ( 'NONE', ( #41307 ), #72049, .T. ) ;
#103241 = ORIENTED_EDGE ( 'NONE', *, *, #11430, .T. ) ;
#103242 = ORIENTED_EDGE ( 'NONE', *, *, #23119, .F. ) ;
#103243 = CARTESIAN_POINT ( 'NONE',  ( -4.150000000000024336, 2.500000000000000000, -2.165063509461101710 ) ) ;
#103244 = DIRECTION ( 'NONE',  ( -0.000000000000000000, 1.000000000000000000, -0.000000000000000000 ) ) ;
#103245 = CONICAL_SURFACE ( 'NONE', #835, 0.1000000000000002554, 0.003490658503988666988 ) ;
#103246 = DIRECTION ( 'NONE',  ( 0.000000000000000000, -0.000000000000000000, 1.000000000000000000 ) ) ;
#103247 = AXIS2_PLACEMENT_3D ( 'NONE', #107879, #67953, #47045 ) ;
#103248 = FACE_OUTER_BOUND ( 'NONE', #90301, .T. ) ;
#103249 = DIRECTION ( 'NONE',  ( 0.000000000000000000, 0.000000000000000000, -1.000000000000000000 ) ) ;
#103250 = EDGE_LOOP ( 'NONE', ( #126770, #75527 ) ) ;
#103251 = ORIENTED_EDGE ( 'NONE', *, *, #20919, .F. ) ;
#103252 = DIRECTION ( 'NONE',  ( 1.000000000000000000, 0.000000000000000000, 0.000000000000000000 ) ) ;
#103253 = CONICAL_SURFACE ( 'NONE', #117800, 0.1000000000000000472, 0.003490658503988666988 ) ;
#103254 = CIRCLE ( 'NONE', #46822, 0.06509327318403741736 ) ;
#103255 = DIRECTION ( 'NONE',  ( 0.000000000000000000, 0.000000000000000000, 1.000000000000000000 ) ) ;
#103256 = AXIS2_PLACEMENT_3D ( 'NONE', #4224, #15327, #114197 ) ;
#103258 = DIRECTION ( 'NONE',  ( 0.000000000000000000, 0.000000000000000000, -1.000000000000000000 ) ) ;
#103257 = AXIS2_PLACEMENT_3D ( 'NONE', #41963, #92332, #89 ) ;
#103259 = EDGE_LOOP ( 'NONE', ( #370, #28575, #93742, #44087 ) ) ;
#103260 = VERTEX_POINT ( 'NONE', #111291 ) ;
#103261 = CARTESIAN_POINT ( 'NONE',  ( 2.299999999999946976, 12.50000000000000000, 4.676537180435972552 ) ) ;
#103262 = ORIENTED_EDGE ( 'NONE', *, *, #115585, .F. ) ;
#103263 = DIRECTION ( 'NONE',  ( 0.000000000000000000, 1.000000000000000000, 0.000000000000000000 ) ) ;
#103264 = CARTESIAN_POINT ( 'NONE',  ( 7.949999999999925571, 2.500000000000000000, 2.165063509461097713 ) ) ;
#103265 = VECTOR ( 'NONE', #54218, 1000.000000000000000 ) ;
#103266 = AXIS2_PLACEMENT_3D ( 'NONE', #85843, #16451, #6613 ) ;
#103267 = VECTOR ( 'NONE', #58303, 1000.000000000000000 ) ;
#103268 = DIRECTION ( 'NONE',  ( -0.000000000000000000, -1.000000000000000000, -0.000000000000000000 ) ) ;
#103269 = VERTEX_POINT ( 'NONE', #22317 ) ;
#103270 = FACE_OUTER_BOUND ( 'NONE', #9229, .T. ) ;
#103271 = DIRECTION ( 'NONE',  ( -0.000000000000000000, 1.000000000000000000, -0.000000000000000000 ) ) ;
#103272 = CARTESIAN_POINT ( 'NONE',  ( -3.550000000000031797, 2.500000000000000000, -6.148780366869526226 ) ) ;
#103273 = FACE_OUTER_BOUND ( 'NONE', #70859, .T. ) ;
#103274 = AXIS2_PLACEMENT_3D ( 'NONE', #15020, #42605, #72695 ) ;
#103275 = CARTESIAN_POINT ( 'NONE',  ( -10.85000000000000142, 12.50000000000000000, -2.230156782645135394 ) ) ;
#103276 = ORIENTED_EDGE ( 'NONE', *, *, #120900, .T. ) ;
#103277 = CARTESIAN_POINT ( 'NONE',  ( 13.29999999999989946, 2.500000000000000000, -0.1000000000000023925 ) ) ;
#103278 = ADVANCED_FACE ( 'NONE', ( #53048 ), #90433, .T. ) ;
#103279 = CARTESIAN_POINT ( 'NONE',  ( -8.749999999999971578, 12.50000000000000000, 6.495190528383297135 ) ) ;
#103280 = AXIS2_PLACEMENT_3D ( 'NONE', #18566, #38220, #27730 ) ;
#103281 = ORIENTED_EDGE ( 'NONE', *, *, #16553, .F. ) ;
#103282 = EDGE_LOOP ( 'NONE', ( #14661, #100272, #121604, #104580 ) ) ;
#103283 = CARTESIAN_POINT ( 'NONE',  ( 184.8177083336747160, 4.367472073101515306, 7.564683531250000925 ) ) ;
#103284 = CARTESIAN_POINT ( 'NONE',  ( 8.149999999999923972, 12.50000000000000000, 2.576566944158910744 ) ) ;
#103285 = CARTESIAN_POINT ( 'NONE',  ( 9.599999999999914380, 2.500000000000000000, 4.430127018922196847 ) ) ;
#103286 = CIRCLE ( 'NONE', #69825, 0.09999999999999982514 ) ;
#103287 = FACE_OUTER_BOUND ( 'NONE', #24822, .T. ) ;
#103288 = DIRECTION ( 'NONE',  ( 0.000000000000000000, 0.000000000000000000, 1.000000000000000000 ) ) ;
#103289 = ADVANCED_FACE ( 'NONE', ( #70113 ), #13070, .T. ) ;
#103290 = LINE ( 'NONE', #53545, #32523 ) ;
#103291 = DIRECTION ( 'NONE',  ( 0.000000000000000000, 0.000000000000000000, -1.000000000000000000 ) ) ;
#103292 = DIRECTION ( 'NONE',  ( 0.000000000000000000, 0.000000000000000000, 1.000000000000000000 ) ) ;
#103293 = DIRECTION ( 'NONE',  ( 0.000000000000000000, 0.000000000000000000, 1.000000000000000000 ) ) ;
#103294 = DIRECTION ( 'NONE',  ( 0.000000000000000000, 1.000000000000000000, 0.000000000000000000 ) ) ;
#103296 = CONICAL_SURFACE ( 'NONE', #107493, 0.1000000000000002554, 0.003490658503988666988 ) ;
#103295 = FACE_OUTER_BOUND ( 'NONE', #114993, .T. ) ;
#103297 = EDGE_LOOP ( 'NONE', ( #88089, #105396, #69123, #21672 ) ) ;
#103298 = CIRCLE ( 'NONE', #48922, 0.06509327318403745899 ) ;
#103299 = EDGE_LOOP ( 'NONE', ( #84187, #2941 ) ) ;
#103300 = EDGE_LOOP ( 'NONE', ( #105748, #39484, #3990, #96642 ) ) ;
#103301 = ORIENTED_EDGE ( 'NONE', *, *, #68155, .F. ) ;
#103302 = CONICAL_SURFACE ( 'NONE', #40331, 0.1000000000000000056, 0.003490658503988666988 ) ;
#103303 = CARTESIAN_POINT ( 'NONE',  ( -11.04999999999999893, 12.50000000000000000, 6.148780366869520009 ) ) ;
#103304 = DIRECTION ( 'NONE',  ( 0.000000000000000000, 1.000000000000000000, 0.000000000000000000 ) ) ;
#103305 = ORIENTED_EDGE ( 'NONE', *, *, #61396, .F. ) ;
#103306 = DIRECTION ( 'NONE',  ( -0.000000000000000000, 1.000000000000000000, -0.000000000000000000 ) ) ;
#103307 = AXIS2_PLACEMENT_3D ( 'NONE', #61801, #19936, #59882 ) ;
#103308 = DIRECTION ( 'NONE',  ( 0.000000000000000000, 1.000000000000000000, 0.000000000000000000 ) ) ;
#103310 = ORIENTED_EDGE ( 'NONE', *, *, #67726, .T. ) ;
#103309 = CARTESIAN_POINT ( 'NONE',  ( -2.900000000000029221, 2.500000000000000000, -5.122947341949753763 ) ) ;
#103311 = DIRECTION ( 'NONE',  ( 0.000000000000000000, 0.000000000000000000, 1.000000000000000000 ) ) ;
#103312 = CARTESIAN_POINT ( 'NONE',  ( 4.349999999999940137, 2.500000000000000000, -2.511473670974877948 ) ) ;
#103313 = VERTEX_POINT ( 'NONE', #10523 ) ;
#103314 = CIRCLE ( 'NONE', #9307, 0.09999999999999982514 ) ;
#103315 = CIRCLE ( 'NONE', #90785, 0.06509327318403745899 ) ;
#103316 = EDGE_LOOP ( 'NONE', ( #115768, #123703, #43235, #69719 ) ) ;
#103317 = ORIENTED_EDGE ( 'NONE', *, *, #16355, .F. ) ;
#103318 = VERTEX_POINT ( 'NONE', #123688 ) ;
#103319 = CARTESIAN_POINT ( 'NONE',  ( 9.999999999999912959, 2.500000000000000000, -4.922947341949753586 ) ) ;
#103320 = AXIS2_PLACEMENT_3D ( 'NONE', #72794, #51237, #121883 ) ;
#103321 = DIRECTION ( 'NONE',  ( 0.000000000000000000, -0.000000000000000000, 1.000000000000000000 ) ) ;
#103322 = DIRECTION ( 'NONE',  ( 0.000000000000000000, 0.000000000000000000, 1.000000000000000000 ) ) ;
#103323 = CIRCLE ( 'NONE', #23909, 0.06509327318403745899 ) ;
#103324 = CYLINDRICAL_SURFACE ( 'NONE', #60424, 7.699999999999999289 ) ;
#103325 = EDGE_CURVE ( 'NONE', #54263, #89280, #88284, .T. ) ;
#103326 = ORIENTED_EDGE ( 'NONE', *, *, #67717, .T. ) ;
#103327 = CARTESIAN_POINT ( 'NONE',  ( -11.05000000000000071, 12.50000000000000000, -2.446380397790836270 ) ) ;
#103328 = EDGE_LOOP ( 'NONE', ( #15239, #18916 ) ) ;
#103329 = FACE_OUTER_BOUND ( 'NONE', #78765, .T. ) ;
#103330 = DIRECTION ( 'NONE',  ( 0.000000000000000000, 0.000000000000000000, 1.000000000000000000 ) ) ;
#103331 = EDGE_CURVE ( 'NONE', #7558, #73190, #63263, .T. ) ;
#103332 = DIRECTION ( 'NONE',  ( -4.274815082592931898E-19, -0.9999939076577903929, -0.003490651415223739937 ) ) ;
#103333 = DIRECTION ( 'NONE',  ( 0.000000000000000000, 1.000000000000000000, 0.000000000000000000 ) ) ;
#103334 = EDGE_CURVE ( 'NONE', #93212, #11168, #17265, .T. ) ;
#103335 = ORIENTED_EDGE ( 'NONE', *, *, #59304, .F. ) ;
#103336 = AXIS2_PLACEMENT_3D ( 'NONE', #27584, #106794, #17100 ) ;
#103337 = EDGE_LOOP ( 'NONE', ( #67491, #65895, #59711, #77232 ) ) ;
#103338 = ADVANCED_FACE ( 'NONE', ( #54330 ), #83783, .T. ) ;
#103339 = CIRCLE ( 'NONE', #86592, 0.06509327318403741736 ) ;
#103341 = ORIENTED_EDGE ( 'NONE', *, *, #31895, .F. ) ;
#103340 = EDGE_CURVE ( 'NONE', #6261, #54499, #113905, .T. ) ;
#103342 = LINE ( 'NONE', #102049, #7179 ) ;
#103344 = CIRCLE ( 'NONE', #122124, 0.06509327318403745899 ) ;
#103343 = CARTESIAN_POINT ( 'NONE',  ( 7.899999999999923084, 12.50000000000000000, -0.6928203230275542523 ) ) ;
#103345 = AXIS2_PLACEMENT_3D ( 'NONE', #494, #12251, #40459 ) ;
#103346 = CARTESIAN_POINT ( 'NONE',  ( -8.350000000000012079, 2.500000000000000000, -1.472243186433550122 ) ) ;
#103347 = ADVANCED_FACE ( 'NONE', ( #54965 ), #107167, .T. ) ;
#103348 = FACE_BOUND ( 'NONE', #65773, .T. ) ;
#103349 = DIRECTION ( 'NONE',  ( 0.000000000000000000, 1.000000000000000000, 0.000000000000000000 ) ) ;
#103350 = DIRECTION ( 'NONE',  ( 0.000000000000000000, 0.000000000000000000, 1.000000000000000000 ) ) ;
#103351 = DIRECTION ( 'NONE',  ( 0.000000000000000000, 0.000000000000000000, 1.000000000000000000 ) ) ;
#103352 = CIRCLE ( 'NONE', #46917, 0.1000000000000002554 ) ;
#103353 = CIRCLE ( 'NONE', #105494, 0.06509327318403745899 ) ;
#103354 = VECTOR ( 'NONE', #36316, 1000.000000000000000 ) ;
#103355 = CARTESIAN_POINT ( 'NONE',  ( 2.500000000000002220, 2.500000000000000000, 9.000000000000003553 ) ) ;
#103356 = FACE_OUTER_BOUND ( 'NONE', #118888, .T. ) ;
#103357 = DIRECTION ( 'NONE',  ( 0.000000000000000000, -0.000000000000000000, 1.000000000000000000 ) ) ;
#103358 = VERTEX_POINT ( 'NONE', #45808 ) ;
#103359 = VECTOR ( 'NONE', #37793, 1000.000000000000000 ) ;
#103360 = AXIS2_PLACEMENT_3D ( 'NONE', #77193, #109213, #58842 ) ;
#103361 = VECTOR ( 'NONE', #42535, 1000.000000000000000 ) ;
#103362 = LINE ( 'NONE', #5138, #5680 ) ;
#103363 = ORIENTED_EDGE ( 'NONE', *, *, #108983, .F. ) ;
#103364 = VERTEX_POINT ( 'NONE', #84434 ) ;
#103365 = DIRECTION ( 'NONE',  ( 0.000000000000000000, 1.000000000000000000, 0.000000000000000000 ) ) ;
#103366 = FACE_BOUND ( 'NONE', #104999, .T. ) ;
#103367 = LINE ( 'NONE', #113170, #84961 ) ;
#103368 = EDGE_LOOP ( 'NONE', ( #110815, #50946 ) ) ;
#103369 = CARTESIAN_POINT ( 'NONE',  ( 23.85240649353447751, 2.660544618071316147, 4.258220037268930724 ) ) ;
#103370 = FACE_OUTER_BOUND ( 'NONE', #78666, .T. ) ;
#103371 = ORIENTED_EDGE ( 'NONE', *, *, #61010, .F. ) ;
#103372 = DIRECTION ( 'NONE',  ( 0.000000000000000000, 1.000000000000000000, 0.000000000000000000 ) ) ;
#103373 = CARTESIAN_POINT ( 'NONE',  ( -3.749999999999994671, 2.500000000000000000, -6.595190528383302109 ) ) ;
#103374 = EDGE_CURVE ( 'NONE', #81926, #118944, #21402, .T. ) ;
#103375 = ORIENTED_EDGE ( 'NONE', *, *, #45549, .F. ) ;
#103376 = EDGE_CURVE ( 'NONE', #43898, #118209, #75776, .T. ) ;
#103377 = CARTESIAN_POINT ( 'NONE',  ( -6.050000000000017586, 12.50000000000000000, 1.883746621131358934 ) ) ;
#103378 = CARTESIAN_POINT ( 'NONE',  ( -6.050000000000018474, 12.50000000000000000, 6.841600689897072485 ) ) ;
#103379 = ADVANCED_FACE ( 'NONE', ( #125001 ), #105018, .T. ) ;
#103380 = AXIS2_PLACEMENT_3D ( 'NONE', #6273, #46218, #86119 ) ;
#103381 = ORIENTED_EDGE ( 'NONE', *, *, #43425, .T. ) ;
#103382 = DIRECTION ( 'NONE',  ( -0.000000000000000000, -1.000000000000000000, -0.000000000000000000 ) ) ;
#103383 = CARTESIAN_POINT ( 'NONE',  ( 0.5999999999999612310, 2.500000000000000000, -0.3464101615137760715 ) ) ;
#103385 = ADVANCED_FACE ( 'NONE', ( #34716 ), #117611, .T. ) ;
#103384 = PLANE ( 'NONE',  #47217 ) ;
#103386 = ADVANCED_FACE ( 'NONE', ( #124367 ), #13742, .T. ) ;
#103387 = EDGE_LOOP ( 'NONE', ( #63400, #98559, #27090, #113664 ) ) ;
#103388 = ORIENTED_EDGE ( 'NONE', *, *, #103781, .F. ) ;
#103389 = ADVANCED_FACE ( 'NONE', ( #53687 ), #65305, .T. ) ;
#103390 = CARTESIAN_POINT ( 'NONE',  ( 195.0000000000000000, 0.000000000000000000, 0.000000000000000000 ) ) ;
#103391 = EDGE_LOOP ( 'NONE', ( #79103, #60803, #11945, #31967 ) ) ;
#103392 = CARTESIAN_POINT ( 'NONE',  ( 4.399999999999940847, 12.50000000000000000, -4.611443907251939756 ) ) ;
#103393 = CARTESIAN_POINT ( 'NONE',  ( 5.649999999999934630, 12.50000000000000000, 6.083687093685483660 ) ) ;
#103394 = ADVANCED_FACE ( 'NONE', ( #93608 ), #8871, .T. ) ;
#103395 = AXIS2_PLACEMENT_3D ( 'NONE', #52601, #42822, #74185 ) ;
#103396 = ADVANCED_FACE ( 'NONE', ( #64143 ), #105364, .F. ) ;
#103397 = ORIENTED_EDGE ( 'NONE', *, *, #37475, .F. ) ;
#103398 = CARTESIAN_POINT ( 'NONE',  ( 9.599999999999914380, 2.500000000000000000, -4.330127018922201643 ) ) ;
#103399 = CARTESIAN_POINT ( 'NONE',  ( -9.600000000000008527, 12.50000000000000000, 4.265033745738159077 ) ) ;
#103400 = CARTESIAN_POINT ( 'NONE',  ( -1.650000000000035216, 2.500000000000000000, -5.902370205355750521 ) ) ;
#103401 = DIRECTION ( 'NONE',  ( 0.000000000000000000, 1.000000000000000000, 0.000000000000000000 ) ) ;
#103403 = EDGE_CURVE ( 'NONE', #3528, #11005, #98763, .T. ) ;
#103402 = CARTESIAN_POINT ( 'NONE',  ( -10.00000000000000533, 12.50000000000000000, -4.957854068765712441 ) ) ;
#103404 = VERTEX_POINT ( 'NONE', #96174 ) ;
#103405 = ORIENTED_EDGE ( 'NONE', *, *, #11627, .F. ) ;
#103406 = DIRECTION ( 'NONE',  ( 0.000000000000000000, 0.000000000000000000, 1.000000000000000000 ) ) ;
#103407 = VECTOR ( 'NONE', #97230, 1000.000000000000000 ) ;
#103408 = CIRCLE ( 'NONE', #63704, 0.06509327318403745899 ) ;
#103409 = CARTESIAN_POINT ( 'NONE',  ( 104.2471014634786712, 6.952484616901103642, -3.319144779746969309 ) ) ;
#103411 = ORIENTED_EDGE ( 'NONE', *, *, #47010, .T. ) ;
#103410 = EDGE_LOOP ( 'NONE', ( #104729, #37915 ) ) ;
#103412 = ORIENTED_EDGE ( 'NONE', *, *, #51487, .F. ) ;
#103413 = CIRCLE ( 'NONE', #28103, 0.4999999999999995559 ) ;
#103414 = CARTESIAN_POINT ( 'NONE',  ( -2.050000000000032685, 12.50000000000000000, -2.230156782645139391 ) ) ;
#103415 = CIRCLE ( 'NONE', #105465, 0.06509327318403741736 ) ;
#103416 = LINE ( 'NONE', #43222, #119602 ) ;
#103417 = DIRECTION ( 'NONE',  ( 0.000000000000000000, 0.000000000000000000, 1.000000000000000000 ) ) ;
#103418 =( LENGTH_UNIT ( ) NAMED_UNIT ( * ) SI_UNIT ( .MILLI., .METRE. ) );
#103419 = CARTESIAN_POINT ( 'NONE',  ( 2.500000000000002220, -1.500000000000000000, 10.00000000000000178 ) ) ;
#103420 = CARTESIAN_POINT ( 'NONE',  ( 1.049999999999954525, 2.500000000000000000, 1.818653347947321475 ) ) ;
#103421 = DIRECTION ( 'NONE',  ( 0.000000000000000000, -0.9999939076577903929, 0.003490651415223739937 ) ) ;
#103422 = DIRECTION ( 'NONE',  ( 0.000000000000000000, 0.000000000000000000, -1.000000000000000000 ) ) ;
#103423 = CARTESIAN_POINT ( 'NONE',  ( 10.64999999999990976, 2.500000000000000000, -6.148780366869526226 ) ) ;
#103424 = FACE_OUTER_BOUND ( 'NONE', #65894, .T. ) ;
#103425 = VERTEX_POINT ( 'NONE', #14385 ) ;
#103426 = CIRCLE ( 'NONE', #107626, 0.06509327318403745899 ) ;
#103427 = CIRCLE ( 'NONE', #46998, 0.06509327318403745899 ) ;
#103428 = FACE_OUTER_BOUND ( 'NONE', #123495, .T. ) ;
#103429 = AXIS2_PLACEMENT_3D ( 'NONE', #120023, #129224, #38915 ) ;
#103430 = VECTOR ( 'NONE', #6926, 1000.000000000000000 ) ;
#103431 = EDGE_LOOP ( 'NONE', ( #15324, #108687, #37946, #43367 ) ) ;
#103432 = ORIENTED_EDGE ( 'NONE', *, *, #94169, .F. ) ;
#103433 = CARTESIAN_POINT ( 'NONE',  ( 185.0000000000000000, 0.000000000000000000, 7.700000000000000178 ) ) ;
#103434 = DIRECTION ( 'NONE',  ( 0.000000000000000000, 0.000000000000000000, 1.000000000000000000 ) ) ;
#103435 = DIRECTION ( 'NONE',  ( -0.000000000000000000, -1.000000000000000000, -0.000000000000000000 ) ) ;
#103436 = VECTOR ( 'NONE', #48203, 1000.000000000000000 ) ;
#103437 = DIRECTION ( 'NONE',  ( 0.000000000000000000, 0.000000000000000000, 1.000000000000000000 ) ) ;
#103438 = EDGE_CURVE ( 'NONE', #53090, #93141, #43885, .T. ) ;
#103439 = AXIS2_PLACEMENT_3D ( 'NONE', #113192, #34006, #23528 ) ;
#103441 = DIRECTION ( 'NONE',  ( 0.000000000000000000, -0.9999939076577903929, 0.003490651415223739937 ) ) ;
#103440 = CIRCLE ( 'NONE', #38714, 0.1000000000000000472 ) ;
#103442 = CARTESIAN_POINT ( 'NONE',  ( 185.8645833340161175, -6.668395609140180369, 3.849999999999994760 ) ) ;
#103443 = DIRECTION ( 'NONE',  ( 0.000000000000000000, 0.000000000000000000, -1.000000000000000000 ) ) ;
#103444 = VERTEX_POINT ( 'NONE', #106647 ) ;
#103445 = DIRECTION ( 'NONE',  ( 0.000000000000000000, 0.000000000000000000, 1.000000000000000000 ) ) ;
#103446 = AXIS2_PLACEMENT_3D ( 'NONE', #75760, #98610, #58079 ) ;
#103447 = DIRECTION ( 'NONE',  ( -1.000000000000000000, -0.000000000000000000, -0.000000000000000000 ) ) ;
#103449 = ORIENTED_EDGE ( 'NONE', *, *, #66003, .T. ) ;
#103448 = AXIS2_PLACEMENT_3D ( 'NONE', #15521, #54804, #94735 ) ;
#103450 = AXIS2_PLACEMENT_3D ( 'NONE', #92246, #62805, #102704 ) ;
#103451 = ORIENTED_EDGE ( 'NONE', *, *, #104526, .T. ) ;
#103452 = ORIENTED_EDGE ( 'NONE', *, *, #87822, .T. ) ;
#103453 = CIRCLE ( 'NONE', #49085, 0.09999999999999982514 ) ;
#103454 = VERTEX_POINT ( 'NONE', #39237 ) ;
#103455 = DIRECTION ( 'NONE',  ( 0.000000000000000000, 1.000000000000000000, 0.000000000000000000 ) ) ;
#103456 = CARTESIAN_POINT ( 'NONE',  ( 6.699999999999930012, 2.500000000000000000, 4.430127018922196847 ) ) ;
#103457 = CARTESIAN_POINT ( 'NONE',  ( 14.34999999999989662, 2.500000000000000000, 2.611473670974873151 ) ) ;
#103458 = CARTESIAN_POINT ( 'NONE',  ( 7.099999999999928590, 2.500000000000000000, -4.430127018922202176 ) ) ;
#103459 = CARTESIAN_POINT ( 'NONE',  ( -7.700000000000012612, 2.500000000000000000, 4.676537180435972552 ) ) ;
#103460 = ORIENTED_EDGE ( 'NONE', *, *, #51546, .T. ) ;
#103461 = CARTESIAN_POINT ( 'NONE',  ( 32.27737262862851964, -1.406459147574385504, 4.686451386305379607 ) ) ;
#103462 = DIRECTION ( 'NONE',  ( -0.000000000000000000, 1.000000000000000000, -0.000000000000000000 ) ) ;
#103463 = DIRECTION ( 'NONE',  ( 0.000000000000000000, -0.9999939076577903929, 0.003490651415223739937 ) ) ;
#103464 = CIRCLE ( 'NONE', #76270, 0.06509327318403745899 ) ;
#103465 = CARTESIAN_POINT ( 'NONE',  ( -9.150000000000009237, 2.500000000000000000, -6.495190528383297135 ) ) ;
#103466 = ORIENTED_EDGE ( 'NONE', *, *, #43501, .T. ) ;
#103467 = VERTEX_POINT ( 'NONE', #27429 ) ;
#103468 = ORIENTED_EDGE ( 'NONE', *, *, #49808, .F. ) ;
#103469 = CARTESIAN_POINT ( 'NONE',  ( 0.3999999999999619971, 2.500000000000000000, -0.1000000000000001166 ) ) ;
#103470 = CONICAL_SURFACE ( 'NONE', #95155, 0.09999999999999982514, 0.003490658503988666988 ) ;
#103471 = DIRECTION ( 'NONE',  ( -0.000000000000000000, 1.000000000000000000, -0.000000000000000000 ) ) ;
#103472 = CARTESIAN_POINT ( 'NONE',  ( -14.39999999999998614, 2.500000000000000000, -0.4464101615137760493 ) ) ;
#103473 = VECTOR ( 'NONE', #111049, 1000.000000000000000 ) ;
#103474 = EDGE_CURVE ( 'NONE', #49409, #70661, #2613, .T. ) ;
#103475 = ORIENTED_EDGE ( 'NONE', *, *, #102803, .F. ) ;
#103476 = LINE ( 'NONE', #104121, #51580 ) ;
#103477 = CARTESIAN_POINT ( 'NONE',  ( 10.19999999999991580, 2.500000000000000000, -0.3464101615137783474 ) ) ;
#103478 = EDGE_CURVE ( 'NONE', #14553, #52245, #107290, .T. ) ;
#103479 = CARTESIAN_POINT ( 'NONE',  ( -12.49999999999999289, 12.50000000000000000, -0.6277270498435125745 ) ) ;
#103480 = LINE ( 'NONE', #115196, #79135 ) ;
#103481 = EDGE_CURVE ( 'NONE', #460, #4381, #126945, .T. ) ;
#103482 = CARTESIAN_POINT ( 'NONE',  ( -10.80000000000000071, 2.500000000000000000, 4.330127018922196314 ) ) ;
#103483 = AXIS2_PLACEMENT_3D ( 'NONE', #25428, #113842, #24164 ) ;
#103484 = ORIENTED_EDGE ( 'NONE', *, *, #88816, .T. ) ;
#103485 = EDGE_CURVE ( 'NONE', #21052, #115754, #69515, .T. ) ;
#103486 = EDGE_CURVE ( 'NONE', #21966, #81870, #121842, .T. ) ;
#103487 = ORIENTED_EDGE ( 'NONE', *, *, #29630, .T. ) ;
#103488 = EDGE_CURVE ( 'NONE', #3295, #13562, #29918, .T. ) ;
#103490 = EDGE_CURVE ( 'NONE', #88669, #42865, #26187, .T. ) ;
#103489 = CARTESIAN_POINT ( 'NONE',  ( 106.0514428414850272, 8.500000000000000000, 1.125000000000000444 ) ) ;
#103491 = EDGE_CURVE ( 'NONE', #92653, #106656, #58843, .T. ) ;
#103492 = DIRECTION ( 'NONE',  ( -0.000000000000000000, 1.000000000000000000, -0.000000000000000000 ) ) ;
#103493 = DIRECTION ( 'NONE',  ( 0.000000000000000000, 1.000000000000000000, 0.000000000000000000 ) ) ;
#103494 = DIRECTION ( 'NONE',  ( 0.000000000000000000, 1.000000000000000000, 0.000000000000000000 ) ) ;
#103495 = CARTESIAN_POINT ( 'NONE',  ( 0.6499999999999543920, 12.50000000000000000, 6.148780366869520897 ) ) ;
#103496 = ORIENTED_EDGE ( 'NONE', *, *, #51888, .T. ) ;
#103497 = AXIS2_PLACEMENT_3D ( 'NONE', #108960, #960, #60556 ) ;
#103498 = CIRCLE ( 'NONE', #15643, 0.06509327318403745899 ) ;
#103499 = VERTEX_POINT ( 'NONE', #48378 ) ;
#103500 = CARTESIAN_POINT ( 'NONE',  ( 8.299999999999922551, 12.50000000000000000, 4.395220292106234439 ) ) ;
#103501 = LINE ( 'NONE', #13808, #44705 ) ;
#103502 = EDGE_CURVE ( 'NONE', #106434, #109438, #84286, .T. ) ;
#103503 = CARTESIAN_POINT ( 'NONE',  ( 17.99892161670943480, -2.500000000000000444, -4.934975022999348759 ) ) ;
#103504 = DIRECTION ( 'NONE',  ( 0.000000000000000000, 1.000000000000000000, 0.000000000000000000 ) ) ;
#103505 = ORIENTED_EDGE ( 'NONE', *, *, #77746, .F. ) ;
#103507 = EDGE_CURVE ( 'NONE', #80752, #76477, #61313, .T. ) ;
#103506 = DIRECTION ( 'NONE',  ( 0.000000000000000000, -0.000000000000000000, 1.000000000000000000 ) ) ;
#103508 = DIRECTION ( 'NONE',  ( 0.000000000000000000, 0.000000000000000000, -1.000000000000000000 ) ) ;
#103509 = EDGE_LOOP ( 'NONE', ( #125413, #85453, #87036, #44618 ) ) ;
#103510 = DIRECTION ( 'NONE',  ( 0.000000000000000000, 0.000000000000000000, -1.000000000000000000 ) ) ;
#103511 = AXIS2_PLACEMENT_3D ( 'NONE', #91024, #22933, #102759 ) ;
#103512 = ORIENTED_EDGE ( 'NONE', *, *, #98526, .F. ) ;
#103513 = DIRECTION ( 'NONE',  ( 0.000000000000000000, 0.000000000000000000, 1.000000000000000000 ) ) ;
#103514 = AXIS2_PLACEMENT_3D ( 'NONE', #62727, #63358, #124210 ) ;
#103515 = ORIENTED_EDGE ( 'NONE', *, *, #99521, .F. ) ;
#103516 = CARTESIAN_POINT ( 'NONE',  ( -4.150000000000024336, 12.50000000000000000, -2.857883832488653741 ) ) ;
#103517 = CARTESIAN_POINT ( 'NONE',  ( -0.8500000000000386136, 12.50000000000000000, 5.802370205355744659 ) ) ;
#103518 = CONICAL_SURFACE ( 'NONE', #118179, 0.09999999999999982514, 0.003490658503988666988 ) ;
#103519 = AXIS2_PLACEMENT_3D ( 'NONE', #70081, #40643, #107419 ) ;
#103520 = ORIENTED_EDGE ( 'NONE', *, *, #69353, .F. ) ;
#103521 = ORIENTED_EDGE ( 'NONE', *, *, #8944, .F. ) ;
#103522 = CARTESIAN_POINT ( 'NONE',  ( 185.8385416670080872, 6.551208109652274736, 3.782341765625001351 ) ) ;
#103523 = FACE_OUTER_BOUND ( 'NONE', #109190, .T. ) ;
#103524 = CARTESIAN_POINT ( 'NONE',  ( 186.2968750003414584, 8.734944146203032389, 5.348610694689227483E-16 ) ) ;
#103525 = CARTESIAN_POINT ( 'NONE',  ( 184.9010416670080588, -4.367472073101520635, 7.564683531249999149 ) ) ;
#103526 = AXIS2_PLACEMENT_3D ( 'NONE', #43400, #32943, #75404 ) ;
#103527 = AXIS2_PLACEMENT_3D ( 'NONE', #69243, #97423, #7752 ) ;
#103528 = CIRCLE ( 'NONE', #97258, 0.06509327318403745899 ) ;
#103529 = LINE ( 'NONE', #51219, #68136 ) ;
#103530 = CARTESIAN_POINT ( 'NONE',  ( -13.09999999999999254, 2.500000000000000000, -0.4464101615137741064 ) ) ;
#103531 = CIRCLE ( 'NONE', #86794, 0.09999999999999982514 ) ;
#103532 = CARTESIAN_POINT ( 'NONE',  ( -7.900000000000011013, 12.50000000000000000, 5.022947341949748790 ) ) ;
#103533 = ADVANCED_FACE ( 'NONE', ( #37907 ), #126297, .T. ) ;
#103534 = CARTESIAN_POINT ( 'NONE',  ( -13.74999999999998757, 12.50000000000000000, 1.472243186433549456 ) ) ;
#103535 = EDGE_CURVE ( 'NONE', #15950, #22180, #87005, .T. ) ;
#103536 = AXIS2_PLACEMENT_3D ( 'NONE', #115497, #52729, #25193 ) ;
#103537 = CIRCLE ( 'NONE', #109797, 0.06509327318403745899 ) ;
#103538 = VERTEX_POINT ( 'NONE', #9091 ) ;
#103539 = EDGE_CURVE ( 'NONE', #40733, #99388, #42451, .T. ) ;
#103540 = ORIENTED_EDGE ( 'NONE', *, *, #27522, .F. ) ;
#103541 = DIRECTION ( 'NONE',  ( 0.000000000000000000, 0.000000000000000000, 1.000000000000000000 ) ) ;
#103542 = ORIENTED_EDGE ( 'NONE', *, *, #22733, .F. ) ;
#103543 = CARTESIAN_POINT ( 'NONE',  ( 187.3750000000000000, 8.891194145520236347, 5.444286225454521982E-16 ) ) ;
#103544 = DIRECTION ( 'NONE',  ( 0.000000000000000000, 1.000000000000000000, 0.000000000000000000 ) ) ;
#103545 = AXIS2_PLACEMENT_3D ( 'NONE', #127131, #57072, #19751 ) ;
#103546 = DIRECTION ( 'NONE',  ( 0.000000000000000000, 0.000000000000000000, 1.000000000000000000 ) ) ;
#103548 = VERTEX_POINT ( 'NONE', #96819 ) ;
#103547 = VERTEX_POINT ( 'NONE', #29396 ) ;
#103549 = CARTESIAN_POINT ( 'NONE',  ( 6.249999999999930722, 2.500000000000000000, -1.572243186433550211 ) ) ;
#103550 = ORIENTED_EDGE ( 'NONE', *, *, #44534, .T. ) ;
#103551 = EDGE_CURVE ( 'NONE', #22696, #58191, #21508, .T. ) ;
#103552 = DIRECTION ( 'NONE',  ( -0.000000000000000000, -1.000000000000000000, -0.000000000000000000 ) ) ;
#103553 = CARTESIAN_POINT ( 'NONE',  ( -10.85000000000000142, 2.500000000000000000, 2.165063509461097713 ) ) ;
#103554 = EDGE_CURVE ( 'NONE', #121714, #82618, #46636, .T. ) ;
#103555 = FACE_OUTER_BOUND ( 'NONE', #101511, .T. ) ;
#103556 = DIRECTION ( 'NONE',  ( 0.000000000000000000, 0.000000000000000000, -1.000000000000000000 ) ) ;
#103557 = DIRECTION ( 'NONE',  ( 0.000000000000000000, 1.000000000000000000, 0.000000000000000000 ) ) ;
#103558 = EDGE_CURVE ( 'NONE', #20569, #31101, #92611, .T. ) ;
#103559 = DIRECTION ( 'NONE',  ( 0.000000000000000000, 0.000000000000000000, -1.000000000000000000 ) ) ;
#103560 = CARTESIAN_POINT ( 'NONE',  ( -12.89999999999999325, 12.50000000000000000, -3.702399969078684627 ) ) ;
#103561 = LINE ( 'NONE', #64261, #5576 ) ;
#103562 = DIRECTION ( 'NONE',  ( -0.000000000000000000, -1.000000000000000000, -0.000000000000000000 ) ) ;
#103563 = DIRECTION ( 'NONE',  ( 0.000000000000000000, 0.000000000000000000, -1.000000000000000000 ) ) ;
#103564 = AXIS2_PLACEMENT_3D ( 'NONE', #5319, #15783, #45266 ) ;
#103566 = EDGE_CURVE ( 'NONE', #40625, #25430, #77196, .T. ) ;
#103565 = CARTESIAN_POINT ( 'NONE',  ( -9.400000000000009237, 2.500000000000000000, -4.576537180435973795 ) ) ;
#103567 = VERTEX_POINT ( 'NONE', #97475 ) ;
#103568 = ORIENTED_EDGE ( 'NONE', *, *, #123934, .F. ) ;
#103569 = VERTEX_POINT ( 'NONE', #28940 ) ;
#103570 = DIRECTION ( 'NONE',  ( -0.000000000000000000, 1.000000000000000000, -0.000000000000000000 ) ) ;
#103571 = ORIENTED_EDGE ( 'NONE', *, *, #23719, .T. ) ;
#103572 = DIRECTION ( 'NONE',  ( 0.000000000000000000, 1.000000000000000000, 0.000000000000000000 ) ) ;
#103574 = EDGE_LOOP ( 'NONE', ( #34366, #77587 ) ) ;
#103573 = VERTEX_POINT ( 'NONE', #107490 ) ;
#103575 = ORIENTED_EDGE ( 'NONE', *, *, #43683, .T. ) ;
#103576 = DIRECTION ( 'NONE',  ( -0.000000000000000000, -1.000000000000000000, -0.000000000000000000 ) ) ;
#103577 = AXIS2_PLACEMENT_3D ( 'NONE', #116097, #126572, #95814 ) ;
#103578 = VECTOR ( 'NONE', #51524, 1000.000000000000000 ) ;
#103579 = DIRECTION ( 'NONE',  ( 0.000000000000000000, 1.000000000000000000, 0.000000000000000000 ) ) ;
#103580 =( LENGTH_UNIT ( ) NAMED_UNIT ( * ) SI_UNIT ( .MILLI., .METRE. ) );
#103581 = CARTESIAN_POINT ( 'NONE',  ( 186.7916666666667140, 4.445597072760099522, -7.700000000000035705 ) ) ;
#103582 = DIRECTION ( 'NONE',  ( -0.000000000000000000, -1.000000000000000000, -0.000000000000000000 ) ) ;
#103583 = CARTESIAN_POINT ( 'NONE',  ( 4.599999999999940137, 2.500000000000000000, -5.022947341949754119 ) ) ;
#103584 = EDGE_CURVE ( 'NONE', #96634, #127530, #38242, .T. ) ;
#103585 = ORIENTED_EDGE ( 'NONE', *, *, #3499, .F. ) ;
#103586 = LINE ( 'NONE', #94386, #122945 ) ;
#103587 = VERTEX_POINT ( 'NONE', #69483 ) ;
#103588 = CIRCLE ( 'NONE', #72198, 0.06509327318403745899 ) ;
#103589 = ORIENTED_EDGE ( 'NONE', *, *, #28267, .T. ) ;
#103590 = ORIENTED_EDGE ( 'NONE', *, *, #34949, .T. ) ;
#103591 = VECTOR ( 'NONE', #120918, 1000.000000000000000 ) ;
#103592 = DIRECTION ( 'NONE',  ( -0.000000000000000000, 1.000000000000000000, -0.000000000000000000 ) ) ;
#103593 = EDGE_LOOP ( 'NONE', ( #30504, #24796 ) ) ;
#103594 = ORIENTED_EDGE ( 'NONE', *, *, #33628, .F. ) ;
#103595 = ORIENTED_EDGE ( 'NONE', *, *, #60657, .F. ) ;
#103596 = DIRECTION ( 'NONE',  ( -4.274815082592931898E-19, -0.9999939076577903929, -0.003490651415223739937 ) ) ;
#103598 = VECTOR ( 'NONE', #104164, 1000.000000000000000 ) ;
#103597 = DIRECTION ( 'NONE',  ( -0.000000000000000000, 1.000000000000000000, -0.000000000000000000 ) ) ;
#103599 = CARTESIAN_POINT ( 'NONE',  ( -5.600000000000020073, 12.50000000000000000, 3.983716857408420964 ) ) ;
#103600 = AXIS2_PLACEMENT_3D ( 'NONE', #103709, #54578, #95810 ) ;
#103601 = EDGE_CURVE ( 'NONE', #39180, #116552, #88373, .T. ) ;
#103602 = DIRECTION ( 'NONE',  ( 0.000000000000000000, 0.000000000000000000, 1.000000000000000000 ) ) ;
#103603 = CARTESIAN_POINT ( 'NONE',  ( -3.950000000000024603, 2.500000000000000000, 1.818653347947321475 ) ) ;
#103604 = CARTESIAN_POINT ( 'NONE',  ( -5.450000000000019718, 2.500000000000000000, 2.165063509461097713 ) ) ;
#103605 = DIRECTION ( 'NONE',  ( 0.000000000000000000, 0.000000000000000000, 1.000000000000000000 ) ) ;
#103606 = ORIENTED_EDGE ( 'NONE', *, *, #41947, .F. ) ;
#103607 = CARTESIAN_POINT ( 'NONE',  ( -1.250000000000001110, 12.50000000000000000, -2.165063509461101710 ) ) ;
#103608 = ORIENTED_EDGE ( 'NONE', *, *, #43823, .T. ) ;
#103609 = DIRECTION ( 'NONE',  ( 0.000000000000000000, 0.000000000000000000, -1.000000000000000000 ) ) ;
#103610 = CIRCLE ( 'NONE', #105659, 0.1000000000000002554 ) ;
#103611 = VERTEX_POINT ( 'NONE', #17804 ) ;
#103612 = ADVANCED_FACE ( 'NONE', ( #119236 ), #36188, .T. ) ;
#103613 = ORIENTED_EDGE ( 'NONE', *, *, #97812, .T. ) ;
#103614 = FACE_OUTER_BOUND ( 'NONE', #76438, .T. ) ;
#103615 = DIRECTION ( 'NONE',  ( -0.000000000000000000, 1.000000000000000000, -0.000000000000000000 ) ) ;
#103616 = CIRCLE ( 'NONE', #128766, 0.1000000000000002554 ) ;
#103618 = CARTESIAN_POINT ( 'NONE',  ( -3.550000000000031797, 2.500000000000000000, -6.148780366869526226 ) ) ;
#103617 = AXIS2_PLACEMENT_3D ( 'NONE', #74161, #83960, #96352 ) ;
#103619 = ORIENTED_EDGE ( 'NONE', *, *, #21654, .F. ) ;
#103620 = ORIENTED_EDGE ( 'NONE', *, *, #127743, .F. ) ;
#103621 = DIRECTION ( 'NONE',  ( -0.000000000000000000, 1.000000000000000000, -0.000000000000000000 ) ) ;
#103622 = DIRECTION ( 'NONE',  ( 0.000000000000000000, 0.000000000000000000, 1.000000000000000000 ) ) ;
#103623 = CARTESIAN_POINT ( 'NONE',  ( -2.700000000000031264, 2.500000000000000000, 4.776537180435972196 ) ) ;
#103624 = LINE ( 'NONE', #55803, #53443 ) ;
#103625 = AXIS2_PLACEMENT_3D ( 'NONE', #109383, #21001, #91037 ) ;
#103626 = CARTESIAN_POINT ( 'NONE',  ( -2.950000000000029932, 2.500000000000000000, 2.265063509461097357 ) ) ;
#103627 = ORIENTED_EDGE ( 'NONE', *, *, #91612, .T. ) ;
#103628 = AXIS2_PLACEMENT_3D ( 'NONE', #21205, #128619, #129262 ) ;
#103629 = EDGE_LOOP ( 'NONE', ( #103515, #37245, #95608, #21537, #73438 ) ) ;
#103630 = CIRCLE ( 'NONE', #26263, 0.09999999999999982514 ) ;
#103631 = CARTESIAN_POINT ( 'NONE',  ( -3.100000000000028511, 12.50000000000000000, -0.3464101615137782364 ) ) ;
#103633 = AXIS2_PLACEMENT_3D ( 'NONE', #114016, #1464, #91790 ) ;
#103632 = CARTESIAN_POINT ( 'NONE',  ( 17.49862860983167323, 2.500000000000000000, -4.081131818001370704 ) ) ;
#103635 = EDGE_CURVE ( 'NONE', #7958, #94775, #88479, .T. ) ;
#103634 = VECTOR ( 'NONE', #87292, 1000.000000000000000 ) ;
#103636 = AXIS2_PLACEMENT_3D ( 'NONE', #122464, #9917, #10543 ) ;
#103637 = CARTESIAN_POINT ( 'NONE',  ( 184.5468750003414300, -8.734944146203032389, -1.604583208406768146E-15 ) ) ;
#103638 = CARTESIAN_POINT ( 'NONE',  ( 2.049999999999948308, 2.500000000000000000, 6.595190528383296780 ) ) ;
#103639 = FACE_OUTER_BOUND ( 'NONE', #107729, .T. ) ;
#103640 = CARTESIAN_POINT ( 'NONE',  ( 2.949999999999943334, 2.500000000000000000, 6.395190528383296602 ) ) ;
#103641 = CARTESIAN_POINT ( 'NONE',  ( 1.249999999999953815, 2.500000000000000000, 1.572243186433545548 ) ) ;
#103642 = ORIENTED_EDGE ( 'NONE', *, *, #16995, .F. ) ;
#103643 = ADVANCED_FACE ( 'NONE', ( #87829 ), #94646, .T. ) ;
#103644 = CARTESIAN_POINT ( 'NONE',  ( 1.849999999999950573, 12.50000000000000000, -1.818653347947326138 ) ) ;
#103645 = DIRECTION ( 'NONE',  ( 0.000000000000000000, 0.000000000000000000, 1.000000000000000000 ) ) ;
#103646 = DIRECTION ( 'NONE',  ( 0.000000000000000000, 0.000000000000000000, -1.000000000000000000 ) ) ;
#103647 = VERTEX_POINT ( 'NONE', #119885 ) ;
#103648 = EDGE_CURVE ( 'NONE', #37147, #2544, #71677, .T. ) ;
#103649 = EDGE_CURVE ( 'NONE', #105928, #19953, #82148, .T. ) ;
#103650 = EDGE_CURVE ( 'NONE', #7926, #62375, #77925, .T. ) ;
#103651 = EDGE_CURVE ( 'NONE', #97855, #3084, #110070, .T. ) ;
#103652 = CONICAL_SURFACE ( 'NONE', #95327, 0.1000000000000002554, 0.003490658503988666988 ) ;
#103653 = CARTESIAN_POINT ( 'NONE',  ( -8.100000000000013856, 12.50000000000000000, -0.3464101615137782364 ) ) ;
#103654 = ORIENTED_EDGE ( 'NONE', *, *, #5947, .F. ) ;
#103655 = ADVANCED_FACE ( 'NONE', ( #100254 ), #79336, .T. ) ;
#103656 = DIRECTION ( 'NONE',  ( -0.000000000000000000, -1.000000000000000000, -0.000000000000000000 ) ) ;
#103657 = EDGE_CURVE ( 'NONE', #17700, #15440, #109421, .T. ) ;
#103658 = VECTOR ( 'NONE', #111917, 1000.000000000000000 ) ;
#103659 = ORIENTED_EDGE ( 'NONE', *, *, #117835, .F. ) ;
#103660 = CARTESIAN_POINT ( 'NONE',  ( -7.900000000000011013, 2.500000000000000000, 4.330127018922196314 ) ) ;
#103661 = DIRECTION ( 'NONE',  ( -0.000000000000000000, -1.000000000000000000, -0.000000000000000000 ) ) ;
#103662 = EDGE_CURVE ( 'NONE', #37879, #35997, #47936, .T. ) ;
#103663 = CARTESIAN_POINT ( 'NONE',  ( 4.799999999999937650, 12.50000000000000000, -0.3464101615137782364 ) ) ;
#103664 = VECTOR ( 'NONE', #12549, 1000.000000000000000 ) ;
#103665 = AXIS2_PLACEMENT_3D ( 'NONE', #36241, #113494, #16563 ) ;
#103666 = ORIENTED_EDGE ( 'NONE', *, *, #16686, .F. ) ;
#103667 = EDGE_CURVE ( 'NONE', #31864, #71376, #127141, .T. ) ;
#103669 = EDGE_CURVE ( 'NONE', #122087, #25527, #111362, .T. ) ;
#103668 = DIRECTION ( 'NONE',  ( 0.000000000000000000, 1.000000000000000000, 0.000000000000000000 ) ) ;
#103670 = AXIS2_PLACEMENT_3D ( 'NONE', #127658, #17692, #56965 ) ;
#103671 = CARTESIAN_POINT ( 'NONE',  ( 186.7083333333333428, -4.445597072760135937, -7.699999999999966427 ) ) ;
#103672 = ADVANCED_FACE ( 'NONE', ( #18460 ), #115566, .T. ) ;
#103673 = ORIENTED_EDGE ( 'NONE', *, *, #103488, .F. ) ;
#103674 = CIRCLE ( 'NONE', #128738, 0.06509327318403745899 ) ;
#103675 = EDGE_LOOP ( 'NONE', ( #11720, #63374, #105963, #101135 ) ) ;
#103677 = AXIS2_PLACEMENT_3D ( 'NONE', #95329, #83587, #84204 ) ;
#103676 = VECTOR ( 'NONE', #87767, 1000.000000000000000 ) ;
#103678 = VERTEX_POINT ( 'NONE', #128442 ) ;
#103679 = DIRECTION ( 'NONE',  ( 0.000000000000000000, 0.000000000000000000, -1.000000000000000000 ) ) ;
#103680 = DIRECTION ( 'NONE',  ( 0.000000000000000000, 1.000000000000000000, 0.000000000000000000 ) ) ;
#103681 = FACE_OUTER_BOUND ( 'NONE', #87404, .T. ) ;
#103682 = ORIENTED_EDGE ( 'NONE', *, *, #53819, .T. ) ;
#103683 = CARTESIAN_POINT ( 'NONE',  ( 0.5999999999999621192, 2.500000000000000000, 0.3464101615137758494 ) ) ;
#103684 = DIRECTION ( 'NONE',  ( 0.000000000000000000, 0.000000000000000000, 1.000000000000000000 ) ) ;
#103685 = ORIENTED_EDGE ( 'NONE', *, *, #27506, .T. ) ;
#103686 = DIRECTION ( 'NONE',  ( 0.000000000000000000, 0.000000000000000000, 1.000000000000000000 ) ) ;
#103688 = LINE ( 'NONE', #112858, #124527 ) ;
#103687 = CONICAL_SURFACE ( 'NONE', #118056, 0.1000000000000000056, 0.003490658503988666988 ) ;
#103689 = CIRCLE ( 'NONE', #122472, 0.06509327318403745899 ) ;
#103690 = PLANE ( 'NONE',  #78021 ) ;
#103691 = DIRECTION ( 'NONE',  ( 0.000000000000000000, -0.000000000000000000, 1.000000000000000000 ) ) ;
#103692 = DIRECTION ( 'NONE',  ( 0.000000000000000000, 1.000000000000000000, 0.000000000000000000 ) ) ;
#103693 = DIRECTION ( 'NONE',  ( 0.000000000000000000, -0.000000000000000000, 1.000000000000000000 ) ) ;
#103694 = CARTESIAN_POINT ( 'NONE',  ( -8.150000000000012790, 2.500000000000000000, -1.818653347947326138 ) ) ;
#103695 = VERTEX_POINT ( 'NONE', #98956 ) ;
#103696 = ORIENTED_EDGE ( 'NONE', *, *, #48114, .T. ) ;
#103697 = EDGE_LOOP ( 'NONE', ( #74965, #12565, #112248, #31363 ) ) ;
#103698 = VERTEX_POINT ( 'NONE', #49235 ) ;
#103699 = CARTESIAN_POINT ( 'NONE',  ( 81.97061111377642817, 3.937853021265186548, 6.123961096679600757 ) ) ;
#103700 = DIRECTION ( 'NONE',  ( 0.000000000000000000, 0.000000000000000000, 1.000000000000000000 ) ) ;
#103701 = PLANE ( 'NONE',  #88646 ) ;
#103702 = VERTEX_POINT ( 'NONE', #89134 ) ;
#103703 = FACE_BOUND ( 'NONE', #9635, .T. ) ;
#103704 = DIRECTION ( 'NONE',  ( -0.000000000000000000, -1.000000000000000000, -0.000000000000000000 ) ) ;
#103705 = CARTESIAN_POINT ( 'NONE',  ( 3.949999999999941558, 2.500000000000000000, -1.818653347947326138 ) ) ;
#103706 = ADVANCED_FACE ( 'NONE', ( #129091 ), #11108, .T. ) ;
#103707 = DIRECTION ( 'NONE',  ( 0.000000000000000000, 0.000000000000000000, 1.000000000000000000 ) ) ;
#103708 = CIRCLE ( 'NONE', #18002, 0.1000000000000002554 ) ;
#103709 = CARTESIAN_POINT ( 'NONE',  ( 4.999999999999971578, 2.500000000000000000, -2.276824562219559311E-15 ) ) ;
#103710 = EDGE_CURVE ( 'NONE', #61453, #28873, #79957, .T. ) ;
#103711 = CARTESIAN_POINT ( 'NONE',  ( -7.300000000000016698, 2.500000000000000000, -4.776537180435978414 ) ) ;
#103712 = CARTESIAN_POINT ( 'NONE',  ( -11.24999999999996447, 2.500000000000000000, -6.595190528383298556 ) ) ;
#103714 = DIRECTION ( 'NONE',  ( 0.000000000000000000, 0.000000000000000000, 1.000000000000000000 ) ) ;
#103713 =( BOUNDED_CURVE ( )  B_SPLINE_CURVE ( 2, ( #52142, #81590, #112987, #31223, #42321, #41692, #33155 ),
 .UNSPECIFIED., .F., .F. ) 
 B_SPLINE_CURVE_WITH_KNOTS ( ( 3, 2, 2, 3 ),
 ( 0.2142857142857144681, 0.2380952380952383041, 0.2619047619047621955, 0.2857142857142859760 ),
 .UNSPECIFIED. ) 
 CURVE ( )  GEOMETRIC_REPRESENTATION_ITEM ( )  RATIONAL_B_SPLINE_CURVE ( ( 0.9999999999999988898, 0.8660254037844397068, 1.000000000000000000, 0.8660254037844387076, 1.000000000000000000, 0.8660254037844371533, 1.000000000000001554 ) ) 
 REPRESENTATION_ITEM ( '' )  );
#103715 = DIRECTION ( 'NONE',  ( 0.000000000000000000, -0.000000000000000000, 1.000000000000000000 ) ) ;
#103716 = DIRECTION ( 'NONE',  ( 0.000000000000000000, 0.000000000000000000, 1.000000000000000000 ) ) ;
#103718 = EDGE_CURVE ( 'NONE', #103899, #95311, #78029, .T. ) ;
#103717 = CARTESIAN_POINT ( 'NONE',  ( 4.999999999999936939, 2.500000000000000000, -3.737306695894649700 ) ) ;
#103721 = ORIENTED_EDGE ( 'NONE', *, *, #69245, .T. ) ;
#103720 = AXIS2_PLACEMENT_3D ( 'NONE', #28014, #107856, #16229 ) ;
#103719 = CONICAL_SURFACE ( 'NONE', #74755, 0.09999999999999982514, 0.003490658503988666988 ) ;
#103722 = ORIENTED_EDGE ( 'NONE', *, *, #16119, .T. ) ;
#103723 = ORIENTED_EDGE ( 'NONE', *, *, #10324, .F. ) ;
#103724 = VERTEX_POINT ( 'NONE', #100876 ) ;
#103725 = ORIENTED_EDGE ( 'NONE', *, *, #48303, .F. ) ;
#103726 = EDGE_LOOP ( 'NONE', ( #53045, #92423, #66399, #116698 ) ) ;
#103727 = DIRECTION ( 'NONE',  ( 0.000000000000000000, 0.000000000000000000, 1.000000000000000000 ) ) ;
#103728 = VERTEX_POINT ( 'NONE', #113277 ) ;
#103729 = VERTEX_POINT ( 'NONE', #103469 ) ;
#103730 = CIRCLE ( 'NONE', #109977, 0.06509327318403743123 ) ;
#103731 = CIRCLE ( 'NONE', #120441, 0.1000000000000000472 ) ;
#103732 = CARTESIAN_POINT ( 'NONE',  ( 12.65326442544191998, -1.500000000000190292, 8.428886915957789938 ) ) ;
#103733 = DIRECTION ( 'NONE',  ( -0.000000000000000000, 1.000000000000000000, -0.000000000000000000 ) ) ;
#103734 = CARTESIAN_POINT ( 'NONE',  ( -10.85000000000000142, 2.500000000000000000, -6.595190528383298556 ) ) ;
#103735 = EDGE_LOOP ( 'NONE', ( #56874, #27000, #62982, #107168 ) ) ;
#103736 = CARTESIAN_POINT ( 'NONE',  ( -3.150000000000032330, 2.500000000000000000, -6.248780366869526759 ) ) ;
#103737 = ORIENTED_EDGE ( 'NONE', *, *, #93369, .T. ) ;
#103738 = ORIENTED_EDGE ( 'NONE', *, *, #61463, .F. ) ;
#103740 = ORIENTED_EDGE ( 'NONE', *, *, #19265, .T. ) ;
#103739 = CARTESIAN_POINT ( 'NONE',  ( 9.149999999999916866, 2.500000000000000000, -1.472243186433550122 ) ) ;
#103741 = CARTESIAN_POINT ( 'NONE',  ( 12.49999999999990585, 2.500000000000000000, -5.022947341949754119 ) ) ;
#103742 = ORIENTED_EDGE ( 'NONE', *, *, #84427, .F. ) ;
#103743 = DIRECTION ( 'NONE',  ( 0.000000000000000000, 0.000000000000000000, 1.000000000000000000 ) ) ;
#103744 = CARTESIAN_POINT ( 'NONE',  ( 13.14999999999990088, 12.50000000000000000, 1.883746621131358934 ) ) ;
#103745 = FACE_OUTER_BOUND ( 'NONE', #123467, .T. ) ;
#103746 = AXIS2_PLACEMENT_3D ( 'NONE', #63184, #92642, #53373 ) ;
#103747 = DIRECTION ( 'NONE',  ( -0.000000000000000000, -1.000000000000000000, -0.000000000000000000 ) ) ;
#103748 = DIRECTION ( 'NONE',  ( 0.000000000000000000, 0.000000000000000000, 1.000000000000000000 ) ) ;
#103749 = CIRCLE ( 'NONE', #80773, 0.1000000000000002554 ) ;
#103750 = VECTOR ( 'NONE', #49618, 1000.000000000000000 ) ;
#103751 = EDGE_LOOP ( 'NONE', ( #57341, #76290 ) ) ;
#103752 = CARTESIAN_POINT ( 'NONE',  ( -8.350000000000008527, 12.50000000000000000, 7.122917578226811486 ) ) ;
#103753 = ORIENTED_EDGE ( 'NONE', *, *, #12046, .F. ) ;
#103754 = AXIS2_PLACEMENT_3D ( 'NONE', #123001, #83727, #123625 ) ;
#103755 = CARTESIAN_POINT ( 'NONE',  ( 17.50000000000000000, 2.500000000000000000, 3.333333333333334370 ) ) ;
#103756 = ORIENTED_EDGE ( 'NONE', *, *, #63740, .T. ) ;
#103757 = DIRECTION ( 'NONE',  ( -0.000000000000000000, 1.000000000000000000, -0.000000000000000000 ) ) ;
#103758 = DIRECTION ( 'NONE',  ( 0.000000000000000000, 0.000000000000000000, 1.000000000000000000 ) ) ;
#103759 = EDGE_CURVE ( 'NONE', #48774, #61216, #34125, .T. ) ;
#103760 = DIRECTION ( 'NONE',  ( 0.000000000000000000, 0.000000000000000000, -1.000000000000000000 ) ) ;
#103761 = EDGE_CURVE ( 'NONE', #17352, #63575, #13162, .T. ) ;
#103762 = CARTESIAN_POINT ( 'NONE',  ( 1.049999999999954969, 12.50000000000000000, -6.841600689897077814 ) ) ;
#103763 = VERTEX_POINT ( 'NONE', #123110 ) ;
#103764 = CIRCLE ( 'NONE', #112079, 0.06509327318403745899 ) ;
#103765 = DIRECTION ( 'NONE',  ( 0.000000000000000000, 0.000000000000000000, 1.000000000000000000 ) ) ;
#103767 = AXIS2_PLACEMENT_3D ( 'NONE', #41905, #92265, #43200 ) ;
#103766 = CONICAL_SURFACE ( 'NONE', #101713, 0.1000000000000002554, 0.003490658503988666988 ) ;
#103768 = DIRECTION ( 'NONE',  ( 0.000000000000000000, -0.9999939076577903929, 0.003490651415223739937 ) ) ;
#103769 = EDGE_LOOP ( 'NONE', ( #127966, #48217, #108281, #127750 ) ) ;
#103770 = VERTEX_POINT ( 'NONE', #61623 ) ;
#103772 = ORIENTED_EDGE ( 'NONE', *, *, #80756, .F. ) ;
#103771 = EDGE_CURVE ( 'NONE', #53022, #53628, #8965, .T. ) ;
#103773 = CARTESIAN_POINT ( 'NONE',  ( -9.550000000000007816, 2.500000000000000000, -6.395190528383296602 ) ) ;
#103774 = DIRECTION ( 'NONE',  ( 0.000000000000000000, 0.000000000000000000, 1.000000000000000000 ) ) ;
#103775 = CARTESIAN_POINT ( 'NONE',  ( 184.7343750003414016, 8.734944146203032389, 5.348610694689227483E-16 ) ) ;
#103776 = LINE ( 'NONE', #101196, #17724 ) ;
#103777 = CARTESIAN_POINT ( 'NONE',  ( 16.80072262464530652, 1.717570462274060850, -5.816823748342643263 ) ) ;
#103778 = DIRECTION ( 'NONE',  ( -0.000000000000000000, 1.000000000000000000, -0.000000000000000000 ) ) ;
#103779 = EDGE_LOOP ( 'NONE', ( #69686, #12256, #91176, #33283 ) ) ;
#103780 = CARTESIAN_POINT ( 'NONE',  ( 1.899999999999951283, 12.50000000000000000, 0.3464101615137736845 ) ) ;
#103781 = EDGE_CURVE ( 'NONE', #111163, #117766, #65407, .T. ) ;
#103782 = EDGE_LOOP ( 'NONE', ( #63614, #958 ) ) ;
#103783 = CARTESIAN_POINT ( 'NONE',  ( 0.6499999999999561684, 12.50000000000000000, 2.446380397790835826 ) ) ;
#103784 = LINE ( 'NONE', #84784, #3638 ) ;
#103785 = CARTESIAN_POINT ( 'NONE',  ( 5.849999999999933920, 12.50000000000000000, -2.230156782645139391 ) ) ;
#103786 = DIRECTION ( 'NONE',  ( 0.000000000000000000, -0.9999939076577903929, 0.003490651415223739937 ) ) ;
#103787 = EDGE_LOOP ( 'NONE', ( #114948, #92075, #42463, #69737 ) ) ;
#103788 = EDGE_CURVE ( 'NONE', #34917, #44517, #2707, .T. ) ;
#103789 = AXIS2_PLACEMENT_3D ( 'NONE', #6505, #28778, #68684 ) ;
#103790 = CARTESIAN_POINT ( 'NONE',  ( 10.64999999999990976, 2.500000000000000000, 1.718653347947321386 ) ) ;
#103792 = ORIENTED_EDGE ( 'NONE', *, *, #492, .T. ) ;
#103791 = CARTESIAN_POINT ( 'NONE',  ( 10.59999999999990905, 2.500000000000000000, 3.883716857408420431 ) ) ;
#103793 = ADVANCED_FACE ( 'NONE', ( #121809 ), #60955, .T. ) ;
#103794 = ADVANCED_FACE ( 'NONE', ( #81255 ), #52990, .T. ) ;
#103795 = EDGE_CURVE ( 'NONE', #52298, #99291, #32077, .T. ) ;
#103796 = EDGE_CURVE ( 'NONE', #94042, #10496, #15315, .T. ) ;
#103797 = ORIENTED_EDGE ( 'NONE', *, *, #26968, .F. ) ;
#103799 = AXIS2_PLACEMENT_3D ( 'NONE', #46201, #88536, #126042 ) ;
#103798 = AXIS2_PLACEMENT_3D ( 'NONE', #80625, #81263, #20409 ) ;
#103800 = DIRECTION ( 'NONE',  ( 0.000000000000000000, 0.000000000000000000, 1.000000000000000000 ) ) ;
#103801 = VERTEX_POINT ( 'NONE', #745 ) ;
#103802 = ORIENTED_EDGE ( 'NONE', *, *, #73347, .F. ) ;
#103803 = DIRECTION ( 'NONE',  ( 0.000000000000000000, 1.000000000000000000, 0.000000000000000000 ) ) ;
#103804 = EDGE_CURVE ( 'NONE', #17144, #114482, #102184, .T. ) ;
#103805 = ADVANCED_FACE ( 'NONE', ( #91713 ), #34229, .T. ) ;
#103806 = ORIENTED_EDGE ( 'NONE', *, *, #8818, .T. ) ;
#103807 = DIRECTION ( 'NONE',  ( -0.000000000000000000, -1.000000000000000000, -0.000000000000000000 ) ) ;
#103808 = LINE ( 'NONE', #63881, #46395 ) ;
#103809 = VECTOR ( 'NONE', #94, 1000.000000000000000 ) ;
#103810 = DIRECTION ( 'NONE',  ( 0.000000000000000000, 0.000000000000000000, 1.000000000000000000 ) ) ;
#103811 = VERTEX_POINT ( 'NONE', #63551 ) ;
#103812 = EDGE_CURVE ( 'NONE', #89734, #59250, #40496, .T. ) ;
#103813 = CIRCLE ( 'NONE', #26458, 0.09999999999999982514 ) ;
#103814 = EDGE_CURVE ( 'NONE', #36682, #29463, #42639, .T. ) ;
#103815 = DIRECTION ( 'NONE',  ( -4.274815082592931898E-19, -0.9999939076577903929, -0.003490651415223739937 ) ) ;
#103817 = EDGE_LOOP ( 'NONE', ( #27733, #125457 ) ) ;
#103816 = DIRECTION ( 'NONE',  ( -0.000000000000000000, 1.000000000000000000, -0.000000000000000000 ) ) ;
#103818 = CARTESIAN_POINT ( 'NONE',  ( 9.149999999999918643, 12.50000000000000000, 2.165063509461097713 ) ) ;
#103819 = EDGE_CURVE ( 'NONE', #78788, #44264, #9072, .T. ) ;
#103820 = CARTESIAN_POINT ( 'NONE',  ( 3.549999999999942979, 12.50000000000000000, 1.753560074763284016 ) ) ;
#103821 = EDGE_CURVE ( 'NONE', #94166, #118365, #128220, .T. ) ;
#103822 = ORIENTED_EDGE ( 'NONE', *, *, #57259, .T. ) ;
#103823 = ORIENTED_EDGE ( 'NONE', *, *, #104839, .T. ) ;
#103824 = ORIENTED_EDGE ( 'NONE', *, *, #17653, .T. ) ;
#103825 = VERTEX_POINT ( 'NONE', #93013 ) ;
#103826 = CARTESIAN_POINT ( 'NONE',  ( 9.599999999999917932, 12.50000000000000000, -0.7579135962115916003 ) ) ;
#103827 = DIRECTION ( 'NONE',  ( -0.000000000000000000, -1.000000000000000000, -0.000000000000000000 ) ) ;
#103828 = FACE_OUTER_BOUND ( 'NONE', #65557, .T. ) ;
#103829 = FACE_BOUND ( 'NONE', #23964, .T. ) ;
#103830 = ORIENTED_EDGE ( 'NONE', *, *, #72381, .T. ) ;
#103831 = CIRCLE ( 'NONE', #95511, 0.09999999999999982514 ) ;
#103832 = CARTESIAN_POINT ( 'NONE',  ( 184.7760416670080588, 6.551208109652274736, 3.782341765625001351 ) ) ;
#103833 = PLANE ( 'NONE',  #84530 ) ;
#103834 = DIRECTION ( 'NONE',  ( -0.000000000000000000, -1.000000000000000000, -0.000000000000000000 ) ) ;
#103835 = CONICAL_SURFACE ( 'NONE', #127114, 0.1000000000000002554, 0.003490658503988666988 ) ;
#103836 = AXIS2_PLACEMENT_3D ( 'NONE', #85452, #96544, #6865 ) ;
#103837 = DIRECTION ( 'NONE',  ( -0.000000000000000000, 1.000000000000000000, -0.000000000000000000 ) ) ;
#103838 = CARTESIAN_POINT ( 'NONE',  ( 2.699999999999947331, 12.50000000000000000, -4.676537180435978769 ) ) ;
#103839 = FACE_OUTER_BOUND ( 'NONE', #12857, .T. ) ;
#103840 = AXIS2_PLACEMENT_3D ( 'NONE', #28521, #18036, #96588 ) ;
#103841 = AXIS2_PLACEMENT_3D ( 'NONE', #14473, #7724, #53775 ) ;
#103842 = LINE ( 'NONE', #14149, #72510 ) ;
#103843 = CIRCLE ( 'NONE', #47417, 0.1000000000000002554 ) ;
#103844 = EDGE_LOOP ( 'NONE', ( #26362, #72312 ) ) ;
#103845 = ORIENTED_EDGE ( 'NONE', *, *, #103067, .F. ) ;
#103846 = VERTEX_POINT ( 'NONE', #3333 ) ;
#103847 = ORIENTED_EDGE ( 'NONE', *, *, #77926, .F. ) ;
#103848 = ORIENTED_EDGE ( 'NONE', *, *, #77593, .F. ) ;
#103849 = DIRECTION ( 'NONE',  ( -0.000000000000000000, 1.000000000000000000, -0.000000000000000000 ) ) ;
#103850 = CARTESIAN_POINT ( 'NONE',  ( 6.049999999999934097, 12.50000000000000000, -6.148780366869526226 ) ) ;
#103851 = AXIS2_PLACEMENT_3D ( 'NONE', #121104, #53019, #82487 ) ;
#103852 = ORIENTED_EDGE ( 'NONE', *, *, #104849, .T. ) ;
#103853 = FACE_BOUND ( 'NONE', #3119, .T. ) ;
#103855 = DIRECTION ( 'NONE',  ( 0.000000000000000000, 0.000000000000000000, 1.000000000000000000 ) ) ;
#103854 = CIRCLE ( 'NONE', #49493, 0.09999999999999982514 ) ;
#103856 = ADVANCED_FACE ( 'NONE', ( #33455 ), #46736, .T. ) ;
#103858 = AXIS2_PLACEMENT_3D ( 'NONE', #81174, #12417, #112574 ) ;
#103857 = CONICAL_SURFACE ( 'NONE', #47428, 0.1000000000000000056, 0.003490658503988666988 ) ;
#103859 = ADVANCED_FACE ( 'NONE', ( #54361 ), #27947, .T. ) ;
#103860 = ORIENTED_EDGE ( 'NONE', *, *, #14812, .F. ) ;
#103861 = DIRECTION ( 'NONE',  ( 0.000000000000000000, 1.000000000000000000, 0.000000000000000000 ) ) ;
#103862 = FACE_OUTER_BOUND ( 'NONE', #31306, .T. ) ;
#103863 = CARTESIAN_POINT ( 'NONE',  ( 9.149999999999920419, 12.50000000000000000, -7.188010851410854052 ) ) ;
#103864 = VERTEX_POINT ( 'NONE', #65463 ) ;
#103865 = FACE_OUTER_BOUND ( 'NONE', #37981, .T. ) ;
#103866 = ORIENTED_EDGE ( 'NONE', *, *, #129554, .T. ) ;
#103867 = EDGE_LOOP ( 'NONE', ( #49654, #85071 ) ) ;
#103868 = VERTEX_POINT ( 'NONE', #105403 ) ;
#103869 = DIRECTION ( 'NONE',  ( -0.000000000000000000, 1.000000000000000000, -0.000000000000000000 ) ) ;
#103870 = DIRECTION ( 'NONE',  ( -0.000000000000000000, -1.000000000000000000, -0.000000000000000000 ) ) ;
#103871 = CARTESIAN_POINT ( 'NONE',  ( 1.849999999999949685, 2.500000000000000000, -2.511473670974877948 ) ) ;
#103872 = EDGE_LOOP ( 'NONE', ( #70983, #128048 ) ) ;
#103873 = AXIS2_PLACEMENT_3D ( 'NONE', #20159, #54761, #103879 ) ;
#103874 = DIRECTION ( 'NONE',  ( -0.000000000000000000, -1.000000000000000000, -0.000000000000000000 ) ) ;
#103875 = LINE ( 'NONE', #14181, #57463 ) ;
#103876 = CARTESIAN_POINT ( 'NONE',  ( 13.09999999999990195, 2.500000000000000000, -3.983716857408426293 ) ) ;
#103877 = CARTESIAN_POINT ( 'NONE',  ( 185.6145833340161175, 6.668395609140177704, -3.849999999999998312 ) ) ;
#103878 = ORIENTED_EDGE ( 'NONE', *, *, #85142, .T. ) ;
#103879 = DIRECTION ( 'NONE',  ( 0.000000000000000000, -0.000000000000000000, 1.000000000000000000 ) ) ;
#103880 = ORIENTED_EDGE ( 'NONE', *, *, #41797, .T. ) ;
#103881 = FACE_OUTER_BOUND ( 'NONE', #52951, .T. ) ;
#103882 = AXIS2_PLACEMENT_3D ( 'NONE', #25457, #124973, #74580 ) ;
#103883 = ORIENTED_EDGE ( 'NONE', *, *, #100734, .T. ) ;
#103884 = CIRCLE ( 'NONE', #24461, 0.06509327318403741736 ) ;
#103885 = ORIENTED_EDGE ( 'NONE', *, *, #74940, .F. ) ;
#103886 = CARTESIAN_POINT ( 'NONE',  ( -14.34999999999998543, 12.50000000000000000, 2.511473670974877503 ) ) ;
#103887 = DIRECTION ( 'NONE',  ( -0.000000000000000000, -1.000000000000000000, -0.000000000000000000 ) ) ;
#103888 = PLANE ( 'NONE',  #38399 ) ;
#103889 = CARTESIAN_POINT ( 'NONE',  ( -0.4500000000000402012, 2.500000000000000000, 2.265063509461097357 ) ) ;
#103890 = CARTESIAN_POINT ( 'NONE',  ( 6.899999999999926636, 2.500000000000000000, -0.2464101615137782308 ) ) ;
#103891 = EDGE_LOOP ( 'NONE', ( #124161, #46787, #53132, #71691 ) ) ;
#103894 = EDGE_LOOP ( 'NONE', ( #127054, #31121, #48332, #34883 ) ) ;
#103893 = VECTOR ( 'NONE', #71471, 1000.000000000000000 ) ;
#103892 = AXIS2_PLACEMENT_3D ( 'NONE', #12506, #13137, #52435 ) ;
#103895 = ADVANCED_FACE ( 'NONE', ( #96205 ), #61420, .T. ) ;
#103896 = DIRECTION ( 'NONE',  ( 1.000000000000000000, 0.000000000000000000, 0.000000000000000000 ) ) ;
#103897 = CARTESIAN_POINT ( 'NONE',  ( -5.850000000000021849, 12.50000000000000000, -7.188010851410854052 ) ) ;
#103898 = CARTESIAN_POINT ( 'NONE',  ( 7.499999999999927169, 2.500000000000000000, -4.922947341949753586 ) ) ;
#103899 = VERTEX_POINT ( 'NONE', #26841 ) ;
#103900 = ORIENTED_EDGE ( 'NONE', *, *, #31854, .F. ) ;
#103901 = DIRECTION ( 'NONE',  ( -0.000000000000000000, 1.000000000000000000, -0.000000000000000000 ) ) ;
#103903 = AXIS2_PLACEMENT_3D ( 'NONE', #37980, #108007, #126368 ) ;
#103902 = CIRCLE ( 'NONE', #83076, 0.06509327318403745899 ) ;
#103904 = ORIENTED_EDGE ( 'NONE', *, *, #49126, .F. ) ;
#103905 = DIRECTION ( 'NONE',  ( 0.000000000000000000, 0.000000000000000000, 1.000000000000000000 ) ) ;
#103906 = AXIS2_PLACEMENT_3D ( 'NONE', #10763, #70363, #122051 ) ;
#103907 = CARTESIAN_POINT ( 'NONE',  ( -7.700000000000016165, 2.500000000000000000, -3.883716857408426648 ) ) ;
#103908 = ORIENTED_EDGE ( 'NONE', *, *, #54890, .F. ) ;
#103909 = DIRECTION ( 'NONE',  ( 0.000000000000000000, -0.000000000000000000, 1.000000000000000000 ) ) ;
#103910 = PLANE ( 'NONE',  #83879 ) ;
#103911 = LINE ( 'NONE', #33257, #80263 ) ;
#103912 = EDGE_CURVE ( 'NONE', #99741, #16266, #45202, .T. ) ;
#103913 = EDGE_CURVE ( 'NONE', #17273, #88432, #750, .T. ) ;
#103914 = DIRECTION ( 'NONE',  ( 0.000000000000000000, 1.000000000000000000, 0.000000000000000000 ) ) ;
#103915 = ORIENTED_EDGE ( 'NONE', *, *, #30986, .F. ) ;
#103916 = LINE ( 'NONE', #5694, #2755 ) ;
#103917 = DIRECTION ( 'NONE',  ( 0.000000000000000000, 1.000000000000000000, 0.000000000000000000 ) ) ;
#103918 = ORIENTED_EDGE ( 'NONE', *, *, #51119, .T. ) ;
#103919 = ORIENTED_EDGE ( 'NONE', *, *, #66828, .F. ) ;
#103920 = EDGE_CURVE ( 'NONE', #45883, #117091, #15710, .T. ) ;
#103921 = CARTESIAN_POINT ( 'NONE',  ( 186.8802083336747444, 4.367472073101515306, 7.564683531250000925 ) ) ;
#103922 = DIRECTION ( 'NONE',  ( 0.000000000000000000, 1.000000000000000000, 0.000000000000000000 ) ) ;
#103923 = CARTESIAN_POINT ( 'NONE',  ( 1.849999999999948130, 2.500000000000000000, 6.148780366869520009 ) ) ;
#103924 = AXIS2_PLACEMENT_3D ( 'NONE', #21613, #73929, #121095 ) ;
#103926 = AXIS2_PLACEMENT_3D ( 'NONE', #90491, #81344, #2113 ) ;
#103925 = DIRECTION ( 'NONE',  ( 0.000000000000000000, 0.000000000000000000, 1.000000000000000000 ) ) ;
#103927 = PLANE ( 'NONE',  #46451 ) ;
#103928 = CARTESIAN_POINT ( 'NONE',  ( 5.199999999999937117, 12.50000000000000000, -4.676537180435978769 ) ) ;
#103929 = AXIS2_PLACEMENT_3D ( 'NONE', #65657, #66303, #64369 ) ;
#103930 = DIRECTION ( 'NONE',  ( 0.000000000000000000, -1.000000000000000000, 0.000000000000000000 ) ) ;
#103931 = CARTESIAN_POINT ( 'NONE',  ( 0.000000000000000000, 0.000000000000000000, -5.000000000000004441 ) ) ;
#103932 = PLANE ( 'NONE',  #125119 ) ;
#103933 = DIRECTION ( 'NONE',  ( 0.000000000000000000, 1.000000000000000000, 0.000000000000000000 ) ) ;
#103934 = AXIS2_PLACEMENT_3D ( 'NONE', #61857, #14012, #93886 ) ;
#103935 = CIRCLE ( 'NONE', #97666, 0.06509327318403745899 ) ;
#103936 = DIRECTION ( 'NONE',  ( 0.000000000000000000, 0.000000000000000000, 1.000000000000000000 ) ) ;
#103937 = ORIENTED_EDGE ( 'NONE', *, *, #66003, .F. ) ;
#103938 = ORIENTED_EDGE ( 'NONE', *, *, #1285, .T. ) ;
#103939 = ORIENTED_EDGE ( 'NONE', *, *, #120108, .T. ) ;
#103940 = ORIENTED_EDGE ( 'NONE', *, *, #73035, .T. ) ;
#103941 = VECTOR ( 'NONE', #12904, 1000.000000000000000 ) ;
#103942 = DIRECTION ( 'NONE',  ( 0.000000000000000000, 0.000000000000000000, -1.000000000000000000 ) ) ;
#103943 = CARTESIAN_POINT ( 'NONE',  ( 13.74999999999989875, 12.50000000000000000, 1.407149913249508000 ) ) ;
#103944 = EDGE_LOOP ( 'NONE', ( #116564, #129044, #116610, #120755 ) ) ;
#103945 = DIRECTION ( 'NONE',  ( -0.000000000000000000, -1.000000000000000000, -0.000000000000000000 ) ) ;
#103946 = ADVANCED_FACE ( 'NONE', ( #34091 ), #4940, .T. ) ;
#103948 = AXIS2_PLACEMENT_3D ( 'NONE', #24668, #11614, #1782 ) ;
#103947 = VECTOR ( 'NONE', #117393, 1000.000000000000000 ) ;
#103949 = DIRECTION ( 'NONE',  ( 0.000000000000000000, -0.000000000000000000, 1.000000000000000000 ) ) ;
#103951 = EDGE_LOOP ( 'NONE', ( #68209, #31843, #85682, #98509 ) ) ;
#103950 = DIRECTION ( 'NONE',  ( 0.000000000000000000, 0.000000000000000000, -1.000000000000000000 ) ) ;
#103952 = EDGE_CURVE ( 'NONE', #120269, #35997, #78136, .T. ) ;
#103953 = DIRECTION ( 'NONE',  ( 0.000000000000000000, -0.9999939076577903929, 0.003490651415223739937 ) ) ;
#103954 = ADVANCED_FACE ( 'NONE', ( #86392 ), #103160, .T. ) ;
#103955 = DIRECTION ( 'NONE',  ( -0.000000000000000000, -1.000000000000000000, -0.000000000000000000 ) ) ;
#103956 = VERTEX_POINT ( 'NONE', #55652 ) ;
#103957 = ORIENTED_EDGE ( 'NONE', *, *, #44533, .T. ) ;
#103958 = ORIENTED_EDGE ( 'NONE', *, *, #61655, .F. ) ;
#103959 = VERTEX_POINT ( 'NONE', #113936 ) ;
#103960 = LINE ( 'NONE', #96062, #120079 ) ;
#103961 = EDGE_CURVE ( 'NONE', #75979, #126609, #82241, .T. ) ;
#103962 = ADVANCED_FACE ( 'NONE', ( #13782 ), #119889, .T. ) ;
#103963 = EDGE_CURVE ( 'NONE', #45554, #52604, #94844, .T. ) ;
#103964 = AXIS2_PLACEMENT_3D ( 'NONE', #59068, #98985, #6700 ) ;
#103965 = EDGE_CURVE ( 'NONE', #7114, #9353, #42545, .T. ) ;
#103966 = DIRECTION ( 'NONE',  ( 0.000000000000000000, 1.000000000000000000, 0.000000000000000000 ) ) ;
#103967 = DIRECTION ( 'NONE',  ( 0.000000000000000000, -0.000000000000000000, 1.000000000000000000 ) ) ;
#103968 = CARTESIAN_POINT ( 'NONE',  ( 4.199999999999939782, 2.500000000000000000, -0.1000000000000022815 ) ) ;
#103969 = ORIENTED_EDGE ( 'NONE', *, *, #123421, .T. ) ;
#103970 = EDGE_CURVE ( 'NONE', #45836, #60832, #113627, .T. ) ;
#103971 = DIRECTION ( 'NONE',  ( 0.000000000000000000, 0.000000000000000000, 1.000000000000000000 ) ) ;
#103972 = ORIENTED_EDGE ( 'NONE', *, *, #49808, .T. ) ;
#103973 = CARTESIAN_POINT ( 'NONE',  ( -0.2000000000000408673, 12.50000000000000000, -4.048810130592463530 ) ) ;
#103974 = CARTESIAN_POINT ( 'NONE',  ( 12.06068301313226598, -2.499999999999744649, -8.632776999392650197 ) ) ;
#103975 = LINE ( 'NONE', #83688, #83999 ) ;
#103976 = CARTESIAN_POINT ( 'NONE',  ( -5.450000000000023270, 2.500000000000000000, -6.595190528383302109 ) ) ;
#103977 = ADVANCED_FACE ( 'NONE', ( #114561 ), #24904, .T. ) ;
#103978 = VERTEX_POINT ( 'NONE', #5252 ) ;
#103979 = AXIS2_PLACEMENT_3D ( 'NONE', #64603, #114978, #25305 ) ;
#103980 = AXIS2_PLACEMENT_3D ( 'NONE', #34267, #65634, #25711 ) ;
#103981 = ORIENTED_EDGE ( 'NONE', *, *, #118769, .T. ) ;
#103982 = ORIENTED_EDGE ( 'NONE', *, *, #18128, .F. ) ;
#103983 = FACE_OUTER_BOUND ( 'NONE', #67680, .T. ) ;
#103984 = DIRECTION ( 'NONE',  ( 0.000000000000000000, 0.000000000000000000, -1.000000000000000000 ) ) ;
#103985 = LINE ( 'NONE', #83063, #106680 ) ;
#103986 = FACE_BOUND ( 'NONE', #68721, .T. ) ;
#103987 = DIRECTION ( 'NONE',  ( 0.000000000000000000, -0.9999939076577903929, 0.003490651415223739937 ) ) ;
#103988 = DIRECTION ( 'NONE',  ( 0.000000000000000000, -0.9999939076577903929, 0.003490651415223739937 ) ) ;
#103990 = AXIS2_PLACEMENT_3D ( 'NONE', #124880, #66591, #26677 ) ;
#103989 = CIRCLE ( 'NONE', #66317, 0.1000000000000000472 ) ;
#103991 = DIRECTION ( 'NONE',  ( 0.000000000000000000, -0.000000000000000000, 1.000000000000000000 ) ) ;
#103992 = CIRCLE ( 'NONE', #81001, 0.09999999999999999167 ) ;
#103993 = CARTESIAN_POINT ( 'NONE',  ( 187.0885416670080872, -6.551208109652273848, -3.782341765625003571 ) ) ;
#103994 = DIRECTION ( 'NONE',  ( 0.000000000000000000, 0.000000000000000000, 1.000000000000000000 ) ) ;
#103995 = DIRECTION ( 'NONE',  ( -0.000000000000000000, -1.000000000000000000, -0.000000000000000000 ) ) ;
#103996 = VERTEX_POINT ( 'NONE', #125033 ) ;
#103997 = VECTOR ( 'NONE', #101704, 1000.000000000000000 ) ;
#103998 = DIRECTION ( 'NONE',  ( 0.000000000000000000, 1.000000000000000000, 0.000000000000000000 ) ) ;
#103999 = EDGE_LOOP ( 'NONE', ( #61148, #5986, #11336, #2520 ) ) ;
#104000 = ORIENTED_EDGE ( 'NONE', *, *, #66414, .T. ) ;
#104001 = ORIENTED_EDGE ( 'NONE', *, *, #73114, .F. ) ;
#104002 = EDGE_LOOP ( 'NONE', ( #112897, #89536, #117602, #30081 ) ) ;
#104003 = DIRECTION ( 'NONE',  ( 0.000000000000000000, 0.000000000000000000, -1.000000000000000000 ) ) ;
#104004 = FACE_BOUND ( 'NONE', #105005, .T. ) ;
#104005 = CARTESIAN_POINT ( 'NONE',  ( -8.950000000000009948, 12.50000000000000000, -1.883746621131363597 ) ) ;
#104006 = AXIS2_PLACEMENT_3D ( 'NONE', #42215, #122065, #61202 ) ;
#104007 = EDGE_CURVE ( 'NONE', #121634, #39004, #121949, .T. ) ;
#104008 = AXIS2_PLACEMENT_3D ( 'NONE', #21439, #28207, #68117 ) ;
#104009 = ORIENTED_EDGE ( 'NONE', *, *, #94437, .T. ) ;
#104010 = CARTESIAN_POINT ( 'NONE',  ( 1.249999999999986899, 2.500000000000000000, 6.395190528383296602 ) ) ;
#104011 = PLANE ( 'NONE',  #106289 ) ;
#104012 = CIRCLE ( 'NONE', #35071, 0.06509327318403745899 ) ;
#104013 = ORIENTED_EDGE ( 'NONE', *, *, #41562, .T. ) ;
#104014 = FACE_OUTER_BOUND ( 'NONE', #117019, .T. ) ;
#104015 = CIRCLE ( 'NONE', #30875, 0.09999999999999982514 ) ;
#104016 = DIRECTION ( 'NONE',  ( 0.000000000000000000, 1.000000000000000000, 0.000000000000000000 ) ) ;
#104017 = ADVANCED_FACE ( 'NONE', ( #25529 ), #94749, .T. ) ;
#104018 = VECTOR ( 'NONE', #36360, 1000.000000000000000 ) ;
#104019 = ORIENTED_EDGE ( 'NONE', *, *, #48959, .F. ) ;
#104020 = CARTESIAN_POINT ( 'NONE',  ( -0.4500000000000402012, 12.50000000000000000, 2.099970236277060032 ) ) ;
#104021 = CARTESIAN_POINT ( 'NONE',  ( 179.5000000000000000, 0.6250000000000003331, 6.000000000000000000 ) ) ;
#104022 = AXIS2_PLACEMENT_3D ( 'NONE', #57831, #97741, #8069 ) ;
#104023 = CIRCLE ( 'NONE', #26663, 0.06509327318403745899 ) ;
#104024 = ORIENTED_EDGE ( 'NONE', *, *, #62616, .F. ) ;
#104025 = AXIS2_PLACEMENT_3D ( 'NONE', #106019, #25501, #53693 ) ;
#104026 = VECTOR ( 'NONE', #54229, 1000.000000000000000 ) ;
#104027 = CARTESIAN_POINT ( 'NONE',  ( -1.450000000000036371, 2.500000000000000000, 2.411473670974873862 ) ) ;
#104028 = DIRECTION ( 'NONE',  ( 0.000000000000000000, 1.000000000000000000, 0.000000000000000000 ) ) ;
#104029 = CARTESIAN_POINT ( 'NONE',  ( -4.350000000000023626, 2.500000000000000000, 6.048780366869521252 ) ) ;
#104030 = ORIENTED_EDGE ( 'NONE', *, *, #26652, .T. ) ;
#104031 = VERTEX_POINT ( 'NONE', #98789 ) ;
#104032 = CIRCLE ( 'NONE', #70583, 0.1000000000000000472 ) ;
#104033 = CARTESIAN_POINT ( 'NONE',  ( 14.19999999999989626, 12.50000000000000000, 0.06509327318403515528 ) ) ;
#104034 = ORIENTED_EDGE ( 'NONE', *, *, #3289, .F. ) ;
#104035 = DIRECTION ( 'NONE',  ( -0.000000000000000000, -1.000000000000000000, -0.000000000000000000 ) ) ;
#104036 = DIRECTION ( 'NONE',  ( 0.000000000000000000, 0.000000000000000000, 1.000000000000000000 ) ) ;
#104038 = CIRCLE ( 'NONE', #24619, 0.09999999999999982514 ) ;
#104037 = CIRCLE ( 'NONE', #37149, 0.1000000000000000472 ) ;
#104039 = EDGE_LOOP ( 'NONE', ( #105023, #52831 ) ) ;
#104040 = CARTESIAN_POINT ( 'NONE',  ( -11.05000000000000071, 12.50000000000000000, 2.576566944158910744 ) ) ;
#104041 = CARTESIAN_POINT ( 'NONE',  ( -1.322875655532295136, -2.500000000000000444, 6.000000000000005329 ) ) ;
#104042 = FACE_OUTER_BOUND ( 'NONE', #62491, .T. ) ;
#104043 = DIRECTION ( 'NONE',  ( 0.000000000000000000, 1.000000000000000000, 0.000000000000000000 ) ) ;
#104044 = DIRECTION ( 'NONE',  ( 0.000000000000000000, 0.000000000000000000, -1.000000000000000000 ) ) ;
#104045 = ORIENTED_EDGE ( 'NONE', *, *, #12843, .F. ) ;
#104047 = ORIENTED_EDGE ( 'NONE', *, *, #24616, .T. ) ;
#104046 = ADVANCED_FACE ( 'NONE', ( #58250 ), #78541, .T. ) ;
#104048 = CARTESIAN_POINT ( 'NONE',  ( 2.299999999999949640, 2.500000000000000000, -4.676537180435977881 ) ) ;
#104049 = DIRECTION ( 'NONE',  ( 0.000000000000000000, 1.000000000000000000, 0.000000000000000000 ) ) ;
#104050 = DIRECTION ( 'NONE',  ( -4.274815082592931898E-19, -0.9999939076577903929, -0.003490651415223739937 ) ) ;
#104052 = ORIENTED_EDGE ( 'NONE', *, *, #128163, .F. ) ;
#104051 = ORIENTED_EDGE ( 'NONE', *, *, #101920, .T. ) ;
#104053 = ORIENTED_EDGE ( 'NONE', *, *, #115306, .T. ) ;
#104054 = DIRECTION ( 'NONE',  ( -0.000000000000000000, -1.000000000000000000, -0.000000000000000000 ) ) ;
#104056 = EDGE_CURVE ( 'NONE', #80982, #82263, #107899, .T. ) ;
#104055 = CARTESIAN_POINT ( 'NONE',  ( 9.149999999999916866, 12.50000000000000000, -1.537336459617587581 ) ) ;
#104057 = CARTESIAN_POINT ( 'NONE',  ( -14.34999999999998543, 2.500000000000000000, -2.511473670974875727 ) ) ;
#104058 = DIRECTION ( 'NONE',  ( 0.000000000000000000, 0.000000000000000000, 1.000000000000000000 ) ) ;
#104059 = LINE ( 'NONE', #14368, #91286 ) ;
#104060 = CARTESIAN_POINT ( 'NONE',  ( -12.69999999999999218, 2.500000000000000000, -4.576537180435974683 ) ) ;
#104061 = DIRECTION ( 'NONE',  ( 0.000000000000000000, 0.000000000000000000, 1.000000000000000000 ) ) ;
#104062 = CARTESIAN_POINT ( 'NONE',  ( -1.700000000000034817, 12.50000000000000000, -4.330127018922201643 ) ) ;
#104063 = DIRECTION ( 'NONE',  ( 0.000000000000000000, 0.000000000000000000, -1.000000000000000000 ) ) ;
#104064 = EDGE_CURVE ( 'NONE', #86788, #11458, #56917, .T. ) ;
#104065 = ADVANCED_FACE ( 'NONE', ( #28785 ), #87679, .T. ) ;
#104066 = DIRECTION ( 'NONE',  ( 0.000000000000000000, -0.000000000000000000, 1.000000000000000000 ) ) ;
#104068 = VERTEX_POINT ( 'NONE', #37948 ) ;
#104067 = VECTOR ( 'NONE', #4698, 1000.000000000000000 ) ;
#104069 = AXIS2_PLACEMENT_3D ( 'NONE', #79345, #77396, #117281 ) ;
#104070 = ADVANCED_FACE ( 'NONE', ( #99461 ), #69713, .T. ) ;
#104071 = CARTESIAN_POINT ( 'NONE',  ( -7.900000000000011013, 2.500000000000000000, 4.230127018922196669 ) ) ;
#104072 = ORIENTED_EDGE ( 'NONE', *, *, #128334, .F. ) ;
#104073 = EDGE_LOOP ( 'NONE', ( #118450, #61512, #64913, #53841 ) ) ;
#104074 = ADVANCED_FACE ( 'NONE', ( #9775 ), #48896, .T. ) ;
#104075 = DIRECTION ( 'NONE',  ( 0.000000000000000000, 0.000000000000000000, 1.000000000000000000 ) ) ;
#104076 = PLANE ( 'NONE',  #42746 ) ;
#104077 = CARTESIAN_POINT ( 'NONE',  ( 3.749999999999940492, 2.500000000000000000, 5.802370205355744659 ) ) ;
#104078 = AXIS2_PLACEMENT_3D ( 'NONE', #92311, #88614, #2629 ) ;
#104079 = CARTESIAN_POINT ( 'NONE',  ( 186.7083333333333428, -4.445597072760135937, -7.699999999999966427 ) ) ;
#104080 = CONICAL_SURFACE ( 'NONE', #97810, 0.1000000000000002554, 0.003490658503988666988 ) ;
#104081 = CIRCLE ( 'NONE', #26718, 0.06509327318403745899 ) ;
#104082 = CARTESIAN_POINT ( 'NONE',  ( 11.64999999999990266, 2.500000000000000000, 2.265063509461097357 ) ) ;
#104083 = DIRECTION ( 'NONE',  ( 0.000000000000000000, 1.000000000000000000, 0.000000000000000000 ) ) ;
#104084 = CARTESIAN_POINT ( 'NONE',  ( -3.750000000000027534, 2.500000000000000000, 2.757883832488649656 ) ) ;
#104085 = ORIENTED_EDGE ( 'NONE', *, *, #118139, .F. ) ;
#104086 = DIRECTION ( 'NONE',  ( -0.000000000000000000, 1.000000000000000000, -0.000000000000000000 ) ) ;
#104087 = DIRECTION ( 'NONE',  ( 0.000000000000000000, 0.000000000000000000, 1.000000000000000000 ) ) ;
#104088 = EDGE_LOOP ( 'NONE', ( #14621, #92711 ) ) ;
#104089 = AXIS2_PLACEMENT_3D ( 'NONE', #108683, #45910, #85810 ) ;
#104090 = EDGE_LOOP ( 'NONE', ( #4706, #102453, #38444, #81541 ) ) ;
#104091 = VERTEX_POINT ( 'NONE', #16970 ) ;
#104092 = AXIS2_PLACEMENT_3D ( 'NONE', #39569, #9437, #119372 ) ;
#104093 = EDGE_LOOP ( 'NONE', ( #118374, #39353 ) ) ;
#104094 = DIRECTION ( 'NONE',  ( -4.274815082592931898E-19, -0.9999939076577903929, -0.003490651415223739937 ) ) ;
#104095 = CARTESIAN_POINT ( 'NONE',  ( -11.05000000000000071, 12.50000000000000000, -2.511473670974873951 ) ) ;
#104096 = AXIS2_PLACEMENT_3D ( 'NONE', #92377, #25399, #2703 ) ;
#104097 = DIRECTION ( 'NONE',  ( -1.000000000000000000, 0.000000000000000000, 0.000000000000000000 ) ) ;
#104098 = CARTESIAN_POINT ( 'NONE',  ( -10.85000000000000142, 2.500000000000000000, -2.165063509461097713 ) ) ;
#104099 = COLOUR_RGB ( '', 0.72549020, 0.75294118, 0.79215686) ;
#104100 = DIRECTION ( 'NONE',  ( 0.000000000000000000, 1.000000000000000000, 0.000000000000000000 ) ) ;
#104101 = VERTEX_POINT ( 'NONE', #68692 ) ;
#104102 = CARTESIAN_POINT ( 'NONE',  ( 87.50000000000001421, -3.975344334345451980, 6.360552532166690476 ) ) ;
#104103 = CARTESIAN_POINT ( 'NONE',  ( -6.650000000000019007, 2.500000000000000000, -1.572243186433550211 ) ) ;
#104104 = CIRCLE ( 'NONE', #66437, 0.06509327318403745899 ) ;
#104105 = ADVANCED_FACE ( 'NONE', ( #98146 ), #47135, .T. ) ;
#104106 = DIRECTION ( 'NONE',  ( 0.000000000000000000, 1.000000000000000000, 0.000000000000000000 ) ) ;
#104107 = VERTEX_POINT ( 'NONE', #39270 ) ;
#104108 = CIRCLE ( 'NONE', #110365, 0.06509327318403745899 ) ;
#104109 = VERTEX_POINT ( 'NONE', #129581 ) ;
#104110 = ORIENTED_EDGE ( 'NONE', *, *, #58631, .F. ) ;
#104111 = EDGE_CURVE ( 'NONE', #114560, #93851, #7086, .T. ) ;
#104112 = DIRECTION ( 'NONE',  ( -0.000000000000000000, 1.000000000000000000, -0.000000000000000000 ) ) ;
#104113 = EDGE_CURVE ( 'NONE', #7472, #69648, #92807, .T. ) ;
#104114 = ADVANCED_FACE ( 'NONE', ( #87039 ), #18935, .T. ) ;
#104115 = AXIS2_PLACEMENT_3D ( 'NONE', #69571, #79415, #119311 ) ;
#104116 = EDGE_CURVE ( 'NONE', #8586, #94676, #852, .T. ) ;
#104117 = DIRECTION ( 'NONE',  ( 0.000000000000000000, 0.000000000000000000, -1.000000000000000000 ) ) ;
#104118 = CARTESIAN_POINT ( 'NONE',  ( 13.09999999999989839, 12.50000000000000000, 0.2813168883297361700 ) ) ;
#104119 = ADVANCED_FACE ( 'NONE', ( #126978 ), #117913, .T. ) ;
#104120 = ORIENTED_EDGE ( 'NONE', *, *, #35668, .T. ) ;
#104121 = CARTESIAN_POINT ( 'NONE',  ( 0.8499999999999557909, 2.500000000000000000, -7.288010851410854585 ) ) ;
#104123 = AXIS2_PLACEMENT_3D ( 'NONE', #107864, #77745, #39157 ) ;
#104122 = CARTESIAN_POINT ( 'NONE',  ( 8.099999999999923261, 2.500000000000000000, -3.883716857408426648 ) ) ;
#104124 = CARTESIAN_POINT ( 'NONE',  ( -14.54999999999998472, 2.500000000000000000, -2.165063509461099489 ) ) ;
#104125 = CARTESIAN_POINT ( 'NONE',  ( 5.399999999999936406, 2.500000000000000000, -4.922947341949753586 ) ) ;
#104126 = ADVANCED_FACE ( 'NONE', ( #107330 ), #17650, .T. ) ;
#104129 = EDGE_CURVE ( 'NONE', #2455, #97521, #94947, .T. ) ;
#104128 = AXIS2_PLACEMENT_3D ( 'NONE', #8636, #129110, #18477 ) ;
#104127 = CONICAL_SURFACE ( 'NONE', #58174, 0.1000000000000000472, 0.003490658503988666988 ) ;
#104130 = CARTESIAN_POINT ( 'NONE',  ( -14.14999999999998614, 2.500000000000000000, 2.265063509461101354 ) ) ;
#104131 = ORIENTED_EDGE ( 'NONE', *, *, #101863, .T. ) ;
#104132 = VERTEX_POINT ( 'NONE', #10415 ) ;
#104133 = DIRECTION ( 'NONE',  ( 1.000000000000000000, 0.000000000000000000, 0.000000000000000000 ) ) ;
#104134 = DIRECTION ( 'NONE',  ( 0.000000000000000000, -0.000000000000000000, 1.000000000000000000 ) ) ;
#104135 = DIRECTION ( 'NONE',  ( 0.000000000000000000, 0.000000000000000000, 1.000000000000000000 ) ) ;
#104136 = CARTESIAN_POINT ( 'NONE',  ( 3.349999999999942801, 2.500000000000000000, 2.857883832488649301 ) ) ;
#104137 = DIRECTION ( 'NONE',  ( 0.000000000000000000, 0.000000000000000000, -1.000000000000000000 ) ) ;
#104138 = VERTEX_POINT ( 'NONE', #12971 ) ;
#104139 = EDGE_LOOP ( 'NONE', ( #51872, #59009 ) ) ;
#104140 = CARTESIAN_POINT ( 'NONE',  ( 9.399999999999915090, 12.50000000000000000, -3.983716857408426293 ) ) ;
#104141 = PLANE ( 'NONE',  #107384 ) ;
#104142 = DIRECTION ( 'NONE',  ( -0.000000000000000000, 1.000000000000000000, -0.000000000000000000 ) ) ;
#104143 = DIRECTION ( 'NONE',  ( -4.274815082592931898E-19, -0.9999939076577903929, -0.003490651415223739937 ) ) ;
#104144 = ORIENTED_EDGE ( 'NONE', *, *, #15445, .T. ) ;
#104145 = DIRECTION ( 'NONE',  ( 0.000000000000000000, 0.000000000000000000, 1.000000000000000000 ) ) ;
#104146 = DIRECTION ( 'NONE',  ( -0.000000000000000000, 1.000000000000000000, -0.000000000000000000 ) ) ;
#104147 = CIRCLE ( 'NONE', #87406, 0.1000000000000002554 ) ;
#104148 = CONICAL_SURFACE ( 'NONE', #97880, 0.1000000000000002554, 0.003490658503988666988 ) ;
#104149 = EDGE_LOOP ( 'NONE', ( #113349, #239, #66507, #38208 ) ) ;
#104150 = AXIS2_PLACEMENT_3D ( 'NONE', #121557, #12879, #91462 ) ;
#104151 = CARTESIAN_POINT ( 'NONE',  ( -15.79999999999998117, 2.500000000000000000, 0.000000000000000000 ) ) ;
#104152 = ORIENTED_EDGE ( 'NONE', *, *, #89063, .F. ) ;
#104153 = DIRECTION ( 'NONE',  ( 0.000000000000000000, -0.9999939076577903929, 0.003490651415223739937 ) ) ;
#104154 = CONICAL_SURFACE ( 'NONE', #47735, 0.09999999999999982514, 0.003490658503988666988 ) ;
#104155 = EDGE_LOOP ( 'NONE', ( #9625, #15375, #124905, #113256 ) ) ;
#104156 = DIRECTION ( 'NONE',  ( 0.000000000000000000, 0.000000000000000000, 1.000000000000000000 ) ) ;
#104157 = DIRECTION ( 'NONE',  ( 0.000000000000000000, 0.000000000000000000, 1.000000000000000000 ) ) ;
#104158 = VERTEX_POINT ( 'NONE', #60814 ) ;
#104159 = ORIENTED_EDGE ( 'NONE', *, *, #96119, .T. ) ;
#104160 = CARTESIAN_POINT ( 'NONE',  ( 186.5052083336747444, -6.551208109652278289, 3.782341765624995134 ) ) ;
#104161 = LINE ( 'NONE', #23029, #62374 ) ;
#104162 = VECTOR ( 'NONE', #29295, 1000.000000000000000 ) ;
#104163 = CARTESIAN_POINT ( 'NONE',  ( -0.4500000000000402012, 2.500000000000000000, 6.495190528383297135 ) ) ;
#104164 = DIRECTION ( 'NONE',  ( 0.000000000000000000, -0.9999939076577903929, 0.003490651415223739937 ) ) ;
#104165 = EDGE_CURVE ( 'NONE', #85814, #98726, #25891, .T. ) ;
#104166 = VECTOR ( 'NONE', #53065, 1000.000000000000000 ) ;
#104167 = LINE ( 'NONE', #95637, #15988 ) ;
#104168 = CARTESIAN_POINT ( 'NONE',  ( 3.549999999999941203, 2.500000000000000000, 6.048780366869521252 ) ) ;
#104169 = DIRECTION ( 'NONE',  ( 0.000000000000000000, 1.000000000000000000, 0.000000000000000000 ) ) ;
#104170 = CARTESIAN_POINT ( 'NONE',  ( 108.0000000000000142, 7.119691004531021328, -5.000000000000004441 ) ) ;
#104171 = ORIENTED_EDGE ( 'NONE', *, *, #47488, .T. ) ;
#104172 = ORIENTED_EDGE ( 'NONE', *, *, #22262, .F. ) ;
#104173 = DIRECTION ( 'NONE',  ( -0.000000000000000000, 1.000000000000000000, -0.000000000000000000 ) ) ;
#104174 = CARTESIAN_POINT ( 'NONE',  ( -14.59999999999998366, 2.500000000000000000, 0.6928203230275518099 ) ) ;
#104175 = CARTESIAN_POINT ( 'NONE',  ( 8.349999999999923261, 2.500000000000000000, -5.902370205355750521 ) ) ;
#104176 = AXIS2_PLACEMENT_3D ( 'NONE', #2832, #21848, #42790 ) ;
#104177 = CARTESIAN_POINT ( 'NONE',  ( -15.39999999999997904, 2.500000000000000000, -0.6928203230275519209 ) ) ;
#104179 = EDGE_LOOP ( 'NONE', ( #91257, #95142, #15087, #105592 ) ) ;
#104178 = VERTEX_POINT ( 'NONE', #102659 ) ;
#104180 = FACE_BOUND ( 'NONE', #70805, .T. ) ;
#104181 = VERTEX_POINT ( 'NONE', #92192 ) ;
#104182 = DIRECTION ( 'NONE',  ( 0.000000000000000000, -0.000000000000000000, 1.000000000000000000 ) ) ;
#104183 = FACE_OUTER_BOUND ( 'NONE', #72908, .T. ) ;
#104184 = VERTEX_POINT ( 'NONE', #51651 ) ;
#104185 = FACE_OUTER_BOUND ( 'NONE', #94992, .T. ) ;
#104186 = AXIS2_PLACEMENT_3D ( 'NONE', #20217, #556, #3161 ) ;
#104187 = CARTESIAN_POINT ( 'NONE',  ( 6.049999999999934097, 12.50000000000000000, 6.148780366869520897 ) ) ;
#104188 = DIRECTION ( 'NONE',  ( -4.274815082592931898E-19, -0.9999939076577903929, -0.003490651415223739937 ) ) ;
#104189 = DIRECTION ( 'NONE',  ( 0.000000000000000000, -0.000000000000000000, 1.000000000000000000 ) ) ;
#104190 = DIRECTION ( 'NONE',  ( 0.000000000000000000, -0.000000000000000000, 1.000000000000000000 ) ) ;
#104191 = DIRECTION ( 'NONE',  ( 0.000000000000000000, -0.9999939076577903929, 0.003490651415223739937 ) ) ;
#104192 = DIRECTION ( 'NONE',  ( 0.000000000000000000, 0.000000000000000000, 1.000000000000000000 ) ) ;
#104193 = LINE ( 'NONE', #15142, #8835 ) ;
#104194 = CIRCLE ( 'NONE', #122986, 0.06509327318403741736 ) ;
#104195 = DIRECTION ( 'NONE',  ( 0.000000000000000000, 1.000000000000000000, 0.000000000000000000 ) ) ;
#104196 = ORIENTED_EDGE ( 'NONE', *, *, #57830, .T. ) ;
#104197 = EDGE_LOOP ( 'NONE', ( #4853, #114909 ) ) ;
#104198 = VERTEX_POINT ( 'NONE', #83044 ) ;
#104199 = DIRECTION ( 'NONE',  ( 0.000000000000000000, 0.000000000000000000, -1.000000000000000000 ) ) ;
#104200 = EDGE_LOOP ( 'NONE', ( #7380, #65179, #4578, #5237 ) ) ;
#104202 = ORIENTED_EDGE ( 'NONE', *, *, #69970, .T. ) ;
#104201 = ORIENTED_EDGE ( 'NONE', *, *, #120186, .F. ) ;
#104203 = VERTEX_POINT ( 'NONE', #121653 ) ;
#104204 = CIRCLE ( 'NONE', #56264, 0.06509327318403745899 ) ;
#104205 = FACE_OUTER_BOUND ( 'NONE', #38289, .T. ) ;
#104206 = ADVANCED_FACE ( 'NONE', ( #122959 ), #40592, .T. ) ;
#104207 = CARTESIAN_POINT ( 'NONE',  ( 10.84999999999990905, 2.500000000000000000, -6.495190528383302464 ) ) ;
#104208 = SURFACE_STYLE_USAGE ( .BOTH. , #64917 ) ;
#104209 = FACE_OUTER_BOUND ( 'NONE', #13939, .T. ) ;
#104210 = CARTESIAN_POINT ( 'NONE',  ( 10.84999999999991260, 12.50000000000000000, -2.099970236277064473 ) ) ;
#104211 = DIRECTION ( 'NONE',  ( 0.000000000000000000, 0.000000000000000000, 1.000000000000000000 ) ) ;
#104212 = EDGE_CURVE ( 'NONE', #48086, #97670, #2914, .T. ) ;
#104213 = ORIENTED_EDGE ( 'NONE', *, *, #113293, .T. ) ;
#104214 = EDGE_CURVE ( 'NONE', #28200, #39206, #80278, .T. ) ;
#104215 = DIRECTION ( 'NONE',  ( 0.000000000000000000, 1.000000000000000000, 0.000000000000000000 ) ) ;
#104216 = ORIENTED_EDGE ( 'NONE', *, *, #96380, .F. ) ;
#104218 = AXIS2_PLACEMENT_3D ( 'NONE', #35868, #117609, #58092 ) ;
#104217 = AXIS2_PLACEMENT_3D ( 'NONE', #27276, #46945, #105194 ) ;
#104219 = EDGE_LOOP ( 'NONE', ( #25969, #92617, #32085, #8894 ) ) ;
#104220 = ORIENTED_EDGE ( 'NONE', *, *, #110520, .T. ) ;
#104221 = EDGE_CURVE ( 'NONE', #46426, #75204, #11703, .T. ) ;
#104223 = EDGE_CURVE ( 'NONE', #126716, #75929, #23844, .T. ) ;
#104222 = DIRECTION ( 'NONE',  ( 0.000000000000000000, 0.000000000000000000, 1.000000000000000000 ) ) ;
#104225 = VERTEX_POINT ( 'NONE', #120382 ) ;
#104224 = ADVANCED_FACE ( 'NONE', ( #60186 ), #111672, .T. ) ;
#104226 = ORIENTED_EDGE ( 'NONE', *, *, #90947, .T. ) ;
#104227 = EDGE_CURVE ( 'NONE', #106745, #60753, #90736, .T. ) ;
#104229 = ORIENTED_EDGE ( 'NONE', *, *, #93414, .T. ) ;
#104228 = ADVANCED_FACE ( 'NONE', ( #81727 ), #84478, .T. ) ;
#104230 = SURFACE_STYLE_USAGE ( .BOTH. , #42765 ) ;
#104231 = DIRECTION ( 'NONE',  ( 0.000000000000000000, 1.000000000000000000, 0.000000000000000000 ) ) ;
#104232 = DIRECTION ( 'NONE',  ( 0.000000000000000000, 1.000000000000000000, 0.000000000000000000 ) ) ;
#104233 = DIRECTION ( 'NONE',  ( 0.000000000000000000, 0.000000000000000000, -1.000000000000000000 ) ) ;
#104234 = CARTESIAN_POINT ( 'NONE',  ( -8.350000000000010303, 12.50000000000000000, 6.560283801567334372 ) ) ;
#104235 = DIRECTION ( 'NONE',  ( -0.000000000000000000, -1.000000000000000000, -0.000000000000000000 ) ) ;
#104236 = EDGE_LOOP ( 'NONE', ( #103585, #261, #60123, #80799 ) ) ;
#104237 = ADVANCED_FACE ( 'NONE', ( #81110 ), #111569, .T. ) ;
#104238 = CARTESIAN_POINT ( 'NONE',  ( -9.350000000000006750, 12.50000000000000000, -2.446380397790840266 ) ) ;
#104239 = ORIENTED_EDGE ( 'NONE', *, *, #117671, .T. ) ;
#104241 = CARTESIAN_POINT ( 'NONE',  ( -13.74999999999998934, 2.500000000000000000, 2.857883832488652853 ) ) ;
#104240 = CIRCLE ( 'NONE', #47814, 0.1000000000000002554 ) ;
#104243 = ORIENTED_EDGE ( 'NONE', *, *, #37055, .F. ) ;
#104242 = CIRCLE ( 'NONE', #1825, 0.06509327318403745899 ) ;
#104244 = CARTESIAN_POINT ( 'NONE',  ( 185.9062500006827747, -8.891194145520236347, -1.633285867636356299E-15 ) ) ;
#104245 = CONICAL_SURFACE ( 'NONE', #120965, 0.1000000000000002554, 0.003490658503988666988 ) ;
#104246 = ORIENTED_EDGE ( 'NONE', *, *, #15399, .T. ) ;
#104247 = VERTEX_POINT ( 'NONE', #40554 ) ;
#104249 = CARTESIAN_POINT ( 'NONE',  ( 12.09999999999990195, 12.50000000000000000, -0.7579135962115916003 ) ) ;
#104248 = CONICAL_SURFACE ( 'NONE', #79130, 0.1000000000000002554, 0.003490658503988666988 ) ;
#104250 = FACE_OUTER_BOUND ( 'NONE', #76860, .T. ) ;
#104251 = CIRCLE ( 'NONE', #37456, 0.06509327318403741736 ) ;
#104252 = CIRCLE ( 'NONE', #83427, 0.1000000000000002554 ) ;
#104253 = AXIS2_PLACEMENT_3D ( 'NONE', #102889, #61041, #71504 ) ;
#104254 = DIRECTION ( 'NONE',  ( 0.000000000000000000, 1.000000000000000000, 0.000000000000000000 ) ) ;
#104255 = EDGE_LOOP ( 'NONE', ( #51970, #6953, #120030, #108418 ) ) ;
#104256 = CARTESIAN_POINT ( 'NONE',  ( 142.3152275665817115, 2.500000000000000000, 2.763522878056728693 ) ) ;
#104257 = ORIENTED_EDGE ( 'NONE', *, *, #48643, .F. ) ;
#104258 = CARTESIAN_POINT ( 'NONE',  ( -2.300000000000033573, 12.50000000000000000, 4.676537180435972552 ) ) ;
#104259 = DIRECTION ( 'NONE',  ( 0.000000000000000000, 1.000000000000000000, 0.000000000000000000 ) ) ;
#104260 = DIRECTION ( 'NONE',  ( 0.000000000000000000, 1.000000000000000000, 0.000000000000000000 ) ) ;
#104261 = CARTESIAN_POINT ( 'NONE',  ( -1.450000000000035039, 2.500000000000000000, -2.411473670974877859 ) ) ;
#104262 = CIRCLE ( 'NONE', #64539, 0.09999999999999982514 ) ;
#104263 = DIRECTION ( 'NONE',  ( 0.000000000000000000, 0.000000000000000000, 1.000000000000000000 ) ) ;
#104264 = CIRCLE ( 'NONE', #8108, 0.06509327318403745899 ) ;
#104265 = ORIENTED_EDGE ( 'NONE', *, *, #61544, .F. ) ;
#104266 = EDGE_CURVE ( 'NONE', #86566, #50747, #38435, .T. ) ;
#104267 = ADVANCED_FACE ( 'NONE', ( #100719 ), #111854, .T. ) ;
#104268 = ORIENTED_EDGE ( 'NONE', *, *, #87093, .T. ) ;
#104269 = CARTESIAN_POINT ( 'NONE',  ( 12.49999999999993960, 2.500000000000000000, -4.330127018922201643 ) ) ;
#104271 = VECTOR ( 'NONE', #85981, 1000.000000000000000 ) ;
#104270 = CARTESIAN_POINT ( 'NONE',  ( 17.50000000000000000, 2.500000000000000888, -4.040567763475094942 ) ) ;
#104272 = ADVANCED_FACE ( 'NONE', ( #102029 ), #34319, .T. ) ;
#104273 = CONICAL_SURFACE ( 'NONE', #129345, 0.1000000000000002554, 0.003490658503988666988 ) ;
#104274 = CARTESIAN_POINT ( 'NONE',  ( 184.4635416670080588, -4.367472073101519747, 7.564683531249999149 ) ) ;
#104275 = CARTESIAN_POINT ( 'NONE',  ( 187.5000000000000000, 0.000000000000000000, 7.700000000000000178 ) ) ;
#104276 = CARTESIAN_POINT ( 'NONE',  ( 3.349999999999943689, 2.500000000000000000, 1.572243186433545548 ) ) ;
#104277 = EDGE_CURVE ( 'NONE', #112874, #35339, #59369, .T. ) ;
#104278 = LINE ( 'NONE', #82723, #106627 ) ;
#104279 = LINE ( 'NONE', #64349, #74733 ) ;
#104280 = ORIENTED_EDGE ( 'NONE', *, *, #67226, .F. ) ;
#104281 = ADVANCED_FACE ( 'NONE', ( #80470 ), #19638, .T. ) ;
#104282 = EDGE_CURVE ( 'NONE', #70210, #115346, #17556, .T. ) ;
#104283 = CARTESIAN_POINT ( 'NONE',  ( 4.349999999999936584, 2.500000000000000000, 6.148780366869520009 ) ) ;
#104284 = EDGE_CURVE ( 'NONE', #56443, #28355, #104593, .T. ) ;
#104285 = DIRECTION ( 'NONE',  ( -4.274815082592931898E-19, -0.9999939076577903929, -0.003490651415223739937 ) ) ;
#104286 = CARTESIAN_POINT ( 'NONE',  ( 88.00000000000001421, 0.000000000000000000, 0.000000000000000000 ) ) ;
#104287 = CIRCLE ( 'NONE', #64561, 0.06509327318403745899 ) ;
#104288 = EDGE_LOOP ( 'NONE', ( #55565, #25851 ) ) ;
#104289 = AXIS2_PLACEMENT_3D ( 'NONE', #6165, #107608, #27115 ) ;
#104290 = EDGE_CURVE ( 'NONE', #82143, #15440, #69809, .T. ) ;
#104291 = CARTESIAN_POINT ( 'NONE',  ( 195.5000000000000000, 9.541191101069066007E-16, 7.541925104783893552 ) ) ;
#104292 = AXIS2_PLACEMENT_3D ( 'NONE', #103164, #123440, #82894 ) ;
#104293 = ORIENTED_EDGE ( 'NONE', *, *, #104934, .T. ) ;
#104294 = DIRECTION ( 'NONE',  ( 0.000000000000000000, 0.000000000000000000, 1.000000000000000000 ) ) ;
#104295 = ORIENTED_EDGE ( 'NONE', *, *, #74977, .T. ) ;
#104297 = AXIS2_PLACEMENT_3D ( 'NONE', #104364, #114816, #112901 ) ;
#104296 = CARTESIAN_POINT ( 'NONE',  ( 8.749999999999918288, 2.500000000000000000, -1.472243186433550122 ) ) ;
#104298 = FACE_OUTER_BOUND ( 'NONE', #62208, .T. ) ;
#104299 = CARTESIAN_POINT ( 'NONE',  ( -2.700000000000031264, 2.500000000000000000, 4.576537180435972019 ) ) ;
#104300 = ORIENTED_EDGE ( 'NONE', *, *, #82968, .T. ) ;
#104301 = CARTESIAN_POINT ( 'NONE',  ( 6.649999999999930189, 2.500000000000000000, -2.957883832488653830 ) ) ;
#104302 = CONICAL_SURFACE ( 'NONE', #108496, 0.1000000000000000472, 0.003490658503988666988 ) ;
#104303 = CARTESIAN_POINT ( 'NONE',  ( -7.500000000000013323, 12.50000000000000000, 5.022947341949748790 ) ) ;
#104304 = AXIS2_PLACEMENT_3D ( 'NONE', #7566, #48813, #67784 ) ;
#104305 = EDGE_CURVE ( 'NONE', #35339, #112874, #107458, .T. ) ;
#104306 = VERTEX_POINT ( 'NONE', #95429 ) ;
#104307 = DIRECTION ( 'NONE',  ( 0.000000000000000000, 0.000000000000000000, -1.000000000000000000 ) ) ;
#104308 = VECTOR ( 'NONE', #55471, 1000.000000000000000 ) ;
#104309 = ORIENTED_EDGE ( 'NONE', *, *, #63174, .T. ) ;
#104310 = ORIENTED_EDGE ( 'NONE', *, *, #111890, .F. ) ;
#104311 = DIRECTION ( 'NONE',  ( 0.000000000000000000, -0.000000000000000000, 1.000000000000000000 ) ) ;
#104312 = DIRECTION ( 'NONE',  ( -0.000000000000000000, 1.000000000000000000, -0.000000000000000000 ) ) ;
#104313 = FACE_OUTER_BOUND ( 'NONE', #88827, .T. ) ;
#104314 = VERTEX_POINT ( 'NONE', #105887 ) ;
#104315 = DIRECTION ( 'NONE',  ( 0.000000000000000000, 0.000000000000000000, -1.000000000000000000 ) ) ;
#104316 = LINE ( 'NONE', #101743, #29379 ) ;
#104317 = ORIENTED_EDGE ( 'NONE', *, *, #115589, .T. ) ;
#104318 = CARTESIAN_POINT ( 'NONE',  ( -9.400000000000007461, 2.500000000000000000, 3.983716857408420076 ) ) ;
#104319 = PLANE ( 'NONE',  #126575 ) ;
#104320 = EDGE_CURVE ( 'NONE', #44872, #8732, #123582, .T. ) ;
#104321 = CARTESIAN_POINT ( 'NONE',  ( -0.6000000000000323963, 2.500000000000000000, 0.3464101615137759604 ) ) ;
#104322 = FACE_OUTER_BOUND ( 'NONE', #114932, .T. ) ;
#104323 = VECTOR ( 'NONE', #86938, 1000.000000000000000 ) ;
#104324 = CARTESIAN_POINT ( 'NONE',  ( 162.5000000000000000, 0.5000000000000000000, 7.499999999999994671 ) ) ;
#104325 = DIRECTION ( 'NONE',  ( 0.000000000000000000, -0.9999939076577903929, 0.003490651415223739937 ) ) ;
#104326 = CARTESIAN_POINT ( 'NONE',  ( 8.349999999999919709, 12.50000000000000000, 7.188010851410848723 ) ) ;
#104327 = CONICAL_SURFACE ( 'NONE', #98061, 0.09999999999999982514, 0.003490658503988666988 ) ;
#104328 = ORIENTED_EDGE ( 'NONE', *, *, #61643, .F. ) ;
#104329 = EDGE_LOOP ( 'NONE', ( #190, #30033 ) ) ;
#104330 = VERTEX_POINT ( 'NONE', #115044 ) ;
#104331 = VERTEX_POINT ( 'NONE', #16196 ) ;
#104332 = CARTESIAN_POINT ( 'NONE',  ( -8.950000000000011724, 12.50000000000000000, -6.148780366869520897 ) ) ;
#104333 = FACE_OUTER_BOUND ( 'NONE', #74391, .T. ) ;
#104334 = FACE_OUTER_BOUND ( 'NONE', #62053, .T. ) ;
#104335 = VERTEX_POINT ( 'NONE', #24111 ) ;
#104336 = EDGE_CURVE ( 'NONE', #107226, #55968, #30118, .T. ) ;
#104337 = FACE_BOUND ( 'NONE', #58627, .T. ) ;
#104338 = CARTESIAN_POINT ( 'NONE',  ( -9.550000000000002487, 2.500000000000000000, 6.595190528383296780 ) ) ;
#104339 = CARTESIAN_POINT ( 'NONE',  ( -5.400000000000023448, 2.500000000000000000, -4.922947341949753586 ) ) ;
#104340 = AXIS2_PLACEMENT_3D ( 'NONE', #8135, #15365, #115502 ) ;
#104341 = CONICAL_SURFACE ( 'NONE', #83517, 0.1000000000000002554, 0.003490658503988666988 ) ;
#104342 = LINE ( 'NONE', #122692, #65873 ) ;
#104343 = CONICAL_SURFACE ( 'NONE', #60543, 0.1000000000000000472, 0.003490658503988666988 ) ;
#104344 = DIRECTION ( 'NONE',  ( 0.000000000000000000, -0.9999939076577903929, 0.003490651415223739937 ) ) ;
#104345 = DIRECTION ( 'NONE',  ( 0.000000000000000000, 1.000000000000000000, 0.000000000000000000 ) ) ;
#104346 = DIRECTION ( 'NONE',  ( 0.000000000000000000, 0.000000000000000000, 1.000000000000000000 ) ) ;
#104347 = DIRECTION ( 'NONE',  ( -4.274815082592931898E-19, -0.9999939076577903929, -0.003490651415223739937 ) ) ;
#104348 = DIRECTION ( 'NONE',  ( 0.000000000000000000, 0.000000000000000000, 1.000000000000000000 ) ) ;
#104349 = CARTESIAN_POINT ( 'NONE',  ( -10.65000000000000213, 2.500000000000000000, 6.148780366869520009 ) ) ;
#104350 = AXIS2_PLACEMENT_3D ( 'NONE', #100444, #103680, #72919 ) ;
#104351 = DIRECTION ( 'NONE',  ( -0.000000000000000000, 1.000000000000000000, -0.000000000000000000 ) ) ;
#104352 = AXIS2_PLACEMENT_3D ( 'NONE', #105226, #84296, #17967 ) ;
#104353 = ORIENTED_EDGE ( 'NONE', *, *, #117782, .F. ) ;
#104354 = ORIENTED_EDGE ( 'NONE', *, *, #54890, .T. ) ;
#104355 = ORIENTED_EDGE ( 'NONE', *, *, #27251, .T. ) ;
#104356 = ORIENTED_EDGE ( 'NONE', *, *, #66156, .T. ) ;
#104357 = DIRECTION ( 'NONE',  ( 0.000000000000000000, 0.000000000000000000, 1.000000000000000000 ) ) ;
#104358 = VERTEX_POINT ( 'NONE', #103319 ) ;
#104359 = CARTESIAN_POINT ( 'NONE',  ( 12.29999999999990656, 12.50000000000000000, 3.983716857408420964 ) ) ;
#104360 = VERTEX_POINT ( 'NONE', #73850 ) ;
#104361 = ORIENTED_EDGE ( 'NONE', *, *, #7739, .T. ) ;
#104362 = EDGE_CURVE ( 'NONE', #96862, #78573, #124887, .T. ) ;
#104363 = CARTESIAN_POINT ( 'NONE',  ( 8.512291507236847465, -2.500000000000381473, 9.502944100472593192 ) ) ;
#104364 = CARTESIAN_POINT ( 'NONE',  ( -3.950000000000024603, 12.50000000000000000, 1.818653347947321475 ) ) ;
#104365 = CARTESIAN_POINT ( 'NONE',  ( -5.850000000000021849, 2.500000000000000000, -1.572243186433550211 ) ) ;
#104366 = AXIS2_PLACEMENT_3D ( 'NONE', #109742, #60017, #99924 ) ;
#104367 = CARTESIAN_POINT ( 'NONE',  ( -14.34999999999998543, 2.500000000000000000, -2.511473670974875727 ) ) ;
#104368 = ORIENTED_EDGE ( 'NONE', *, *, #106521, .T. ) ;
#104369 = EDGE_CURVE ( 'NONE', #83004, #107108, #94132, .T. ) ;
#104370 = ORIENTED_EDGE ( 'NONE', *, *, #85301, .T. ) ;
#104371 = EDGE_LOOP ( 'NONE', ( #36807, #44261, #69171, #17800 ) ) ;
#104373 = ORIENTED_EDGE ( 'NONE', *, *, #68733, .F. ) ;
#104372 = DIRECTION ( 'NONE',  ( 0.000000000000000000, 0.000000000000000000, 1.000000000000000000 ) ) ;
#104374 = ADVANCED_FACE ( 'NONE', ( #35234 ), #53573, .T. ) ;
#104376 = EDGE_CURVE ( 'NONE', #75521, #122569, #56131, .T. ) ;
#104375 = CARTESIAN_POINT ( 'NONE',  ( 184.6250000000000000, -8.891194145520236347, -1.633285867636356299E-15 ) ) ;
#104378 = VERTEX_POINT ( 'NONE', #5096 ) ;
#104377 = EDGE_CURVE ( 'NONE', #127091, #38693, #103960, .T. ) ;
#104379 = EDGE_CURVE ( 'NONE', #107914, #47637, #59459, .T. ) ;
#104380 = ORIENTED_EDGE ( 'NONE', *, *, #43160, .F. ) ;
#104381 = CIRCLE ( 'NONE', #121100, 0.06509327318403741736 ) ;
#104382 = DIRECTION ( 'NONE',  ( 0.000000000000000000, 0.000000000000000000, 1.000000000000000000 ) ) ;
#104383 = DIRECTION ( 'NONE',  ( -0.000000000000000000, -1.000000000000000000, -0.000000000000000000 ) ) ;
#104384 = CARTESIAN_POINT ( 'NONE',  ( -8.950000000000009948, 12.50000000000000000, -6.776507416713035248 ) ) ;
#104385 = DIRECTION ( 'NONE',  ( 0.000000000000000000, -0.000000000000000000, 1.000000000000000000 ) ) ;
#104386 = DIRECTION ( 'NONE',  ( 0.000000000000000000, 0.000000000000000000, -1.000000000000000000 ) ) ;
#104387 = VECTOR ( 'NONE', #58511, 1000.000000000000000 ) ;
#104388 = EDGE_CURVE ( 'NONE', #60541, #113663, #82440, .T. ) ;
#104389 = EDGE_LOOP ( 'NONE', ( #79589, #88514, #17484, #79745 ) ) ;
#104390 = CARTESIAN_POINT ( 'NONE',  ( -9.600000000000006750, 2.500000000000000000, 5.022947341949748790 ) ) ;
#104391 = ADVANCED_FACE ( 'NONE', ( #45053 ), #124248, .F. ) ;
#104392 = EDGE_CURVE ( 'NONE', #84812, #116290, #9261, .T. ) ;
#104393 = EDGE_LOOP ( 'NONE', ( #19688, #105402 ) ) ;
#104394 = CARTESIAN_POINT ( 'NONE',  ( 17.50000000000000000, 2.499999999999999556, 0.3333333333333366455 ) ) ;
#104396 = CIRCLE ( 'NONE', #33311, 0.09999999999999982514 ) ;
#104395 = AXIS2_PLACEMENT_3D ( 'NONE', #10250, #122155, #90742 ) ;
#104397 = ORIENTED_EDGE ( 'NONE', *, *, #112829, .T. ) ;
#104398 = CARTESIAN_POINT ( 'NONE',  ( 3.099999999999945466, 2.500000000000000000, 0.3464101615137735735 ) ) ;
#104399 = DIRECTION ( 'NONE',  ( 0.000000000000000000, 1.000000000000000000, 0.000000000000000000 ) ) ;
#104400 = VECTOR ( 'NONE', #113510, 1000.000000000000000 ) ;
#104401 = FACE_OUTER_BOUND ( 'NONE', #61231, .T. ) ;
#104402 = CARTESIAN_POINT ( 'NONE',  ( 4.799999999999939426, 2.500000000000000000, -4.576537180435977348 ) ) ;
#104403 = EDGE_LOOP ( 'NONE', ( #24927, #107246 ) ) ;
#104404 = DIRECTION ( 'NONE',  ( 0.000000000000000000, 0.000000000000000000, 1.000000000000000000 ) ) ;
#104405 = VECTOR ( 'NONE', #110720, 1000.000000000000000 ) ;
#104406 = CARTESIAN_POINT ( 'NONE',  ( -8.750000000000005329, 12.50000000000000000, 5.867463478539781896 ) ) ;
#104407 = ORIENTED_EDGE ( 'NONE', *, *, #1288, .T. ) ;
#104408 = ORIENTED_EDGE ( 'NONE', *, *, #68155, .T. ) ;
#104409 = ORIENTED_EDGE ( 'NONE', *, *, #27220, .T. ) ;
#104410 = CARTESIAN_POINT ( 'NONE',  ( 4.999999999999935163, 12.50000000000000000, 0.6277270498435120194 ) ) ;
#104411 = DIRECTION ( 'NONE',  ( -0.000000000000000000, 1.000000000000000000, -0.000000000000000000 ) ) ;
#104412 = CARTESIAN_POINT ( 'NONE',  ( 184.5260416670080588, -6.551208109652273848, -3.782341765625003571 ) ) ;
#104413 = CARTESIAN_POINT ( 'NONE',  ( -8.150000000000009237, 2.500000000000000000, 6.048780366869520364 ) ) ;
#104414 = DIRECTION ( 'NONE',  ( 0.000000000000000000, 0.000000000000000000, 1.000000000000000000 ) ) ;
#104415 = DIRECTION ( 'NONE',  ( 0.000000000000000000, 1.000000000000000000, 0.000000000000000000 ) ) ;
#104416 = AXIS2_PLACEMENT_3D ( 'NONE', #44788, #123967, #34333 ) ;
#104417 = ORIENTED_EDGE ( 'NONE', *, *, #84108, .T. ) ;
#104418 = PLANE ( 'NONE',  #111221 ) ;
#104419 = CONICAL_SURFACE ( 'NONE', #70971, 0.1000000000000002554, 0.003490658503988666988 ) ;
#104420 = AXIS2_PLACEMENT_3D ( 'NONE', #35205, #75117, #105214 ) ;
#104421 = ORIENTED_EDGE ( 'NONE', *, *, #68445, .T. ) ;
#104422 = CARTESIAN_POINT ( 'NONE',  ( -13.29999999999999005, 12.50000000000000000, -4.265033745738161741 ) ) ;
#104423 = DIRECTION ( 'NONE',  ( 0.000000000000000000, -0.000000000000000000, 1.000000000000000000 ) ) ;
#104424 = EDGE_CURVE ( 'NONE', #69263, #4103, #103055, .T. ) ;
#104425 = CARTESIAN_POINT ( 'NONE',  ( 7.099999999999928590, 2.500000000000000000, -4.230127018922201998 ) ) ;
#104426 = AXIS2_PLACEMENT_3D ( 'NONE', #97015, #16504, #7980 ) ;
#104427 = ORIENTED_EDGE ( 'NONE', *, *, #18414, .T. ) ;
#104428 = AXIS2_PLACEMENT_3D ( 'NONE', #40993, #101181, #19375 ) ;
#104429 = EDGE_CURVE ( 'NONE', #8018, #33146, #46313, .T. ) ;
#104430 = CIRCLE ( 'NONE', #14532, 0.06509327318403745899 ) ;
#104431 = EDGE_CURVE ( 'NONE', #46303, #117313, #42440, .T. ) ;
#104432 = CARTESIAN_POINT ( 'NONE',  ( -4.400000000000025224, 2.500000000000000000, 4.776537180435972196 ) ) ;
#104433 = DIRECTION ( 'NONE',  ( 0.000000000000000000, 0.000000000000000000, 1.000000000000000000 ) ) ;
#104434 = CONICAL_SURFACE ( 'NONE', #50086, 0.1000000000000000056, 0.003490658503988666988 ) ;
#104435 = EDGE_LOOP ( 'NONE', ( #30236, #100253 ) ) ;
#104436 = ADVANCED_FACE ( 'NONE', ( #48917 ), #69166, .T. ) ;
#104437 = CARTESIAN_POINT ( 'NONE',  ( -9.150000000000009237, 2.500000000000000000, -2.165063509461101710 ) ) ;
#104438 = VECTOR ( 'NONE', #121325, 1000.000000000000000 ) ;
#104439 = AXIS2_PLACEMENT_3D ( 'NONE', #25724, #15240, #85921 ) ;
#104440 = ORIENTED_EDGE ( 'NONE', *, *, #27105, .T. ) ;
#104441 = EDGE_LOOP ( 'NONE', ( #99467, #34444 ) ) ;
#104442 = CARTESIAN_POINT ( 'NONE',  ( 4.599999999999940137, 2.500000000000000000, -4.430127018922202176 ) ) ;
#104443 = ORIENTED_EDGE ( 'NONE', *, *, #97078, .F. ) ;
#104444 = CARTESIAN_POINT ( 'NONE',  ( -10.40000000000000213, 12.50000000000000000, -0.06509327318403970719 ) ) ;
#104445 = FACE_OUTER_BOUND ( 'NONE', #98510, .T. ) ;
#104446 = CARTESIAN_POINT ( 'NONE',  ( -7.050000000000013145, 2.500000000000000000, 2.265063509461097357 ) ) ;
#104447 = ORIENTED_EDGE ( 'NONE', *, *, #84580, .T. ) ;
#104448 = FACE_BOUND ( 'NONE', #116955, .T. ) ;
#104449 = DIRECTION ( 'NONE',  ( 0.000000000000000000, 0.000000000000000000, -1.000000000000000000 ) ) ;
#104451 = EDGE_LOOP ( 'NONE', ( #98911, #41148 ) ) ;
#104450 = CARTESIAN_POINT ( 'NONE',  ( 10.44999999999991047, 2.500000000000000000, -6.595190528383302109 ) ) ;
#104452 = DIRECTION ( 'NONE',  ( 0.000000000000000000, -0.9999939076577903929, 0.003490651415223739937 ) ) ;
#104453 = DIRECTION ( 'NONE',  ( 0.000000000000000000, 0.000000000000000000, 1.000000000000000000 ) ) ;
#104454 = EDGE_CURVE ( 'NONE', #49071, #43610, #80082, .T. ) ;
#104455 = ORIENTED_EDGE ( 'NONE', *, *, #8992, .T. ) ;
#104456 = ORIENTED_EDGE ( 'NONE', *, *, #109419, .T. ) ;
#104457 = ORIENTED_EDGE ( 'NONE', *, *, #101847, .T. ) ;
#104458 = FACE_OUTER_BOUND ( 'NONE', #31423, .T. ) ;
#104459 = CARTESIAN_POINT ( 'NONE',  ( -9.800000000000006040, 2.500000000000000000, 0.3464101615137735735 ) ) ;
#104460 =( BOUNDED_CURVE ( )  B_SPLINE_CURVE ( 2, ( #53433, #89648, #19614, #29440, #23301, #100114, #83536 ),
 .UNSPECIFIED., .F., .F. ) 
 B_SPLINE_CURVE_WITH_KNOTS ( ( 3, 2, 2, 3 ),
 ( 0.000000000000000000, 0.02380952380952383249, 0.04761904761904766498, 0.07142857142857149400 ),
 .UNSPECIFIED. ) 
 CURVE ( )  GEOMETRIC_REPRESENTATION_ITEM ( )  RATIONAL_B_SPLINE_CURVE ( ( 1.000000000000000000, 0.8660254037844387076, 1.000000000000000000, 0.8660254037844387076, 1.000000000000000000, 0.8660254037844383745, 1.000000000000000444 ) ) 
 REPRESENTATION_ITEM ( '' )  );
#104461 = DIRECTION ( 'NONE',  ( -0.000000000000000000, -1.000000000000000000, -0.000000000000000000 ) ) ;
#104462 = FACE_BOUND ( 'NONE', #67086, .T. ) ;
#104463 = VERTEX_POINT ( 'NONE', #107818 ) ;
#104464 = CARTESIAN_POINT ( 'NONE',  ( 185.4843750003414300, -8.734944146203032389, -1.604583208406768146E-15 ) ) ;
#104465 = DIRECTION ( 'NONE',  ( 0.000000000000000000, 1.000000000000000000, 0.000000000000000000 ) ) ;
#104466 = CARTESIAN_POINT ( 'NONE',  ( 7.299999999999924327, 12.50000000000000000, 0.3464101615137735735 ) ) ;
#104467 = CARTESIAN_POINT ( 'NONE',  ( 6.649999999999929301, 2.500000000000000000, -2.165063509461101710 ) ) ;
#104468 = ADVANCED_FACE ( 'NONE', ( #27307 ), #105406, .T. ) ;
#104469 = CARTESIAN_POINT ( 'NONE',  ( -9.150000000000009237, 12.50000000000000000, 1.407149913249508000 ) ) ;
#104470 = DIRECTION ( 'NONE',  ( 0.000000000000000000, 0.000000000000000000, -1.000000000000000000 ) ) ;
#104471 = CONICAL_SURFACE ( 'NONE', #62730, 0.1000000000000000472, 0.003490658503988666988 ) ;
#104472 = CARTESIAN_POINT ( 'NONE',  ( 0.1999999999999627909, 12.50000000000000000, 0.3464101615137758494 ) ) ;
#104473 = LINE ( 'NONE', #33804, #55770 ) ;
#104475 = CONICAL_SURFACE ( 'NONE', #18792, 0.09999999999999999167, 0.003490658503988666988 ) ;
#104474 = VECTOR ( 'NONE', #76266, 1000.000000000000000 ) ;
#104476 = ORIENTED_EDGE ( 'NONE', *, *, #92553, .F. ) ;
#104477 = ORIENTED_EDGE ( 'NONE', *, *, #44710, .T. ) ;
#104478 = ORIENTED_EDGE ( 'NONE', *, *, #21917, .T. ) ;
#104479 = ORIENTED_EDGE ( 'NONE', *, *, #74846, .T. ) ;
#104480 = ORIENTED_EDGE ( 'NONE', *, *, #14633, .T. ) ;
#104481 = DIRECTION ( 'NONE',  ( 0.000000000000000000, 0.000000000000000000, 1.000000000000000000 ) ) ;
#104482 = VECTOR ( 'NONE', #4038, 1000.000000000000114 ) ;
#104483 = FACE_OUTER_BOUND ( 'NONE', #32912, .T. ) ;
#104484 = ORIENTED_EDGE ( 'NONE', *, *, #19997, .T. ) ;
#104485 = EDGE_CURVE ( 'NONE', #120320, #27458, #66601, .T. ) ;
#104486 = FACE_BOUND ( 'NONE', #100105, .T. ) ;
#104487 = DIRECTION ( 'NONE',  ( 0.000000000000000000, 1.000000000000000000, 0.000000000000000000 ) ) ;
#104488 = AXIS2_PLACEMENT_3D ( 'NONE', #48436, #119112, #16999 ) ;
#104489 = DIRECTION ( 'NONE',  ( 0.000000000000000000, 0.000000000000000000, -1.000000000000000000 ) ) ;
#104490 = ORIENTED_EDGE ( 'NONE', *, *, #20346, .F. ) ;
#104491 = CARTESIAN_POINT ( 'NONE',  ( -13.29999999999999005, 2.500000000000000000, 0.1000000000000018513 ) ) ;
#104492 = EDGE_CURVE ( 'NONE', #75483, #24119, #19424, .T. ) ;
#104493 = DIRECTION ( 'NONE',  ( -0.000000000000000000, 1.000000000000000000, -0.000000000000000000 ) ) ;
#104494 = DIRECTION ( 'NONE',  ( 0.000000000000000000, 1.000000000000000000, 0.000000000000000000 ) ) ;
#104495 = ORIENTED_EDGE ( 'NONE', *, *, #55306, .T. ) ;
#104496 = LINE ( 'NONE', #5640, #47146 ) ;
#104497 = ORIENTED_EDGE ( 'NONE', *, *, #114602, .T. ) ;
#104498 = ORIENTED_EDGE ( 'NONE', *, *, #18913, .T. ) ;
#104499 = ORIENTED_EDGE ( 'NONE', *, *, #69347, .F. ) ;
#104500 = PLANE ( 'NONE',  #115345 ) ;
#104501 = CARTESIAN_POINT ( 'NONE',  ( 0.1999999999999627909, 2.500000000000000000, 0.3464101615137758494 ) ) ;
#104502 = CARTESIAN_POINT ( 'NONE',  ( -15.19999999999998330, 2.500000000000000000, 0.2464101615137758439 ) ) ;
#104503 = ORIENTED_EDGE ( 'NONE', *, *, #43299, .T. ) ;
#104504 = CARTESIAN_POINT ( 'NONE',  ( -10.65000000000000391, 2.500000000000000000, -1.818653347947322141 ) ) ;
#104505 = AXIS2_PLACEMENT_3D ( 'NONE', #80564, #50, #91021 ) ;
#104506 = DIRECTION ( 'NONE',  ( 0.000000000000000000, 0.000000000000000000, 1.000000000000000000 ) ) ;
#104507 = AXIS2_PLACEMENT_3D ( 'NONE', #15946, #95820, #125906 ) ;
#104508 = EDGE_CURVE ( 'NONE', #51768, #29710, #9618, .T. ) ;
#104509 = CARTESIAN_POINT ( 'NONE',  ( -2.900000000000029221, 2.500000000000000000, -0.5928203230275541635 ) ) ;
#104510 = CARTESIAN_POINT ( 'NONE',  ( 185.1979166673494603, 6.668395609140176816, 3.850000000000000977 ) ) ;
#104512 = ORIENTED_EDGE ( 'NONE', *, *, #36889, .F. ) ;
#104511 = DIRECTION ( 'NONE',  ( 0.000000000000000000, 1.000000000000000000, 0.000000000000000000 ) ) ;
#104513 = FACE_OUTER_BOUND ( 'NONE', #103817, .T. ) ;
#104514 = VERTEX_POINT ( 'NONE', #48252 ) ;
#104515 = DIRECTION ( 'NONE',  ( -0.000000000000000000, -1.000000000000000000, -0.000000000000000000 ) ) ;
#104516 = CIRCLE ( 'NONE', #48097, 0.1000000000000000472 ) ;
#104517 = ADVANCED_FACE ( 'NONE', ( #126172 ), #116975, .T. ) ;
#104518 = ORIENTED_EDGE ( 'NONE', *, *, #43503, .T. ) ;
#104519 = ORIENTED_EDGE ( 'NONE', *, *, #40246, .F. ) ;
#104520 = DIRECTION ( 'NONE',  ( -0.000000000000000000, 1.000000000000000000, -0.000000000000000000 ) ) ;
#104521 = CARTESIAN_POINT ( 'NONE',  ( 11.04999999999991012, 2.500000000000000000, 6.841600689897072485 ) ) ;
#104522 = ADVANCED_FACE ( 'NONE', ( #58725 ), #23638, .T. ) ;
#104523 = DIRECTION ( 'NONE',  ( -4.274815082592931898E-19, -0.9999939076577903929, -0.003490651415223739937 ) ) ;
#104525 = EDGE_CURVE ( 'NONE', #12341, #104358, #40381, .T. ) ;
#104524 = LINE ( 'NONE', #124823, #42550 ) ;
#104526 = EDGE_CURVE ( 'NONE', #106999, #2948, #18784, .T. ) ;
#104527 = DIRECTION ( 'NONE',  ( 0.000000000000000000, 0.000000000000000000, 1.000000000000000000 ) ) ;
#104529 = EDGE_CURVE ( 'NONE', #44872, #51386, #92600, .T. ) ;
#104528 = AXIS2_PLACEMENT_3D ( 'NONE', #82927, #12228, #80985 ) ;
#104530 = ORIENTED_EDGE ( 'NONE', *, *, #25147, .F. ) ;
#104531 = ORIENTED_EDGE ( 'NONE', *, *, #72897, .F. ) ;
#104532 = CIRCLE ( 'NONE', #114982, 0.06509327318403745899 ) ;
#104533 = CARTESIAN_POINT ( 'NONE',  ( -14.34999999999998543, 2.500000000000000000, -1.818653347947323695 ) ) ;
#104534 = AXIS2_PLACEMENT_3D ( 'NONE', #99635, #20425, #2700 ) ;
#104535 = PLANE ( 'NONE',  #22309 ) ;
#104536 = EDGE_CURVE ( 'NONE', #24357, #78982, #3005, .T. ) ;
#104537 = DIRECTION ( 'NONE',  ( 0.000000000000000000, 0.000000000000000000, -1.000000000000000000 ) ) ;
#104538 = ORIENTED_EDGE ( 'NONE', *, *, #11726, .T. ) ;
#104539 = ORIENTED_EDGE ( 'NONE', *, *, #45093, .T. ) ;
#104540 = ADVANCED_FACE ( 'NONE', ( #86883 ), #18142, .T. ) ;
#104541 = CARTESIAN_POINT ( 'NONE',  ( -5.850000000000021849, 2.500000000000000000, -5.802370205355749988 ) ) ;
#104542 = ADVANCED_FACE ( 'NONE', ( #87523 ), #37163, .T. ) ;
#104543 = ORIENTED_EDGE ( 'NONE', *, *, #68193, .T. ) ;
#104544 = CARTESIAN_POINT ( 'NONE',  ( -4.600000000000025402, 2.500000000000000000, -2.385244779468109755E-15 ) ) ;
#104545 = EDGE_CURVE ( 'NONE', #79392, #85331, #126030, .T. ) ;
#104546 = ADVANCED_FACE ( 'NONE', ( #97992 ), #113523, .T. ) ;
#104547 = DIRECTION ( 'NONE',  ( 0.000000000000000000, 0.000000000000000000, 1.000000000000000000 ) ) ;
#104548 = EDGE_LOOP ( 'NONE', ( #73421, #62273, #9171, #75575 ) ) ;
#104549 = DIRECTION ( 'NONE',  ( 0.000000000000000000, 0.000000000000000000, 1.000000000000000000 ) ) ;
#104550 = CARTESIAN_POINT ( 'NONE',  ( 5.399999999999934630, 2.500000000000000000, -0.5928203230275542746 ) ) ;
#104551 = AXIS2_PLACEMENT_3D ( 'NONE', #120420, #60853, #109960 ) ;
#104552 = DIRECTION ( 'NONE',  ( 0.000000000000000000, 1.000000000000000000, 0.000000000000000000 ) ) ;
#104554 = EDGE_CURVE ( 'NONE', #48799, #105604, #57085, .T. ) ;
#104553 = CARTESIAN_POINT ( 'NONE',  ( 1.049999999999953637, 12.50000000000000000, -1.818653347947326138 ) ) ;
#104555 = ORIENTED_EDGE ( 'NONE', *, *, #106869, .T. ) ;
#104556 = DIRECTION ( 'NONE',  ( -0.000000000000000000, -1.000000000000000000, -0.000000000000000000 ) ) ;
#104557 = FACE_OUTER_BOUND ( 'NONE', #51737, .T. ) ;
#104558 = ORIENTED_EDGE ( 'NONE', *, *, #10262, .F. ) ;
#104559 = ORIENTED_EDGE ( 'NONE', *, *, #65676, .F. ) ;
#104560 = LINE ( 'NONE', #126131, #4461 ) ;
#104561 = DIRECTION ( 'NONE',  ( 0.000000000000000000, 1.000000000000000000, 0.000000000000000000 ) ) ;
#104562 = CARTESIAN_POINT ( 'NONE',  ( 130.5000000000000000, -0.5000000000000000000, -7.500000000000001776 ) ) ;
#104563 = DIRECTION ( 'NONE',  ( 0.000000000000000000, 0.000000000000000000, 1.000000000000000000 ) ) ;
#104564 = CARTESIAN_POINT ( 'NONE',  ( -0.4500000000000402012, 2.500000000000000000, 6.395190528383296602 ) ) ;
#104565 = DIRECTION ( 'NONE',  ( 0.000000000000000000, 0.000000000000000000, -1.000000000000000000 ) ) ;
#104566 = DIRECTION ( 'NONE',  ( 0.000000000000000000, -0.9999939076577903929, 0.003490651415223739937 ) ) ;
#104567 = FACE_OUTER_BOUND ( 'NONE', #116001, .T. ) ;
#104568 = CARTESIAN_POINT ( 'NONE',  ( -5.450000000000023270, 2.500000000000000000, -6.395190528383301931 ) ) ;
#104569 = CONICAL_SURFACE ( 'NONE', #20943, 0.09999999999999982514, 0.003490658503988666988 ) ;
#104570 = CIRCLE ( 'NONE', #6338, 0.06509327318403745899 ) ;
#104571 = DIRECTION ( 'NONE',  ( 0.000000000000000000, -0.9999939076577903929, 0.003490651415223739937 ) ) ;
#104572 = EDGE_LOOP ( 'NONE', ( #65576, #121503 ) ) ;
#104573 = ORIENTED_EDGE ( 'NONE', *, *, #74412, .F. ) ;
#104574 = CIRCLE ( 'NONE', #48147, 0.06509327318403745899 ) ;
#104575 = VERTEX_POINT ( 'NONE', #40385 ) ;
#104576 = VERTEX_POINT ( 'NONE', #1719 ) ;
#104577 = DIRECTION ( 'NONE',  ( 0.000000000000000000, -0.000000000000000000, 1.000000000000000000 ) ) ;
#104578 = CARTESIAN_POINT ( 'NONE',  ( 12.89999999999989733, 12.50000000000000000, -2.385244779468109755E-15 ) ) ;
#104579 = DIRECTION ( 'NONE',  ( -4.274815082592931898E-19, -0.9999939076577903929, -0.003490651415223739937 ) ) ;
#104580 = ORIENTED_EDGE ( 'NONE', *, *, #107985, .T. ) ;
#104581 = DIRECTION ( 'NONE',  ( -0.000000000000000000, -1.000000000000000000, -0.000000000000000000 ) ) ;
#104582 = ADVANCED_FACE ( 'NONE', ( #1084 ), #6884, .T. ) ;
#104583 = EDGE_CURVE ( 'NONE', #57277, #116085, #61307, .T. ) ;
#104584 = CARTESIAN_POINT ( 'NONE',  ( 4.349999999999939249, 2.500000000000000000, 2.511473670974873507 ) ) ;
#104586 = ORIENTED_EDGE ( 'NONE', *, *, #17666, .F. ) ;
#104585 = DIRECTION ( 'NONE',  ( 0.000000000000000000, 1.000000000000000000, 0.000000000000000000 ) ) ;
#104587 = CARTESIAN_POINT ( 'NONE',  ( -4.200000000000029488, 12.50000000000000000, -4.330127018922201643 ) ) ;
#104588 = ORIENTED_EDGE ( 'NONE', *, *, #39669, .F. ) ;
#104589 = ADVANCED_FACE ( 'NONE', ( #424 ), #30208, .T. ) ;
#104590 = ORIENTED_EDGE ( 'NONE', *, *, #118875, .F. ) ;
#104591 = ORIENTED_EDGE ( 'NONE', *, *, #6387, .T. ) ;
#104592 = EDGE_LOOP ( 'NONE', ( #45788, #96716, #57972, #76385 ) ) ;
#104593 = LINE ( 'NONE', #84953, #53085 ) ;
#104594 = DIRECTION ( 'NONE',  ( 0.000000000000000000, -0.9999939076577903929, 0.003490651415223739937 ) ) ;
#104595 = CARTESIAN_POINT ( 'NONE',  ( 3.749999999999944045, 12.50000000000000000, -7.188010851410854052 ) ) ;
#104596 = FACE_OUTER_BOUND ( 'NONE', #99706, .T. ) ;
#104597 = VECTOR ( 'NONE', #84415, 1000.000000000000000 ) ;
#104598 = VERTEX_POINT ( 'NONE', #80306 ) ;
#104599 = VECTOR ( 'NONE', #70577, 1000.000000000000000 ) ;
#104600 = CARTESIAN_POINT ( 'NONE',  ( 9.399999999999915090, 2.500000000000000000, 4.676537180435972552 ) ) ;
#104601 = VERTEX_POINT ( 'NONE', #80948 ) ;
#104602 = CARTESIAN_POINT ( 'NONE',  ( 8.749999999999918288, 2.500000000000000000, 7.088010851410848190 ) ) ;
#104603 = DIRECTION ( 'NONE',  ( 0.000000000000000000, 0.000000000000000000, 1.000000000000000000 ) ) ;
#104604 = DIRECTION ( 'NONE',  ( 0.000000000000000000, 0.000000000000000000, 1.000000000000000000 ) ) ;
#104605 = LINE ( 'NONE', #74512, #84038 ) ;
#104606 = AXIS2_PLACEMENT_3D ( 'NONE', #94621, #53432, #74998 ) ;
#104607 = EDGE_LOOP ( 'NONE', ( #104973, #46406 ) ) ;
#104608 = VERTEX_POINT ( 'NONE', #12814 ) ;
#104609 = EDGE_LOOP ( 'NONE', ( #80374, #111713 ) ) ;
#104610 = LINE ( 'NONE', #14912, #44005 ) ;
#104611 = DIRECTION ( 'NONE',  ( -0.000000000000000000, 1.000000000000000000, -0.000000000000000000 ) ) ;
#104612 = PLANE ( 'NONE',  #16859 ) ;
#104613 = FACE_BOUND ( 'NONE', #125175, .T. ) ;
#104614 = CARTESIAN_POINT ( 'NONE',  ( 6.649999999999930189, 12.50000000000000000, 5.802370205355744659 ) ) ;
#104615 = CARTESIAN_POINT ( 'NONE',  ( 3.549999999999943867, 12.50000000000000000, -1.818653347947326138 ) ) ;
#104616 = PLANE ( 'NONE',  #29108 ) ;
#104618 = EDGE_CURVE ( 'NONE', #71554, #126826, #52895, .T. ) ;
#104617 = AXIS2_PLACEMENT_3D ( 'NONE', #85750, #15049, #17654 ) ;
#104619 = CIRCLE ( 'NONE', #100424, 0.06509327318403745899 ) ;
#104620 = CARTESIAN_POINT ( 'NONE',  ( 186.6302083336747728, -4.367472073101514418, -7.564683531250002702 ) ) ;
#104621 = DIRECTION ( 'NONE',  ( 0.000000000000000000, 0.000000000000000000, 1.000000000000000000 ) ) ;
#104622 = DIRECTION ( 'NONE',  ( -4.274815082592931898E-19, -0.9999939076577903929, -0.003490651415223739937 ) ) ;
#104623 = ORIENTED_EDGE ( 'NONE', *, *, #40193, .F. ) ;
#104624 = AXIS2_PLACEMENT_3D ( 'NONE', #98811, #49097, #119107 ) ;
#104625 = FACE_OUTER_BOUND ( 'NONE', #97351, .T. ) ;
#104626 = ORIENTED_EDGE ( 'NONE', *, *, #7892, .T. ) ;
#104627 = CONICAL_SURFACE ( 'NONE', #79603, 0.1000000000000002554, 0.003490658503988666988 ) ;
#104628 = ORIENTED_EDGE ( 'NONE', *, *, #118583, .T. ) ;
#104629 = ORIENTED_EDGE ( 'NONE', *, *, #63600, .F. ) ;
#104630 = ORIENTED_EDGE ( 'NONE', *, *, #15107, .T. ) ;
#104631 = EDGE_CURVE ( 'NONE', #124173, #108711, #29907, .T. ) ;
#104632 = DIRECTION ( 'NONE',  ( 0.000000000000000000, 0.000000000000000000, 1.000000000000000000 ) ) ;
#104633 = FACE_BOUND ( 'NONE', #52558, .T. ) ;
#104634 = CARTESIAN_POINT ( 'NONE',  ( 0.8499999999999536815, 2.500000000000000000, 6.595190528383296780 ) ) ;
#104635 = EDGE_LOOP ( 'NONE', ( #33208, #61388, #33348, #72204 ) ) ;
#104636 = CARTESIAN_POINT ( 'NONE',  ( 23.99354682432708330, 2.839181451644113618, 2.508508607402079260 ) ) ;
#104637 = EDGE_CURVE ( 'NONE', #57040, #92171, #128416, .T. ) ;
#104638 = CARTESIAN_POINT ( 'NONE',  ( 8.349999999999919709, 2.500000000000000000, -2.857883832488653741 ) ) ;
#104639 = ORIENTED_EDGE ( 'NONE', *, *, #114426, .T. ) ;
#104640 = DIRECTION ( 'NONE',  ( 0.000000000000000000, 0.000000000000000000, 1.000000000000000000 ) ) ;
#104641 = PLANE ( 'NONE',  #55366 ) ;
#104642 = ORIENTED_EDGE ( 'NONE', *, *, #59953, .F. ) ;
#104643 = AXIS2_PLACEMENT_3D ( 'NONE', #23762, #85871, #113420 ) ;
#104644 = FACE_OUTER_BOUND ( 'NONE', #116273, .T. ) ;
#104645 = CIRCLE ( 'NONE', #33656, 0.06509327318403745899 ) ;
#104646 = CARTESIAN_POINT ( 'NONE',  ( -10.85000000000000142, 2.500000000000000000, -2.065063509461098068 ) ) ;
#104647 = ORIENTED_EDGE ( 'NONE', *, *, #55259, .F. ) ;
#104648 = DIRECTION ( 'NONE',  ( 0.000000000000000000, 0.000000000000000000, -1.000000000000000000 ) ) ;
#104649 = PRESENTATION_LAYER_ASSIGNMENT (  '', '', ( #85869 ) ) ;
#104650 = CARTESIAN_POINT ( 'NONE',  ( 187.0312500006828031, 9.429780353434619030E-16, -7.700000000000000178 ) ) ;
#104651 = DIRECTION ( 'NONE',  ( 0.000000000000000000, 1.000000000000000000, 0.000000000000000000 ) ) ;
#104652 = VERTEX_POINT ( 'NONE', #101871 ) ;
#104653 = AXIS2_PLACEMENT_3D ( 'NONE', #70409, #52067, #31777 ) ;
#104654 = ORIENTED_EDGE ( 'NONE', *, *, #46969, .T. ) ;
#104655 = DIRECTION ( 'NONE',  ( 0.000000000000000000, 0.000000000000000000, 1.000000000000000000 ) ) ;
#104656 = VERTEX_POINT ( 'NONE', #31212 ) ;
#104657 = FACE_OUTER_BOUND ( 'NONE', #49400, .T. ) ;
#104658 = CARTESIAN_POINT ( 'NONE',  ( 15.59999999999988951, 12.50000000000000000, -0.4115034346978157509 ) ) ;
#104659 = EDGE_CURVE ( 'NONE', #3256, #115958, #71970, .T. ) ;
#104660 = ORIENTED_EDGE ( 'NONE', *, *, #120394, .T. ) ;
#104661 = FACE_OUTER_BOUND ( 'NONE', #79178, .T. ) ;
#104662 = DIRECTION ( 'NONE',  ( 1.000000000000000000, 0.000000000000000000, 0.000000000000000000 ) ) ;
#104663 = CARTESIAN_POINT ( 'NONE',  ( 6.249999999999930722, 12.50000000000000000, 7.188010851410848723 ) ) ;
#104664 = DIRECTION ( 'NONE',  ( 0.000000000000000000, 0.000000000000000000, -1.000000000000000000 ) ) ;
#104665 = ADVANCED_FACE ( 'NONE', ( #2348 ), #48986, .T. ) ;
#104666 = CARTESIAN_POINT ( 'NONE',  ( -0.4000000000000396572, 2.500000000000000000, 4.430127018922196847 ) ) ;
#104667 = ADVANCED_FACE ( 'NONE', ( #99941 ), #42745, .T. ) ;
#104668 = ORIENTED_EDGE ( 'NONE', *, *, #77795, .T. ) ;
#104669 = VERTEX_POINT ( 'NONE', #50207 ) ;
#104670 = PLANE ( 'NONE',  #129007 ) ;
#104671 = DIRECTION ( 'NONE',  ( 0.000000000000000000, -0.9999939076577903929, 0.003490651415223739937 ) ) ;
#104672 = ADVANCED_FACE ( 'NONE', ( #41037 ), #111014, .T. ) ;
#104673 = CARTESIAN_POINT ( 'NONE',  ( -7.500000000000015099, 2.500000000000000000, -4.922947341949753586 ) ) ;
#104675 = ORIENTED_EDGE ( 'NONE', *, *, #67888, .F. ) ;
#104674 = ORIENTED_EDGE ( 'NONE', *, *, #103558, .F. ) ;
#104676 = EDGE_CURVE ( 'NONE', #74488, #70177, #110390, .T. ) ;
#104677 = VERTEX_POINT ( 'NONE', #70473 ) ;
#104678 = ADVANCED_FACE ( 'NONE', ( #20734 ), #31845, .T. ) ;
#104679 = FACE_OUTER_BOUND ( 'NONE', #76025, .T. ) ;
#104680 = CIRCLE ( 'NONE', #27311, 0.06509327318403741736 ) ;
#104681 = CARTESIAN_POINT ( 'NONE',  ( -11.64999999999999680, 12.50000000000000000, 2.857883832488649301 ) ) ;
#104682 = CONICAL_SURFACE ( 'NONE', #106829, 0.09999999999999982514, 0.003490658503988666988 ) ;
#104683 = CARTESIAN_POINT ( 'NONE',  ( -4.350000000000023626, 12.50000000000000000, 1.883746621131358934 ) ) ;
#104684 = EDGE_CURVE ( 'NONE', #101605, #77155, #36273, .T. ) ;
#104685 = CARTESIAN_POINT ( 'NONE',  ( -2.300000000000033573, 2.500000000000000000, 4.776537180435972196 ) ) ;
#104686 = DIRECTION ( 'NONE',  ( 0.000000000000000000, 0.000000000000000000, 1.000000000000000000 ) ) ;
#104687 = PLANE ( 'NONE',  #84140 ) ;
#104688 = CARTESIAN_POINT ( 'NONE',  ( 6.049999999999935874, 2.500000000000000000, -6.841600689897077814 ) ) ;
#104689 = FACE_OUTER_BOUND ( 'NONE', #114953, .T. ) ;
#104692 = EDGE_CURVE ( 'NONE', #19953, #105928, #78019, .T. ) ;
#104691 = AXIS2_PLACEMENT_3D ( 'NONE', #96071, #6370, #27314 ) ;
#104690 = DIRECTION ( 'NONE',  ( 0.000000000000000000, 0.000000000000000000, 1.000000000000000000 ) ) ;
#104693 = CONICAL_SURFACE ( 'NONE', #235, 0.09999999999999982514, 0.003490658503988666988 ) ;
#104694 = EDGE_LOOP ( 'NONE', ( #16808, #71632 ) ) ;
#104695 = DIRECTION ( 'NONE',  ( -4.274815082592931898E-19, -0.9999939076577903929, -0.003490651415223739937 ) ) ;
#104696 = ORIENTED_EDGE ( 'NONE', *, *, #59789, .T. ) ;
#104697 = VERTEX_POINT ( 'NONE', #62600 ) ;
#104698 = CARTESIAN_POINT ( 'NONE',  ( 7.299999999999926104, 2.500000000000000000, 4.676537180435972552 ) ) ;
#104699 = DIRECTION ( 'NONE',  ( 0.000000000000000000, 1.000000000000000000, 0.000000000000000000 ) ) ;
#104700 = CARTESIAN_POINT ( 'NONE',  ( -13.74999999999998934, 2.500000000000000000, -1.372243186433547812 ) ) ;
#104701 = CIRCLE ( 'NONE', #48290, 0.06509327318403743123 ) ;
#104702 = DIRECTION ( 'NONE',  ( 0.000000000000000000, -0.000000000000000000, 1.000000000000000000 ) ) ;
#104703 = VECTOR ( 'NONE', #93359, 1000.000000000000000 ) ;
#104705 = CARTESIAN_POINT ( 'NONE',  ( 12.89999999999989910, 2.500000000000000000, -0.6928203230275542523 ) ) ;
#104704 = PRODUCT_DEFINITION_SHAPE ( 'NONE', 'NONE',  #129624 ) ;
#104706 = FACE_OUTER_BOUND ( 'NONE', #19028, .T. ) ;
#104707 = DIRECTION ( 'NONE',  ( -0.000000000000000000, -1.000000000000000000, -0.000000000000000000 ) ) ;
#104708 = ORIENTED_EDGE ( 'NONE', *, *, #44863, .F. ) ;
#104709 = DIRECTION ( 'NONE',  ( 0.000000000000000000, 0.000000000000000000, -1.000000000000000000 ) ) ;
#104710 = CONICAL_SURFACE ( 'NONE', #94257, 0.09999999999999982514, 0.003490658503988666988 ) ;
#104711 = CARTESIAN_POINT ( 'NONE',  ( -0.8500000000000395017, 2.500000000000000000, 6.595190528383296780 ) ) ;
#104712 = ORIENTED_EDGE ( 'NONE', *, *, #40311, .F. ) ;
#104713 = ORIENTED_EDGE ( 'NONE', *, *, #49032, .F. ) ;
#104714 = CIRCLE ( 'NONE', #79684, 0.06509327318403745899 ) ;
#104715 = EDGE_LOOP ( 'NONE', ( #75472, #123087 ) ) ;
#104716 = VERTEX_POINT ( 'NONE', #89469 ) ;
#104717 = PLANE ( 'NONE',  #21158 ) ;
#104718 = DIRECTION ( 'NONE',  ( 0.000000000000000000, 0.000000000000000000, -1.000000000000000000 ) ) ;
#104719 = DIRECTION ( 'NONE',  ( -1.000000000000000000, 0.000000000000000000, 1.224646799147352221E-16 ) ) ;
#104720 = ADVANCED_FACE ( 'NONE', ( #129428 ), #39752, .T. ) ;
#104721 = FACE_OUTER_BOUND ( 'NONE', #99297, .T. ) ;
#104722 = CARTESIAN_POINT ( 'NONE',  ( 17.50000000000000000, 2.500000000000000000, 4.000000000000000888 ) ) ;
#104723 = ORIENTED_EDGE ( 'NONE', *, *, #57247, .T. ) ;
#104724 = DIRECTION ( 'NONE',  ( -0.000000000000000000, 1.000000000000000000, -0.000000000000000000 ) ) ;
#104725 = DIRECTION ( 'NONE',  ( 0.000000000000000000, 0.000000000000000000, 1.000000000000000000 ) ) ;
#104727 = EDGE_CURVE ( 'NONE', #94262, #58821, #23746, .T. ) ;
#104726 = DIRECTION ( 'NONE',  ( 0.000000000000000000, 1.000000000000000000, 0.000000000000000000 ) ) ;
#104728 = ORIENTED_EDGE ( 'NONE', *, *, #108417, .F. ) ;
#104729 = ORIENTED_EDGE ( 'NONE', *, *, #97582, .F. ) ;
#104730 = ORIENTED_EDGE ( 'NONE', *, *, #38854, .T. ) ;
#104731 = CONICAL_SURFACE ( 'NONE', #40015, 0.1000000000000002554, 0.003490658503988666988 ) ;
#104732 = CARTESIAN_POINT ( 'NONE',  ( 8.549999999999924327, 12.50000000000000000, 1.818653347947321475 ) ) ;
#104733 = CONICAL_SURFACE ( 'NONE', #54560, 0.09999999999999982514, 0.003490658503988666988 ) ;
#104734 = CARTESIAN_POINT ( 'NONE',  ( -3.749999999999991118, 12.50000000000000000, 2.165063509461097713 ) ) ;
#104735 = DIRECTION ( 'NONE',  ( 0.000000000000000000, 1.000000000000000000, 0.000000000000000000 ) ) ;
#104736 = AXIS2_PLACEMENT_3D ( 'NONE', #74020, #62909, #43286 ) ;
#104737 = ORIENTED_EDGE ( 'NONE', *, *, #79570, .F. ) ;
#104738 = DIRECTION ( 'NONE',  ( 0.000000000000000000, 1.000000000000000000, 0.000000000000000000 ) ) ;
#104739 = DIRECTION ( 'NONE',  ( -0.000000000000000000, 1.000000000000000000, -0.000000000000000000 ) ) ;
#104740 = CARTESIAN_POINT ( 'NONE',  ( 9.549999999999918998, 12.50000000000000000, 2.099970236277060032 ) ) ;
#104741 = DIRECTION ( 'NONE',  ( 0.000000000000000000, 1.000000000000000000, 0.000000000000000000 ) ) ;
#104742 = LINE ( 'NONE', #104125, #89585 ) ;
#104743 = ORIENTED_EDGE ( 'NONE', *, *, #88633, .T. ) ;
#104744 = DIRECTION ( 'NONE',  ( 0.000000000000000000, 1.000000000000000000, 0.000000000000000000 ) ) ;
#104745 = VERTEX_POINT ( 'NONE', #84144 ) ;
#104746 = EDGE_LOOP ( 'NONE', ( #35606, #43651 ) ) ;
#104747 = DIRECTION ( 'NONE',  ( 0.000000000000000000, 0.000000000000000000, -1.000000000000000000 ) ) ;
#104748 = FACE_BOUND ( 'NONE', #124439, .T. ) ;
#104749 = DIRECTION ( 'NONE',  ( 0.000000000000000000, 0.000000000000000000, 1.000000000000000000 ) ) ;
#104750 = CARTESIAN_POINT ( 'NONE',  ( -4.250072516143177381E-14, 12.50000000000000000, -3.637306695894650055 ) ) ;
#104751 = DIRECTION ( 'NONE',  ( 0.000000000000000000, 0.000000000000000000, 1.000000000000000000 ) ) ;
#104752 = EDGE_CURVE ( 'NONE', #57522, #26422, #115663, .T. ) ;
#104753 = ORIENTED_EDGE ( 'NONE', *, *, #11567, .F. ) ;
#104754 = EDGE_LOOP ( 'NONE', ( #65761, #44802, #58976, #115435 ) ) ;
#104756 = EDGE_CURVE ( 'NONE', #70003, #55669, #74339, .T. ) ;
#104755 = CARTESIAN_POINT ( 'NONE',  ( -6.650000000000019007, 12.50000000000000000, -5.737276932171712751 ) ) ;
#104757 = LINE ( 'NONE', #15079, #36305 ) ;
#104758 = LINE ( 'NONE', #107359, #50792 ) ;
#104759 = LINE ( 'NONE', #46499, #23885 ) ;
#104760 = ORIENTED_EDGE ( 'NONE', *, *, #67851, .F. ) ;
#104761 = CIRCLE ( 'NONE', #96360, 0.1000000000000000472 ) ;
#104762 = EDGE_CURVE ( 'NONE', #80302, #88979, #92688, .T. ) ;
#104763 = DIRECTION ( 'NONE',  ( -0.000000000000000000, 1.000000000000000000, -0.000000000000000000 ) ) ;
#104764 = AXIS2_PLACEMENT_3D ( 'NONE', #35658, #27125, #65747 ) ;
#104765 = DIRECTION ( 'NONE',  ( 0.000000000000000000, 0.000000000000000000, -1.000000000000000000 ) ) ;
#104766 = VERTEX_POINT ( 'NONE', #114259 ) ;
#104767 = EDGE_CURVE ( 'NONE', #57867, #51861, #82886, .T. ) ;
#104768 = CARTESIAN_POINT ( 'NONE',  ( 6.849999999999929479, 12.50000000000000000, -2.511473670974877948 ) ) ;
#104769 = EDGE_CURVE ( 'NONE', #56167, #113064, #57179, .T. ) ;
#104770 = EDGE_LOOP ( 'NONE', ( #68245, #129179, #108776, #19199 ) ) ;
#104771 = FACE_BOUND ( 'NONE', #29254, .T. ) ;
#104772 = CONICAL_SURFACE ( 'NONE', #121498, 0.09999999999999982514, 0.003490658503988666988 ) ;
#104773 = LINE ( 'NONE', #22389, #57896 ) ;
#104774 = AXIS2_PLACEMENT_3D ( 'NONE', #19564, #49689, #110519 ) ;
#104775 = VERTEX_POINT ( 'NONE', #33140 ) ;
#104776 = CARTESIAN_POINT ( 'NONE',  ( 7.099999999999928590, 2.500000000000000000, -4.922947341949753586 ) ) ;
#104777 = DIRECTION ( 'NONE',  ( 0.000000000000000000, -0.9999939076577903929, 0.003490651415223739937 ) ) ;
#104778 = EDGE_CURVE ( 'NONE', #8315, #44421, #52981, .T. ) ;
#104779 = ORIENTED_EDGE ( 'NONE', *, *, #113099, .F. ) ;
#104780 = EDGE_LOOP ( 'NONE', ( #116379, #129293 ) ) ;
#104781 = EDGE_CURVE ( 'NONE', #81044, #69509, #71764, .T. ) ;
#104782 = CARTESIAN_POINT ( 'NONE',  ( 186.9635416670080303, -4.367472073101519747, 7.564683531249999149 ) ) ;
#104784 = CARTESIAN_POINT ( 'NONE',  ( 184.6718750003414016, 9.264065473108010111E-16, -7.564683531250000925 ) ) ;
#104783 = AXIS2_PLACEMENT_3D ( 'NONE', #119563, #129430, #88155 ) ;
#104785 = DIRECTION ( 'NONE',  ( -0.000000000000000000, 1.000000000000000000, -0.000000000000000000 ) ) ;
#104786 = AXIS2_PLACEMENT_3D ( 'NONE', #127341, #126687, #96556 ) ;
#104787 = CARTESIAN_POINT ( 'NONE',  ( 5.449999999999934452, 2.500000000000000000, 2.165063509461097713 ) ) ;
#104788 = VECTOR ( 'NONE', #22669, 1000.000000000000000 ) ;
#104789 = CARTESIAN_POINT ( 'NONE',  ( -3.642919299551294898E-14, 2.500000000000000000, 0.6928203230275518099 ) ) ;
#104790 = DIRECTION ( 'NONE',  ( -4.274815082592931898E-19, -0.9999939076577903929, -0.003490651415223739937 ) ) ;
#104791 = DIRECTION ( 'NONE',  ( 0.000000000000000000, 0.000000000000000000, 1.000000000000000000 ) ) ;
#104792 = AXIS2_PLACEMENT_3D ( 'NONE', #63900, #104461, #74362 ) ;
#104793 = EDGE_LOOP ( 'NONE', ( #96210, #74189, #128577, #13719 ) ) ;
#104794 = ORIENTED_EDGE ( 'NONE', *, *, #8365, .T. ) ;
#104795 = CARTESIAN_POINT ( 'NONE',  ( -3.750000000000027534, 12.50000000000000000, 2.922977105672686982 ) ) ;
#104796 = AXIS2_PLACEMENT_3D ( 'NONE', #10608, #110125, #19140 ) ;
#104797 = VECTOR ( 'NONE', #125473, 1000.000000000000000 ) ;
#104798 = DIRECTION ( 'NONE',  ( 0.000000000000000000, 0.000000000000000000, -1.000000000000000000 ) ) ;
#104799 = DIRECTION ( 'NONE',  ( -0.000000000000000000, -1.000000000000000000, -0.000000000000000000 ) ) ;
#104800 = DIRECTION ( 'NONE',  ( -0.000000000000000000, 1.000000000000000000, -0.000000000000000000 ) ) ;
#104802 = ORIENTED_EDGE ( 'NONE', *, *, #82999, .T. ) ;
#104801 = VERTEX_POINT ( 'NONE', #54056 ) ;
#104803 = FACE_BOUND ( 'NONE', #63894, .T. ) ;
#104804 = ORIENTED_EDGE ( 'NONE', *, *, #45404, .T. ) ;
#104805 = DIRECTION ( 'NONE',  ( 1.000000000000000000, 0.000000000000000000, 0.000000000000000000 ) ) ;
#104806 = DIRECTION ( 'NONE',  ( 0.000000000000000000, 1.000000000000000000, 0.000000000000000000 ) ) ;
#104807 = EDGE_LOOP ( 'NONE', ( #95716, #19890, #121291, #67423 ) ) ;
#104808 = DIRECTION ( 'NONE',  ( 0.000000000000000000, 1.000000000000000000, 0.000000000000000000 ) ) ;
#104809 = CARTESIAN_POINT ( 'NONE',  ( -5.200000000000022382, 2.500000000000000000, 4.576537180435972019 ) ) ;
#104810 = ADVANCED_FACE ( 'NONE', ( #83528 ), #67533, .T. ) ;
#104811 = DIRECTION ( 'NONE',  ( 0.000000000000000000, 0.000000000000000000, 1.000000000000000000 ) ) ;
#104812 = DIRECTION ( 'NONE',  ( -0.000000000000000000, 1.000000000000000000, -0.000000000000000000 ) ) ;
#104813 = CARTESIAN_POINT ( 'NONE',  ( -8.750000000000007105, 12.50000000000000000, 7.188010851410848723 ) ) ;
#104814 = DIRECTION ( 'NONE',  ( 0.000000000000000000, 1.000000000000000000, 0.000000000000000000 ) ) ;
#104815 = CARTESIAN_POINT ( 'NONE',  ( 186.9427083336747160, -6.551208109652278289, 3.782341765624995134 ) ) ;
#104816 = DIRECTION ( 'NONE',  ( 0.000000000000000000, 0.000000000000000000, -1.000000000000000000 ) ) ;
#104817 = PLANE ( 'NONE',  #107892 ) ;
#104818 = EDGE_CURVE ( 'NONE', #52810, #91937, #55345, .T. ) ;
#104819 = EDGE_LOOP ( 'NONE', ( #21904, #36719 ) ) ;
#104820 = ORIENTED_EDGE ( 'NONE', *, *, #13713, .F. ) ;
#104821 = VERTEX_POINT ( 'NONE', #23292 ) ;
#104822 = DIRECTION ( 'NONE',  ( 0.000000000000000000, 0.000000000000000000, -1.000000000000000000 ) ) ;
#104823 = EDGE_LOOP ( 'NONE', ( #21149, #44459 ) ) ;
#104824 = AXIS2_PLACEMENT_3D ( 'NONE', #33963, #73882, #32698 ) ;
#104825 = CARTESIAN_POINT ( 'NONE',  ( 21.24754738303277435, 0.7337760880902381988, 4.182111650399361835 ) ) ;
#104826 = AXIS2_PLACEMENT_3D ( 'NONE', #107136, #67861, #106504 ) ;
#104827 = EDGE_CURVE ( 'NONE', #11852, #45708, #42537, .T. ) ;
#104828 = AXIS2_PLACEMENT_3D ( 'NONE', #21154, #2809, #80741 ) ;
#104830 = VERTEX_POINT ( 'NONE', #93339 ) ;
#104829 = VERTEX_POINT ( 'NONE', #45536 ) ;
#104831 = ORIENTED_EDGE ( 'NONE', *, *, #80772, .T. ) ;
#104832 = ADVANCED_FACE ( 'NONE', ( #125374 ), #25218, .T. ) ;
#104833 = FACE_OUTER_BOUND ( 'NONE', #37120, .T. ) ;
#104834 = EDGE_CURVE ( 'NONE', #127971, #13889, #75953, .T. ) ;
#104835 = AXIS2_PLACEMENT_3D ( 'NONE', #41845, #22208, #12987 ) ;
#104836 = CARTESIAN_POINT ( 'NONE',  ( -1.250000000000037970, 2.500000000000000000, 7.088010851410848190 ) ) ;
#104837 = CIRCLE ( 'NONE', #33747, 0.06509327318403741736 ) ;
#104838 =( LENGTH_UNIT ( ) NAMED_UNIT ( * ) SI_UNIT ( .MILLI., .METRE. ) );
#104839 = EDGE_CURVE ( 'NONE', #84139, #4806, #25785, .T. ) ;
#104840 = CARTESIAN_POINT ( 'NONE',  ( -5.650000000000019895, 2.500000000000000000, 6.248780366869520542 ) ) ;
#104841 = DIRECTION ( 'NONE',  ( -4.274815082592931898E-19, -0.9999939076577903929, -0.003490651415223739937 ) ) ;
#104842 = CIRCLE ( 'NONE', #105026, 0.1000000000000000472 ) ;
#104843 = DIRECTION ( 'NONE',  ( 0.000000000000000000, -0.000000000000000000, 1.000000000000000000 ) ) ;
#104844 = ORIENTED_EDGE ( 'NONE', *, *, #53840, .T. ) ;
#104846 = EDGE_CURVE ( 'NONE', #122810, #89858, #113620, .T. ) ;
#104845 = CARTESIAN_POINT ( 'NONE',  ( -9.350000000000006750, 2.500000000000000000, -1.818653347947325916 ) ) ;
#104848 = ORIENTED_EDGE ( 'NONE', *, *, #128523, .F. ) ;
#104847 = AXIS2_PLACEMENT_3D ( 'NONE', #69722, #109651, #67103 ) ;
#104849 = EDGE_CURVE ( 'NONE', #66518, #13897, #13253, .T. ) ;
#104850 = EDGE_LOOP ( 'NONE', ( #72147, #96601, #115675, #26039 ) ) ;
#104851 = ORIENTED_EDGE ( 'NONE', *, *, #31174, .F. ) ;
#104852 = CARTESIAN_POINT ( 'NONE',  ( -1.700000000000034817, 12.50000000000000000, -2.385244779468109755E-15 ) ) ;
#104853 = VERTEX_POINT ( 'NONE', #54672 ) ;
#104854 = VERTEX_POINT ( 'NONE', #105070 ) ;
#104855 = EDGE_LOOP ( 'NONE', ( #15833, #55528 ) ) ;
#104856 = CARTESIAN_POINT ( 'NONE',  ( 7.699999999999923794, 12.50000000000000000, 4.611443907251934426 ) ) ;
#104857 = DIRECTION ( 'NONE',  ( 0.000000000000000000, -0.000000000000000000, 1.000000000000000000 ) ) ;
#104858 = FACE_OUTER_BOUND ( 'NONE', #27474, .T. ) ;
#104859 = CARTESIAN_POINT ( 'NONE',  ( 2.899999999999945732, 2.500000000000000000, -4.330127018922201643 ) ) ;
#104860 = CARTESIAN_POINT ( 'NONE',  ( 12.93920187831608892, 1.500000000000000222, 10.00000000000000000 ) ) ;
#104861 = EDGE_LOOP ( 'NONE', ( #59171, #92034, #121907, #63175 ) ) ;
#104862 = FACE_OUTER_BOUND ( 'NONE', #2473, .T. ) ;
#104863 = CONICAL_SURFACE ( 'NONE', #17007, 0.1000000000000002554, 0.003490658503988666988 ) ;
#104864 = AXIS2_PLACEMENT_3D ( 'NONE', #119215, #69454, #108740 ) ;
#104865 = ORIENTED_EDGE ( 'NONE', *, *, #39432, .F. ) ;
#104866 = DIRECTION ( 'NONE',  ( 0.000000000000000000, 1.000000000000000000, 0.000000000000000000 ) ) ;
#104867 = ORIENTED_EDGE ( 'NONE', *, *, #10828, .T. ) ;
#104868 = FACE_OUTER_BOUND ( 'NONE', #38899, .T. ) ;
#104869 = EDGE_LOOP ( 'NONE', ( #64780, #92505 ) ) ;
#104870 = ORIENTED_EDGE ( 'NONE', *, *, #50513, .T. ) ;
#104871 = CIRCLE ( 'NONE', #19090, 0.09999999999999982514 ) ;
#104872 = LINE ( 'NONE', #83948, #109634 ) ;
#104873 = CARTESIAN_POINT ( 'NONE',  ( 0.3999999999999559464, 2.500000000000000000, -4.230127018922201998 ) ) ;
#104874 = CIRCLE ( 'NONE', #113288, 0.1000000000000002554 ) ;
#104875 = VECTOR ( 'NONE', #85826, 1000.000000000000000 ) ;
#104876 = CARTESIAN_POINT ( 'NONE',  ( 5.599999999999933031, 12.50000000000000000, -0.2813168883297409439 ) ) ;
#104877 = DIRECTION ( 'NONE',  ( -0.000000000000000000, 1.000000000000000000, -0.000000000000000000 ) ) ;
#104878 = ORIENTED_EDGE ( 'NONE', *, *, #105832, .T. ) ;
#104879 = DIRECTION ( 'NONE',  ( 0.000000000000000000, 0.000000000000000000, -1.000000000000000000 ) ) ;
#104880 = DIRECTION ( 'NONE',  ( -0.000000000000000000, -1.000000000000000000, -0.000000000000000000 ) ) ;
#104881 =( REPRESENTATION_RELATIONSHIP ('NONE','NONE', #102928, #125483 ) REPRESENTATION_RELATIONSHIP_WITH_TRANSFORMATION ( #87624 )SHAPE_REPRESENTATION_RELATIONSHIP( ) );
#104882 = CARTESIAN_POINT ( 'NONE',  ( 186.0000000000000000, 0.000000000000000000, 7.700000000000000178 ) ) ;
#104883 = DIRECTION ( 'NONE',  ( 0.000000000000000000, 1.000000000000000000, 0.000000000000000000 ) ) ;
#104884 = AXIS2_PLACEMENT_3D ( 'NONE', #109614, #8169, #67067 ) ;
#104885 = CIRCLE ( 'NONE', #125815, 0.06509327318403745899 ) ;
#104887 = ADVANCED_FACE ( 'NONE', ( #4930 ), #46721, .T. ) ;
#104886 = CARTESIAN_POINT ( 'NONE',  ( 5.449999999999934452, 12.50000000000000000, 2.099970236277060032 ) ) ;
#104888 = ORIENTED_EDGE ( 'NONE', *, *, #26912, .F. ) ;
#104889 = AXIS2_PLACEMENT_3D ( 'NONE', #110748, #89824, #87875 ) ;
#104890 = CIRCLE ( 'NONE', #14989, 0.09999999999999982514 ) ;
#104891 = VECTOR ( 'NONE', #8230, 1000.000000000000000 ) ;
#104892 = ORIENTED_EDGE ( 'NONE', *, *, #6304, .F. ) ;
#104893 = CIRCLE ( 'NONE', #77701, 0.06509327318403745899 ) ;
#104894 = ORIENTED_EDGE ( 'NONE', *, *, #71394, .F. ) ;
#104895 = DIRECTION ( 'NONE',  ( 0.000000000000000000, 0.000000000000000000, -1.000000000000000000 ) ) ;
#104896 = CARTESIAN_POINT ( 'NONE',  ( -9.999999999999969802, 2.500000000000000000, 4.230127018922196669 ) ) ;
#104897 = CIRCLE ( 'NONE', #46415, 0.06509327318403745899 ) ;
#104898 = CARTESIAN_POINT ( 'NONE',  ( 184.7135416670080872, 4.367472073101518859, -7.564683531249999149 ) ) ;
#104899 = LINE ( 'NONE', #53250, #9256 ) ;
#104900 = CARTESIAN_POINT ( 'NONE',  ( 3.949999999999942446, 2.500000000000000000, -2.611473670974877592 ) ) ;
#104901 = LINE ( 'NONE', #114098, #108767 ) ;
#104902 = LINE ( 'NONE', #85276, #12023 ) ;
#104903 = ORIENTED_EDGE ( 'NONE', *, *, #45504, .T. ) ;
#104904 = DIRECTION ( 'NONE',  ( 0.000000000000000000, 0.000000000000000000, -1.000000000000000000 ) ) ;
#104905 = DIRECTION ( 'NONE',  ( 0.000000000000000000, 0.000000000000000000, -1.000000000000000000 ) ) ;
#104906 = ORIENTED_EDGE ( 'NONE', *, *, #48516, .T. ) ;
#104907 = CARTESIAN_POINT ( 'NONE',  ( -11.64999999999999858, 2.500000000000000000, -5.902370205355746968 ) ) ;
#104908 = VERTEX_POINT ( 'NONE', #96531 ) ;
#104909 = FACE_OUTER_BOUND ( 'NONE', #20881, .T. ) ;
#104910 = CIRCLE ( 'NONE', #121651, 0.06509327318403745899 ) ;
#104911 = CIRCLE ( 'NONE', #115367, 0.06509327318403745899 ) ;
#104912 = AXIS2_PLACEMENT_3D ( 'NONE', #41951, #81843, #121771 ) ;
#104913 = ORIENTED_EDGE ( 'NONE', *, *, #35826, .T. ) ;
#104914 = CARTESIAN_POINT ( 'NONE',  ( -14.14999999999998792, 2.500000000000000000, -1.572243186433547990 ) ) ;
#104915 = CARTESIAN_POINT ( 'NONE',  ( -9.600000000000008527, 2.500000000000000000, -5.022947341949749678 ) ) ;
#104916 = DIRECTION ( 'NONE',  ( 0.000000000000000000, 1.000000000000000000, 0.000000000000000000 ) ) ;
#104917 = ORIENTED_EDGE ( 'NONE', *, *, #65780, .F. ) ;
#104918 = EDGE_CURVE ( 'NONE', #27344, #22140, #19525, .T. ) ;
#104920 = CARTESIAN_POINT ( 'NONE',  ( -9.150000000000009237, 2.500000000000000000, -2.065063509461102065 ) ) ;
#104919 = CONICAL_SURFACE ( 'NONE', #121658, 0.09999999999999982514, 0.003490658503988666988 ) ;
#104921 = VECTOR ( 'NONE', #16333, 1000.000000000000000 ) ;
#104922 = AXIS2_PLACEMENT_3D ( 'NONE', #7281, #96307, #47235 ) ;
#104923 = CARTESIAN_POINT ( 'NONE',  ( 6.249999999999930722, 2.500000000000000000, -1.472243186433550122 ) ) ;
#104924 = AXIS2_PLACEMENT_3D ( 'NONE', #57190, #18550, #7433 ) ;
#104925 = EDGE_CURVE ( 'NONE', #62359, #100751, #73904, .T. ) ;
#104926 = ADVANCED_FACE ( 'NONE', ( #97202 ), #17455, .T. ) ;
#104927 = ORIENTED_EDGE ( 'NONE', *, *, #26123, .T. ) ;
#104928 = AXIS2_PLACEMENT_3D ( 'NONE', #75111, #124209, #65270 ) ;
#104929 = DIRECTION ( 'NONE',  ( -0.000000000000000000, 1.000000000000000000, -0.000000000000000000 ) ) ;
#104930 = ORIENTED_EDGE ( 'NONE', *, *, #72734, .T. ) ;
#104931 = ORIENTED_EDGE ( 'NONE', *, *, #9401, .F. ) ;
#104932 = DIRECTION ( 'NONE',  ( 0.000000000000000000, 1.000000000000000000, 0.000000000000000000 ) ) ;
#104933 = DIRECTION ( 'NONE',  ( 0.000000000000000000, 0.000000000000000000, -1.000000000000000000 ) ) ;
#104934 = EDGE_CURVE ( 'NONE', #66994, #38932, #118123, .T. ) ;
#104935 = ADVANCED_FACE ( 'NONE', ( #106372 ), #113615, .T. ) ;
#104936 = ORIENTED_EDGE ( 'NONE', *, *, #3292, .F. ) ;
#104937 = EDGE_CURVE ( 'NONE', #30053, #116514, #40484, .T. ) ;
#104938 = CARTESIAN_POINT ( 'NONE',  ( 5.199999999999931788, 12.50000000000000000, 4.611443907251934426 ) ) ;
#104939 = DIRECTION ( 'NONE',  ( -0.000000000000000000, 1.000000000000000000, -0.000000000000000000 ) ) ;
#104940 = ORIENTED_EDGE ( 'NONE', *, *, #12351, .T. ) ;
#104941 = LINE ( 'NONE', #36878, #105314 ) ;
#104942 = DIRECTION ( 'NONE',  ( 0.000000000000000000, 1.000000000000000000, 0.000000000000000000 ) ) ;
#104943 = FACE_OUTER_BOUND ( 'NONE', #102841, .T. ) ;
#104944 = DIRECTION ( 'NONE',  ( 0.000000000000000000, 1.000000000000000000, 0.000000000000000000 ) ) ;
#104945 = LINE ( 'NONE', #106257, #47234 ) ;
#104946 = DIRECTION ( 'NONE',  ( 0.000000000000000000, 0.000000000000000000, -1.000000000000000000 ) ) ;
#104947 = CIRCLE ( 'NONE', #397, 0.1000000000000002554 ) ;
#104948 = ORIENTED_EDGE ( 'NONE', *, *, #68957, .F. ) ;
#104949 = VERTEX_POINT ( 'NONE', #48108 ) ;
#104950 = ORIENTED_EDGE ( 'NONE', *, *, #117121, .T. ) ;
#104951 = ORIENTED_EDGE ( 'NONE', *, *, #20603, .F. ) ;
#104952 = CARTESIAN_POINT ( 'NONE',  ( -0.6000000000000388356, 2.500000000000000000, 4.676537180435972552 ) ) ;
#104953 = LINE ( 'NONE', #114786, #54045 ) ;
#104954 = DIRECTION ( 'NONE',  ( 0.000000000000000000, 1.000000000000000000, 0.000000000000000000 ) ) ;
#104955 = EDGE_LOOP ( 'NONE', ( #89026, #108223 ) ) ;
#104956 = FACE_BOUND ( 'NONE', #116496, .T. ) ;
#104957 = VECTOR ( 'NONE', #128126, 1000.000000000000000 ) ;
#104958 = CARTESIAN_POINT ( 'NONE',  ( -11.24999999999996447, 2.500000000000000000, -6.495190528383298911 ) ) ;
#104959 = CARTESIAN_POINT ( 'NONE',  ( -1.450000000000036371, 12.50000000000000000, 2.576566944158910744 ) ) ;
#104960 = CIRCLE ( 'NONE', #117563, 0.09999999999999982514 ) ;
#104962 = CARTESIAN_POINT ( 'NONE',  ( 6.049999999999934097, 12.50000000000000000, -2.511473670974877948 ) ) ;
#104961 = AXIS2_PLACEMENT_3D ( 'NONE', #15195, #76723, #7320 ) ;
#104963 = FACE_OUTER_BOUND ( 'NONE', #124076, .T. ) ;
#104964 = CARTESIAN_POINT ( 'NONE',  ( 8.949999999999917577, 12.50000000000000000, 6.213873640053558134 ) ) ;
#104965 = CARTESIAN_POINT ( 'NONE',  ( 2.949999999999945111, 2.500000000000000000, 2.065063509461097624 ) ) ;
#104966 = CARTESIAN_POINT ( 'NONE',  ( 4.399999999999939071, 2.500000000000000000, 0.3464101615137736845 ) ) ;
#104967 = CARTESIAN_POINT ( 'NONE',  ( 9.199999999999919353, 12.50000000000000000, -0.06509327318403970719 ) ) ;
#104968 = EDGE_CURVE ( 'NONE', #122603, #33034, #27809, .T. ) ;
#104969 = DIRECTION ( 'NONE',  ( 0.000000000000000000, 0.000000000000000000, 1.000000000000000000 ) ) ;
#104970 = VECTOR ( 'NONE', #85766, 1000.000000000000000 ) ;
#104971 = CARTESIAN_POINT ( 'NONE',  ( 2.499999999999947153, 2.500000000000000000, 0.5928203230275495006 ) ) ;
#104972 = CIRCLE ( 'NONE', #79949, 0.09999999999999982514 ) ;
#104973 = ORIENTED_EDGE ( 'NONE', *, *, #104659, .T. ) ;
#104974 = EDGE_LOOP ( 'NONE', ( #89454, #123507 ) ) ;
#104975 = ORIENTED_EDGE ( 'NONE', *, *, #33309, .T. ) ;
#104976 = EDGE_LOOP ( 'NONE', ( #81498, #76069, #61452, #36322 ) ) ;
#104977 = AXIS2_PLACEMENT_3D ( 'NONE', #69442, #110033, #60304 ) ;
#104978 = AXIS2_PLACEMENT_3D ( 'NONE', #92437, #61043, #3416 ) ;
#104979 = CARTESIAN_POINT ( 'NONE',  ( -10.40000000000000391, 2.500000000000000000, -3.737306695894645259 ) ) ;
#104980 = ORIENTED_EDGE ( 'NONE', *, *, #129554, .F. ) ;
#104981 = EDGE_CURVE ( 'NONE', #7558, #10391, #18633, .T. ) ;
#104982 = CARTESIAN_POINT ( 'NONE',  ( -14.34999999999998543, 2.500000000000000000, -1.818653347947323695 ) ) ;
#104983 = ADVANCED_FACE ( 'NONE', ( #78872 ), #55028, .T. ) ;
#104984 = ORIENTED_EDGE ( 'NONE', *, *, #112535, .F. ) ;
#104985 = EDGE_LOOP ( 'NONE', ( #102964, #90694, #6081, #123795 ) ) ;
#104986 = AXIS2_PLACEMENT_3D ( 'NONE', #87719, #13981, #106713 ) ;
#104987 = EDGE_CURVE ( 'NONE', #90431, #76513, #29126, .T. ) ;
#104988 = CARTESIAN_POINT ( 'NONE',  ( 5.399999999999934630, 12.50000000000000000, 0.7579135962115869374 ) ) ;
#104989 = AXIS2_PLACEMENT_3D ( 'NONE', #94193, #15617, #4490 ) ;
#104990 = CARTESIAN_POINT ( 'NONE',  ( 6.598553918451516509, -2.500000000000000888, 8.770211965177990621 ) ) ;
#104991 = DIRECTION ( 'NONE',  ( 0.000000000000000000, 0.000000000000000000, -1.000000000000000000 ) ) ;
#104992 = DIRECTION ( 'NONE',  ( -0.000000000000000000, -1.000000000000000000, -0.000000000000000000 ) ) ;
#104993 = EDGE_CURVE ( 'NONE', #26812, #50137, #88474, .T. ) ;
#104994 = CARTESIAN_POINT ( 'NONE',  ( -11.44999999999999751, 12.50000000000000000, 6.841600689897072485 ) ) ;
#104995 = EDGE_CURVE ( 'NONE', #88412, #46827, #17989, .T. ) ;
#104996 = ORIENTED_EDGE ( 'NONE', *, *, #4625, .T. ) ;
#104997 = EDGE_CURVE ( 'NONE', #110014, #76885, #48787, .T. ) ;
#104998 = ADVANCED_FACE ( 'NONE', ( #55975 ), #116186, .T. ) ;
#104999 = EDGE_LOOP ( 'NONE', ( #15118, #79341 ) ) ;
#105000 = EDGE_CURVE ( 'NONE', #23310, #119345, #124074, .T. ) ;
#105001 = ORIENTED_EDGE ( 'NONE', *, *, #38027, .F. ) ;
#105003 = ORIENTED_EDGE ( 'NONE', *, *, #102164, .T. ) ;
#105002 = CARTESIAN_POINT ( 'NONE',  ( -14.39999999999998614, 2.500000000000000000, -0.3464101615137760715 ) ) ;
#105004 = CARTESIAN_POINT ( 'NONE',  ( -14.79999999999998295, 12.50000000000000000, -0.3464101615137760715 ) ) ;
#105005 = EDGE_LOOP ( 'NONE', ( #82314, #20496 ) ) ;
#105006 = ORIENTED_EDGE ( 'NONE', *, *, #70170, .F. ) ;
#105007 = ADVANCED_FACE ( 'NONE', ( #87998 ), #86065, .T. ) ;
#105008 = CARTESIAN_POINT ( 'NONE',  ( 6.649999999999929301, 2.500000000000000000, 6.395190528383296602 ) ) ;
#105009 = CARTESIAN_POINT ( 'NONE',  ( 1.449999999999951772, 12.50000000000000000, -6.213873640053564351 ) ) ;
#105010 = CARTESIAN_POINT ( 'NONE',  ( -1.250000000000035749, 2.500000000000000000, -7.188010851410854052 ) ) ;
#105012 = DIRECTION ( 'NONE',  ( -0.000000000000000000, 1.000000000000000000, -0.000000000000000000 ) ) ;
#105011 = CONICAL_SURFACE ( 'NONE', #59062, 0.1000000000000000472, 0.003490658503988666988 ) ;
#105013 = VECTOR ( 'NONE', #28214, 1000.000000000000000 ) ;
#105014 = AXIS2_PLACEMENT_3D ( 'NONE', #95551, #97477, #87008 ) ;
#105015 = DIRECTION ( 'NONE',  ( 0.000000000000000000, 0.000000000000000000, -1.000000000000000000 ) ) ;
#105016 = ORIENTED_EDGE ( 'NONE', *, *, #54861, .F. ) ;
#105017 = LINE ( 'NONE', #55295, #115953 ) ;
#105018 = CONICAL_SURFACE ( 'NONE', #27753, 0.1000000000000002554, 0.003490658503988666988 ) ;
#105020 = ORIENTED_EDGE ( 'NONE', *, *, #16223, .F. ) ;
#105019 = AXIS2_PLACEMENT_3D ( 'NONE', #9762, #39886, #49707 ) ;
#105021 = CARTESIAN_POINT ( 'NONE',  ( 186.0416666666666572, -4.445597072760079982, 7.700000000000070344 ) ) ;
#105022 = AXIS2_PLACEMENT_3D ( 'NONE', #3914, #41286, #42579 ) ;
#105023 = ORIENTED_EDGE ( 'NONE', *, *, #46638, .T. ) ;
#105024 = DIRECTION ( 'NONE',  ( 0.000000000000000000, -0.9999939076577903929, 0.003490651415223739937 ) ) ;
#105025 = DIRECTION ( 'NONE',  ( -0.000000000000000000, 1.000000000000000000, -0.000000000000000000 ) ) ;
#105026 = AXIS2_PLACEMENT_3D ( 'NONE', #104982, #123354, #15310 ) ;
#105027 = AXIS2_PLACEMENT_3D ( 'NONE', #531, #20836, #29376 ) ;
#105028 = DIRECTION ( 'NONE',  ( -0.000000000000000000, -1.000000000000000000, -0.000000000000000000 ) ) ;
#105029 = ADVANCED_FACE ( 'NONE', ( #76275 ), #86509, .T. ) ;
#105030 = CARTESIAN_POINT ( 'NONE',  ( 9.349999999999916156, 2.500000000000000000, -1.718653347947326049 ) ) ;
#105031 = ORIENTED_EDGE ( 'NONE', *, *, #103912, .F. ) ;
#105032 = AXIS2_PLACEMENT_3D ( 'NONE', #35830, #14863, #26017 ) ;
#105033 = DIRECTION ( 'NONE',  ( 0.000000000000000000, 1.000000000000000000, 0.000000000000000000 ) ) ;
#105034 = DIRECTION ( 'NONE',  ( 0.000000000000000000, 1.000000000000000000, 0.000000000000000000 ) ) ;
#105035 = ORIENTED_EDGE ( 'NONE', *, *, #107130, .F. ) ;
#105036 = VERTEX_POINT ( 'NONE', #89953 ) ;
#105037 = ORIENTED_EDGE ( 'NONE', *, *, #73261, .F. ) ;
#105038 = FACE_OUTER_BOUND ( 'NONE', #56509, .T. ) ;
#105039 = CARTESIAN_POINT ( 'NONE',  ( -2.300000000000033129, 12.50000000000000000, 3.983716857408420076 ) ) ;
#105040 = CARTESIAN_POINT ( 'NONE',  ( 185.6093750003413732, 9.264065473108010111E-16, -7.564683531250000925 ) ) ;
#105041 = DIRECTION ( 'NONE',  ( -0.000000000000000000, 1.000000000000000000, -0.000000000000000000 ) ) ;
#105042 = AXIS2_PLACEMENT_3D ( 'NONE', #123922, #2211, #33627 ) ;
#105044 = ADVANCED_FACE ( 'NONE', ( #1570 ), #88573, .T. ) ;
#105043 = DIRECTION ( 'NONE',  ( 0.000000000000000000, 0.000000000000000000, -1.000000000000000000 ) ) ;
#105045 = CARTESIAN_POINT ( 'NONE',  ( -5.400000000000024336, 2.500000000000000000, -3.737306695894649700 ) ) ;
#105046 = AXIS2_PLACEMENT_3D ( 'NONE', #120053, #21200, #29735 ) ;
#105047 = ORIENTED_EDGE ( 'NONE', *, *, #24179, .T. ) ;
#105048 = CARTESIAN_POINT ( 'NONE',  ( -2.700000000000030820, 2.500000000000000000, -4.083716857408426826 ) ) ;
#105049 = CIRCLE ( 'NONE', #119724, 0.1000000000000002554 ) ;
#105050 = EDGE_LOOP ( 'NONE', ( #116808, #48475, #13756, #27322 ) ) ;
#105051 = EDGE_CURVE ( 'NONE', #33059, #39246, #19940, .T. ) ;
#105052 = DIRECTION ( 'NONE',  ( -4.274815082592931898E-19, -0.9999939076577903929, -0.003490651415223739937 ) ) ;
#105053 = CARTESIAN_POINT ( 'NONE',  ( 11.84999999999990727, 2.500000000000000000, 6.941600689897073018 ) ) ;
#105054 = CARTESIAN_POINT ( 'NONE',  ( -9.600000000000008527, 2.500000000000000000, -4.230127018922197557 ) ) ;
#105055 = AXIS2_PLACEMENT_3D ( 'NONE', #87378, #69031, #78883 ) ;
#105056 = AXIS2_PLACEMENT_3D ( 'NONE', #19551, #9085, #49036 ) ;
#105057 = ORIENTED_EDGE ( 'NONE', *, *, #121985, .F. ) ;
#105058 = AXIS2_PLACEMENT_3D ( 'NONE', #43355, #102887, #13866 ) ;
#105059 = VECTOR ( 'NONE', #34259, 1000.000000000000000 ) ;
#105060 = CARTESIAN_POINT ( 'NONE',  ( 0.8499999999999553468, 12.50000000000000000, 1.472243186433545459 ) ) ;
#105061 = CARTESIAN_POINT ( 'NONE',  ( 186.5312500006828031, 9.429780353434619030E-16, -7.700000000000000178 ) ) ;
#105062 = CONICAL_SURFACE ( 'NONE', #25658, 0.09999999999999982514, 0.003490658503988666988 ) ;
#105063 = VERTEX_POINT ( 'NONE', #59886 ) ;
#105065 = VECTOR ( 'NONE', #16389, 1000.000000000000000 ) ;
#105064 = FACE_OUTER_BOUND ( 'NONE', #29982, .T. ) ;
#105066 = ORIENTED_EDGE ( 'NONE', *, *, #8470, .T. ) ;
#105067 = AXIS2_PLACEMENT_3D ( 'NONE', #62219, #91660, #92298 ) ;
#105068 = ORIENTED_EDGE ( 'NONE', *, *, #72619, .F. ) ;
#105069 = AXIS2_PLACEMENT_3D ( 'NONE', #19686, #129022, #37401 ) ;
#105070 = CARTESIAN_POINT ( 'NONE',  ( 11.64999999999990266, 2.500000000000000000, -6.395190528383301931 ) ) ;
#105072 = ORIENTED_EDGE ( 'NONE', *, *, #49431, .F. ) ;
#105071 = CONICAL_SURFACE ( 'NONE', #48672, 0.09999999999999999167, 0.003490658503988666988 ) ;
#105073 = CARTESIAN_POINT ( 'NONE',  ( -11.44999999999999929, 2.500000000000000000, -1.818653347947322141 ) ) ;
#105074 = DIRECTION ( 'NONE',  ( -1.000000000000000000, 0.000000000000000000, 0.000000000000000000 ) ) ;
#105075 = FACE_OUTER_BOUND ( 'NONE', #75138, .T. ) ;
#105076 = EDGE_LOOP ( 'NONE', ( #13222, #45391, #5641, #109313 ) ) ;
#105077 = ADVANCED_FACE ( 'NONE', ( #61804 ), #42632, .T. ) ;
#105078 = FACE_BOUND ( 'NONE', #98768, .T. ) ;
#105079 = CIRCLE ( 'NONE', #17336, 0.06509327318403741736 ) ;
#105081 = EDGE_LOOP ( 'NONE', ( #8686, #80109, #126954, #127880 ) ) ;
#105080 = DIRECTION ( 'NONE',  ( 0.000000000000000000, 1.000000000000000000, 0.000000000000000000 ) ) ;
#105082 = FACE_OUTER_BOUND ( 'NONE', #12033, .T. ) ;
#105083 = CARTESIAN_POINT ( 'NONE',  ( -8.950000000000008171, 12.50000000000000000, -2.446380397790840266 ) ) ;
#105084 = ADVANCED_FACE ( 'NONE', ( #40889 ), #48888, .T. ) ;
#105085 = ORIENTED_EDGE ( 'NONE', *, *, #76588, .T. ) ;
#105086 = EDGE_LOOP ( 'NONE', ( #116511, #16466 ) ) ;
#105087 = ORIENTED_EDGE ( 'NONE', *, *, #8775, .T. ) ;
#105088 = LINE ( 'NONE', #24622, #14799 ) ;
#105089 = CARTESIAN_POINT ( 'NONE',  ( 2.500000000000002220, 2.500000000000000000, 9.000000000000005329 ) ) ;
#105090 = EDGE_CURVE ( 'NONE', #99080, #55788, #80272, .T. ) ;
#105091 = ADVANCED_FACE ( 'NONE', ( #110246 ), #61404, .T. ) ;
#105092 = CARTESIAN_POINT ( 'NONE',  ( -7.050000000000013145, 2.500000000000000000, 2.165063509461097713 ) ) ;
#105093 = AXIS2_PLACEMENT_3D ( 'NONE', #97498, #66095, #106033 ) ;
#105094 = EDGE_CURVE ( 'NONE', #68510, #26528, #81438, .T. ) ;
#105095 = FACE_BOUND ( 'NONE', #65620, .T. ) ;
#105097 = ADVANCED_FACE ( 'NONE', ( #61147 ), #2903, .T. ) ;
#105096 = VERTEX_POINT ( 'NONE', #50677 ) ;
#105098 = CARTESIAN_POINT ( 'NONE',  ( 185.8593750003413732, 0.000000000000000000, 7.564683531250000925 ) ) ;
#105099 = ADVANCED_FACE ( 'NONE', ( #2208 ), #76060, .T. ) ;
#105100 = CARTESIAN_POINT ( 'NONE',  ( 5.849999999999932143, 2.500000000000000000, 2.065063509461097624 ) ) ;
#105101 = LINE ( 'NONE', #46852, #89905 ) ;
#105102 = PLANE ( 'NONE',  #124425 ) ;
#105103 = VECTOR ( 'NONE', #39322, 1000.000000000000000 ) ;
#105104 = AXIS2_PLACEMENT_3D ( 'NONE', #126256, #14977, #16905 ) ;
#105105 = CARTESIAN_POINT ( 'NONE',  ( 4.599999999999938360, 12.50000000000000000, -0.06509327318403970719 ) ) ;
#105106 = DIRECTION ( 'NONE',  ( 0.000000000000000000, 1.000000000000000000, 0.000000000000000000 ) ) ;
#105107 = EDGE_CURVE ( 'NONE', #37993, #26037, #19627, .T. ) ;
#105108 = CARTESIAN_POINT ( 'NONE',  ( -4.121192902244064579E-14, 2.500000000000000000, 3.537306695894645081 ) ) ;
#105109 = LINE ( 'NONE', #37683, #113041 ) ;
#105110 = EDGE_CURVE ( 'NONE', #23819, #40507, #11395, .T. ) ;
#105112 = ADVANCED_FACE ( 'NONE', ( #32366 ), #103253, .T. ) ;
#105111 = VECTOR ( 'NONE', #76550, 1000.000000000000000 ) ;
#105114 = CARTESIAN_POINT ( 'NONE',  ( 127.5000000000000000, 0.000000000000000000, 0.000000000000000000 ) ) ;
#105113 = VECTOR ( 'NONE', #56743, 1000.000000000000000 ) ;
#105115 = VECTOR ( 'NONE', #117422, 1000.000000000000000 ) ;
#105116 = ORIENTED_EDGE ( 'NONE', *, *, #23123, .T. ) ;
#105117 = ORIENTED_EDGE ( 'NONE', *, *, #126318, .T. ) ;
#105118 = EDGE_LOOP ( 'NONE', ( #87634, #70997, #38066, #95164 ) ) ;
#105119 = ORIENTED_EDGE ( 'NONE', *, *, #72546, .F. ) ;
#105121 = EDGE_LOOP ( 'NONE', ( #126544, #122869, #104927, #81954 ) ) ;
#105120 = AXIS2_PLACEMENT_3D ( 'NONE', #91808, #100346, #51261 ) ;
#105122 = DIRECTION ( 'NONE',  ( -4.274815082592931898E-19, -0.9999939076577903929, -0.003490651415223739937 ) ) ;
#105123 = VECTOR ( 'NONE', #10749, 1000.000000000000000 ) ;
#105124 = DIRECTION ( 'NONE',  ( 0.000000000000000000, 0.000000000000000000, 1.000000000000000000 ) ) ;
#105125 = ORIENTED_EDGE ( 'NONE', *, *, #76880, .F. ) ;
#105126 = FACE_BOUND ( 'NONE', #56699, .T. ) ;
#105127 = CIRCLE ( 'NONE', #65319, 0.09999999999999982514 ) ;
#105128 = DIRECTION ( 'NONE',  ( -0.000000000000000000, -1.000000000000000000, -0.000000000000000000 ) ) ;
#105129 = LINE ( 'NONE', #107057, #38587 ) ;
#105130 = VERTEX_POINT ( 'NONE', #19264 ) ;
#105131 = CARTESIAN_POINT ( 'NONE',  ( 8.349999999999923261, 2.500000000000000000, -5.702370205355749455 ) ) ;
#105132 = CARTESIAN_POINT ( 'NONE',  ( -3.750000000000025757, 2.500000000000000000, 1.472243186433545459 ) ) ;
#105133 = PLANE ( 'NONE',  #45460 ) ;
#105134 = ORIENTED_EDGE ( 'NONE', *, *, #87652, .F. ) ;
#105135 = PLANE ( 'NONE',  #99380 ) ;
#105136 = CIRCLE ( 'NONE', #31904, 0.1000000000000002554 ) ;
#105137 = ORIENTED_EDGE ( 'NONE', *, *, #92396, .F. ) ;
#105138 = ORIENTED_EDGE ( 'NONE', *, *, #32601, .T. ) ;
#105139 = ORIENTED_EDGE ( 'NONE', *, *, #85301, .F. ) ;
#105140 = DIRECTION ( 'NONE',  ( 0.000000000000000000, 1.000000000000000000, 0.000000000000000000 ) ) ;
#105141 = DIRECTION ( 'NONE',  ( -0.000000000000000000, 1.000000000000000000, -0.000000000000000000 ) ) ;
#105142 = DIRECTION ( 'NONE',  ( 0.000000000000000000, 1.000000000000000000, 0.000000000000000000 ) ) ;
#105143 = VERTEX_POINT ( 'NONE', #59235 ) ;
#105144 = CARTESIAN_POINT ( 'NONE',  ( 12.64862127202694353, 1.500000000000319300, -8.430718248283330496 ) ) ;
#105146 = DIRECTION ( 'NONE',  ( 0.000000000000000000, 1.000000000000000000, 0.000000000000000000 ) ) ;
#105145 = CONICAL_SURFACE ( 'NONE', #94685, 0.1000000000000000472, 0.003490658503988666988 ) ;
#105147 = ADVANCED_FACE ( 'NONE', ( #9469 ), #89316, .T. ) ;
#105148 = CARTESIAN_POINT ( 'NONE',  ( -0.6500000000000394351, 2.500000000000000000, 2.511473670974873507 ) ) ;
#105149 = CARTESIAN_POINT ( 'NONE',  ( 187.1093750003414016, 9.264065473108010111E-16, -7.564683531250000925 ) ) ;
#105150 = CARTESIAN_POINT ( 'NONE',  ( -6.450000000000016165, 12.50000000000000000, 6.776507416713035248 ) ) ;
#105151 = CARTESIAN_POINT ( 'NONE',  ( -4.600000000000024514, 12.50000000000000000, -0.6928203230275542523 ) ) ;
#105152 = EDGE_CURVE ( 'NONE', #115126, #18421, #119400, .T. ) ;
#105153 = AXIS2_PLACEMENT_3D ( 'NONE', #47161, #86422, #75961 ) ;
#105154 = ORIENTED_EDGE ( 'NONE', *, *, #73771, .F. ) ;
#105155 = DIRECTION ( 'NONE',  ( -0.000000000000000000, -1.000000000000000000, -0.000000000000000000 ) ) ;
#105156 = CONICAL_SURFACE ( 'NONE', #73864, 0.1000000000000002554, 0.003490658503988666988 ) ;
#105157 = EDGE_CURVE ( 'NONE', #11967, #29091, #839, .T. ) ;
#105158 = CIRCLE ( 'NONE', #113475, 0.06509327318403745899 ) ;
#105159 = ORIENTED_EDGE ( 'NONE', *, *, #55855, .T. ) ;
#105160 = CIRCLE ( 'NONE', #121895, 0.1000000000000000472 ) ;
#105161 = ADVANCED_FACE ( 'NONE', ( #20582 ), #84370, .T. ) ;
#105162 = EDGE_LOOP ( 'NONE', ( #65122, #115317 ) ) ;
#105163 = DIRECTION ( 'NONE',  ( 0.000000000000000000, 0.000000000000000000, -1.000000000000000000 ) ) ;
#105164 = FACE_OUTER_BOUND ( 'NONE', #83310, .T. ) ;
#105165 = CARTESIAN_POINT ( 'NONE',  ( 4.349999999999937472, 2.500000000000000000, 6.841600689897072485 ) ) ;
#105166 = CARTESIAN_POINT ( 'NONE',  ( -2.300000000000033573, 2.500000000000000000, -3.983716857408426293 ) ) ;
#105167 = DIRECTION ( 'NONE',  ( 0.000000000000000000, 0.000000000000000000, 1.000000000000000000 ) ) ;
#105168 = CIRCLE ( 'NONE', #15260, 0.06509327318403745899 ) ;
#105169 = ORIENTED_EDGE ( 'NONE', *, *, #79140, .F. ) ;
#105170 = EDGE_CURVE ( 'NONE', #101388, #86861, #74004, .T. ) ;
#105171 = ORIENTED_EDGE ( 'NONE', *, *, #49242, .T. ) ;
#105172 = CARTESIAN_POINT ( 'NONE',  ( -3.750000000000027534, 12.50000000000000000, -1.407149913249512663 ) ) ;
#105174 = AXIS2_PLACEMENT_3D ( 'NONE', #32624, #111120, #81683 ) ;
#105173 = DIRECTION ( 'NONE',  ( -0.000000000000000000, 1.000000000000000000, -0.000000000000000000 ) ) ;
#105175 = VECTOR ( 'NONE', #67684, 1000.000000000000000 ) ;
#105176 = AXIS2_PLACEMENT_3D ( 'NONE', #120309, #72505, #40475 ) ;
#105177 = DIRECTION ( 'NONE',  ( 0.000000000000000000, -0.000000000000000000, 1.000000000000000000 ) ) ;
#105178 = ORIENTED_EDGE ( 'NONE', *, *, #11414, .T. ) ;
#105179 = EDGE_LOOP ( 'NONE', ( #108745, #61698 ) ) ;
#105180 = DIRECTION ( 'NONE',  ( 0.000000000000000000, 0.000000000000000000, 1.000000000000000000 ) ) ;
#105181 = CIRCLE ( 'NONE', #622, 0.09999999999999999167 ) ;
#105182 = ORIENTED_EDGE ( 'NONE', *, *, #109896, .F. ) ;
#105183 = DIRECTION ( 'NONE',  ( -4.274815082592931898E-19, -0.9999939076577903929, -0.003490651415223739937 ) ) ;
#105184 = CARTESIAN_POINT ( 'NONE',  ( -13.74999999999998934, 2.500000000000000000, -1.472243186433547901 ) ) ;
#105185 = ORIENTED_EDGE ( 'NONE', *, *, #108587, .T. ) ;
#105186 = AXIS2_PLACEMENT_3D ( 'NONE', #110783, #81345, #33537 ) ;
#105187 = FACE_OUTER_BOUND ( 'NONE', #91921, .T. ) ;
#105188 = DIRECTION ( 'NONE',  ( -0.000000000000000000, 1.000000000000000000, -0.000000000000000000 ) ) ;
#105189 = FACE_OUTER_BOUND ( 'NONE', #14020, .T. ) ;
#105190 = EDGE_CURVE ( 'NONE', #5028, #4651, #50939, .T. ) ;
#105191 = CARTESIAN_POINT ( 'NONE',  ( -4.150000000000025224, 12.50000000000000000, 5.802370205355744659 ) ) ;
#105192 = ORIENTED_EDGE ( 'NONE', *, *, #118368, .F. ) ;
#105193 = DIRECTION ( 'NONE',  ( 0.000000000000000000, 0.000000000000000000, -1.000000000000000000 ) ) ;
#105194 = DIRECTION ( 'NONE',  ( 0.000000000000000000, 0.000000000000000000, 1.000000000000000000 ) ) ;
#105195 = EDGE_LOOP ( 'NONE', ( #46572, #89987, #15232, #95999 ) ) ;
#105196 = EDGE_LOOP ( 'NONE', ( #47694, #99727, #86317, #51428 ) ) ;
#105197 = CIRCLE ( 'NONE', #126129, 0.06509327318403745899 ) ;
#105198 = CONICAL_SURFACE ( 'NONE', #92684, 0.1000000000000002554, 0.003490658503988666988 ) ;
#105199 = DIRECTION ( 'NONE',  ( 0.000000000000000000, 1.000000000000000000, 0.000000000000000000 ) ) ;
#105200 = DIRECTION ( 'NONE',  ( -0.000000000000000000, 1.000000000000000000, -0.000000000000000000 ) ) ;
#105201 = DIRECTION ( 'NONE',  ( 0.000000000000000000, 1.000000000000000000, 0.000000000000000000 ) ) ;
#105202 = FACE_OUTER_BOUND ( 'NONE', #1968, .T. ) ;
#105203 = CARTESIAN_POINT ( 'NONE',  ( 8.099999999999921485, 12.50000000000000000, 0.3464101615137735735 ) ) ;
#105204 = DIRECTION ( 'NONE',  ( 0.000000000000000000, 0.000000000000000000, 1.000000000000000000 ) ) ;
#105205 = VECTOR ( 'NONE', #97836, 1000.000000000000000 ) ;
#105207 = EDGE_CURVE ( 'NONE', #55907, #24394, #63730, .T. ) ;
#105206 = DIRECTION ( 'NONE',  ( 0.000000000000000000, 0.000000000000000000, -1.000000000000000000 ) ) ;
#105208 = AXIS2_PLACEMENT_3D ( 'NONE', #47674, #88199, #56813 ) ;
#105209 = FACE_OUTER_BOUND ( 'NONE', #62696, .T. ) ;
#105210 = DIRECTION ( 'NONE',  ( 0.000000000000000000, 0.000000000000000000, -1.000000000000000000 ) ) ;
#105212 = VECTOR ( 'NONE', #69251, 1000.000000000000000 ) ;
#105211 = DIRECTION ( 'NONE',  ( -0.000000000000000000, -1.000000000000000000, -0.000000000000000000 ) ) ;
#105213 = CIRCLE ( 'NONE', #107353, 0.06509327318403741736 ) ;
#105214 = DIRECTION ( 'NONE',  ( 0.000000000000000000, 0.000000000000000000, 1.000000000000000000 ) ) ;
#105215 = EDGE_LOOP ( 'NONE', ( #34892, #62992 ) ) ;
#105216 = VECTOR ( 'NONE', #124402, 1000.000000000000000 ) ;
#105217 = AXIS2_PLACEMENT_3D ( 'NONE', #110173, #20506, #49981 ) ;
#105218 = AXIS2_PLACEMENT_3D ( 'NONE', #62424, #51322, #111497 ) ;
#105219 = ORIENTED_EDGE ( 'NONE', *, *, #65699, .T. ) ;
#105220 = VECTOR ( 'NONE', #84231, 1000.000000000000000 ) ;
#105221 = CONICAL_SURFACE ( 'NONE', #50851, 0.1000000000000002554, 0.003490658503988666988 ) ;
#105222 = ORIENTED_EDGE ( 'NONE', *, *, #82567, .T. ) ;
#105223 = EDGE_CURVE ( 'NONE', #42007, #16778, #14599, .T. ) ;
#105224 = CARTESIAN_POINT ( 'NONE',  ( 5.449999999999934452, 2.500000000000000000, 2.065063509461097624 ) ) ;
#105225 = DIRECTION ( 'NONE',  ( 0.000000000000000000, 1.000000000000000000, 0.000000000000000000 ) ) ;
#105226 = CARTESIAN_POINT ( 'NONE',  ( 6.649999999999930189, 12.50000000000000000, 5.802370205355744659 ) ) ;
#105227 = EDGE_LOOP ( 'NONE', ( #1161, #86384 ) ) ;
#105228 = DIRECTION ( 'NONE',  ( -0.000000000000000000, -1.000000000000000000, -0.000000000000000000 ) ) ;
#105229 = FACE_OUTER_BOUND ( 'NONE', #116851, .T. ) ;
#105231 = EDGE_LOOP ( 'NONE', ( #92528, #332 ) ) ;
#105230 = DIRECTION ( 'NONE',  ( 0.000000000000000000, 1.000000000000000000, 0.000000000000000000 ) ) ;
#105232 =( BOUNDED_SURFACE ( )  B_SPLINE_SURFACE ( 3, 2, ( 
 ( #43002, #40410, #92057 ),
 ( #60057, #2369, #42328 ),
 ( #22057, #3054, #20751 ),
 ( #52782, #90114, #92717 ),
 ( #61970, #1740, #60692 ),
 ( #31231, #122184, #50861 ),
 ( #101893, #82260, #112358 ),
 ( #82903, #71132, #72436 ),
 ( #22703, #122822, #51510 ),
 ( #62624, #99962, #12833 ),
 ( #33165, #80327, #73074 ),
 ( #100587, #10290, #50228 ),
 ( #443, #1103, #120251 ),
 ( #70492, #110415, #41062 ),
 ( #101244, #80967, #120879 ),
 ( #111037, #21388, #61328 ),
 ( #91424, #41698, #105759 ),
 ( #65816, #14761, #4297 ),
 ( #125397, #33789, #83547 ),
 ( #105089, #114913, #85464 ) ),
 .UNSPECIFIED., .F., .F., .F. ) 
 B_SPLINE_SURFACE_WITH_KNOTS ( ( 4, 2, 2, 2, 2, 2, 2, 2, 2, 4 ),
 ( 3, 3 ),
 ( 5.475220971051797392E-18, 0.0008832438798941970272, 0.001766487759788388633, 0.002649731639682580131, 0.003532975519576771629, 0.005299463279365155058, 0.007065951039153538053, 0.008832438798941921049, 0.01059892655873030491, 0.01413190207830707090 ),
 ( 0.000000000000000000, 1.000000000000000000 ),
 .UNSPECIFIED. ) 
 GEOMETRIC_REPRESENTATION_ITEM ( )  RATIONAL_B_SPLINE_SURFACE ( (
 ( 1.000000000000000000, 0.7071067811865472397, 1.000000000000000000),
 ( 1.000000000000000000, 0.7071067811865472397, 1.000000000000000000),
 ( 1.000000000000000000, 0.7071067811865476838, 1.000000000000000000),
 ( 1.000000000000000000, 0.7071067811865476838, 1.000000000000000000),
 ( 1.000000000000000000, 0.7071067811865471286, 1.000000000000000000),
 ( 1.000000000000000000, 0.7071067811865471286, 1.000000000000000000),
 ( 1.000000000000000000, 0.7071067811865471286, 1.000000000000000000),
 ( 1.000000000000000000, 0.7071067811865471286, 1.000000000000000000),
 ( 1.000000000000000000, 0.7071067811865476838, 1.000000000000000000),
 ( 1.000000000000000000, 0.7071067811865476838, 1.000000000000000000),
 ( 1.000000000000000000, 0.7071067811865476838, 1.000000000000000000),
 ( 1.000000000000000000, 0.7071067811865476838, 1.000000000000000000),
 ( 1.000000000000000000, 0.7071067811865473507, 1.000000000000000000),
 ( 1.000000000000000000, 0.7071067811865473507, 1.000000000000000000),
 ( 1.000000000000000000, 0.7071067811865473507, 1.000000000000000000),
 ( 1.000000000000000000, 0.7071067811865473507, 1.000000000000000000),
 ( 1.000000000000000000, 0.7071067811865479058, 1.000000000000000000),
 ( 1.000000000000000000, 0.7071067811865479058, 1.000000000000000000),
 ( 1.000000000000000000, 0.7071067811865473507, 1.000000000000000000),
 ( 1.000000000000000000, 0.7071067811865473507, 1.000000000000000000) ) ) 
 REPRESENTATION_ITEM ( '' )  SURFACE ( )  );
#105234 = FACE_OUTER_BOUND ( 'NONE', #117814, .T. ) ;
#105233 = AXIS2_PLACEMENT_3D ( 'NONE', #46031, #85922, #125855 ) ;
#105235 = ORIENTED_EDGE ( 'NONE', *, *, #21395, .T. ) ;
#105236 = EDGE_CURVE ( 'NONE', #71030, #120080, #9156, .T. ) ;
#105237 = ORIENTED_EDGE ( 'NONE', *, *, #128287, .T. ) ;
#105238 = ORIENTED_EDGE ( 'NONE', *, *, #18256, .T. ) ;
#105239 = ORIENTED_EDGE ( 'NONE', *, *, #112845, .F. ) ;
#105240 = DIRECTION ( 'NONE',  ( 0.000000000000000000, 0.000000000000000000, 1.000000000000000000 ) ) ;
#105242 = AXIS2_PLACEMENT_3D ( 'NONE', #125523, #123585, #64671 ) ;
#105241 = CARTESIAN_POINT ( 'NONE',  ( 10.19999999999991047, 12.50000000000000000, 4.676537180435972552 ) ) ;
#105243 = DIRECTION ( 'NONE',  ( -0.000000000000000000, 1.000000000000000000, -0.000000000000000000 ) ) ;
#105244 = CIRCLE ( 'NONE', #59303, 0.06509327318403745899 ) ;
#105245 = CARTESIAN_POINT ( 'NONE',  ( -8.950000000000004619, 2.500000000000000000, 6.148780366869520897 ) ) ;
#105246 = CIRCLE ( 'NONE', #111506, 0.06509327318403745899 ) ;
#105247 = EDGE_LOOP ( 'NONE', ( #76859, #88414, #5591, #5361 ) ) ;
#105248 = EDGE_CURVE ( 'NONE', #26576, #75844, #112182, .T. ) ;
#105249 = CARTESIAN_POINT ( 'NONE',  ( 11.24999999999991118, 12.50000000000000000, -2.857883832488653741 ) ) ;
#105250 = ORIENTED_EDGE ( 'NONE', *, *, #32810, .F. ) ;
#105251 = CARTESIAN_POINT ( 'NONE',  ( 43.31214921624317071, -3.511364963957428031, -3.941696051812598078 ) ) ;
#105252 = DIRECTION ( 'NONE',  ( 0.000000000000000000, 0.000000000000000000, 1.000000000000000000 ) ) ;
#105253 = CARTESIAN_POINT ( 'NONE',  ( -13.34999999999999076, 12.50000000000000000, 2.099970236277064028 ) ) ;
#105254 = CARTESIAN_POINT ( 'NONE',  ( 17.33812564108897902, -2.538896947917432811, 5.379288978441534752 ) ) ;
#105256 = EDGE_CURVE ( 'NONE', #21947, #119719, #78121, .T. ) ;
#105255 = CIRCLE ( 'NONE', #48842, 0.06509327318403745899 ) ;
#105257 = VERTEX_POINT ( 'NONE', #72903 ) ;
#105258 = CIRCLE ( 'NONE', #65549, 0.09999999999999982514 ) ;
#105259 = EDGE_LOOP ( 'NONE', ( #82764, #101132, #22539, #58948 ) ) ;
#105260 = VERTEX_POINT ( 'NONE', #83372 ) ;
#105261 = FACE_OUTER_BOUND ( 'NONE', #68493, .T. ) ;
#105262 = CARTESIAN_POINT ( 'NONE',  ( -6.450000000000014388, 12.50000000000000000, 1.818653347947321475 ) ) ;
#105263 = ADVANCED_FACE ( 'NONE', ( #104909 ), #21689, .T. ) ;
#105264 = ADVANCED_FACE ( 'NONE', ( #4133 ), #13319, .T. ) ;
#105265 = DIRECTION ( 'NONE',  ( -0.000000000000000000, -1.000000000000000000, -0.000000000000000000 ) ) ;
#105266 = EDGE_CURVE ( 'NONE', #77033, #36233, #3516, .T. ) ;
#105267 = FACE_BOUND ( 'NONE', #127064, .T. ) ;
#105269 = ADVANCED_FACE ( 'NONE', ( #43458 ), #34218, .T. ) ;
#105268 = AXIS2_PLACEMENT_3D ( 'NONE', #122868, #32574, #100165 ) ;
#105270 = CARTESIAN_POINT ( 'NONE',  ( -3.150000000000033218, 2.500000000000000000, -6.841600689897078702 ) ) ;
#105271 = LINE ( 'NONE', #8348, #90492 ) ;
#105272 = CARTESIAN_POINT ( 'NONE',  ( 3.149999999999944400, 12.50000000000000000, 1.753560074763284016 ) ) ;
#105273 = FACE_OUTER_BOUND ( 'NONE', #6451, .T. ) ;
#105274 = CIRCLE ( 'NONE', #29978, 0.1000000000000000472 ) ;
#105275 = AXIS2_PLACEMENT_3D ( 'NONE', #10470, #120438, #77922 ) ;
#105276 = EDGE_CURVE ( 'NONE', #53613, #34661, #32165, .T. ) ;
#105277 = CARTESIAN_POINT ( 'NONE',  ( -8.950000000000011724, 2.500000000000000000, -6.048780366869521252 ) ) ;
#105278 = EDGE_CURVE ( 'NONE', #95476, #75694, #105303, .T. ) ;
#105279 = LINE ( 'NONE', #17526, #117752 ) ;
#105280 = AXIS2_PLACEMENT_3D ( 'NONE', #57976, #97884, #68423 ) ;
#105281 = EDGE_CURVE ( 'NONE', #14873, #11223, #40672, .T. ) ;
#105282 = DIRECTION ( 'NONE',  ( 0.000000000000000000, 0.000000000000000000, -1.000000000000000000 ) ) ;
#105283 = CIRCLE ( 'NONE', #107429, 0.1000000000000002554 ) ;
#105284 = EDGE_CURVE ( 'NONE', #110245, #89903, #84469, .T. ) ;
#105285 = ADVANCED_FACE ( 'NONE', ( #102367 ), #80367, .T. ) ;
#105286 = FACE_OUTER_BOUND ( 'NONE', #122840, .T. ) ;
#105287 = ORIENTED_EDGE ( 'NONE', *, *, #122850, .F. ) ;
#105288 = ORIENTED_EDGE ( 'NONE', *, *, #94437, .F. ) ;
#105289 = VERTEX_POINT ( 'NONE', #73525 ) ;
#105290 = EDGE_LOOP ( 'NONE', ( #116779, #35286 ) ) ;
#105291 = DIRECTION ( 'NONE',  ( 0.000000000000000000, 0.000000000000000000, -1.000000000000000000 ) ) ;
#105292 = FACE_BOUND ( 'NONE', #4175, .T. ) ;
#105293 = ADVANCED_FACE ( 'NONE', ( #4775 ), #57371, .T. ) ;
#105294 = DIRECTION ( 'NONE',  ( -4.274815082592931898E-19, -0.9999939076577903929, -0.003490651415223739937 ) ) ;
#105296 = ORIENTED_EDGE ( 'NONE', *, *, #102441, .T. ) ;
#105295 = CIRCLE ( 'NONE', #96976, 0.09999999999999999167 ) ;
#105298 = AXIS2_PLACEMENT_3D ( 'NONE', #52339, #81787, #51073 ) ;
#105297 = CARTESIAN_POINT ( 'NONE',  ( 59.74180401152909781, 3.401974578027094243, 5.439313020113218045 ) ) ;
#105299 = DIRECTION ( 'NONE',  ( -0.000000000000000000, -1.000000000000000000, -0.000000000000000000 ) ) ;
#105300 = VERTEX_POINT ( 'NONE', #12671 ) ;
#105301 = DIRECTION ( 'NONE',  ( 0.000000000000000000, 1.000000000000000000, 0.000000000000000000 ) ) ;
#105302 = DIRECTION ( 'NONE',  ( 0.000000000000000000, 0.000000000000000000, 1.000000000000000000 ) ) ;
#105303 = CIRCLE ( 'NONE', #117901, 0.1000000000000002554 ) ;
#105304 = AXIS2_PLACEMENT_3D ( 'NONE', #16800, #56725, #18760 ) ;
#105305 = CIRCLE ( 'NONE', #109416, 0.1000000000000000472 ) ;
#105306 = CIRCLE ( 'NONE', #743, 0.1000000000000002554 ) ;
#105307 = AXIS2_PLACEMENT_3D ( 'NONE', #77374, #117259, #38093 ) ;
#105308 = ORIENTED_EDGE ( 'NONE', *, *, #113819, .F. ) ;
#105309 = CARTESIAN_POINT ( 'NONE',  ( 1.899999999999949507, 12.50000000000000000, 3.983716857408420964 ) ) ;
#105310 = CARTESIAN_POINT ( 'NONE',  ( 2.099999999999950351, 2.500000000000000000, -0.5928203230275541635 ) ) ;
#105311 = AXIS2_PLACEMENT_3D ( 'NONE', #12344, #22840, #20245 ) ;
#105313 = ORIENTED_EDGE ( 'NONE', *, *, #36439, .T. ) ;
#105312 = VECTOR ( 'NONE', #37416, 1000.000000000000000 ) ;
#105314 = VECTOR ( 'NONE', #45411, 1000.000000000000000 ) ;
#105315 = CARTESIAN_POINT ( 'NONE',  ( -7.500000000000015099, 2.500000000000000000, -5.022947341949754119 ) ) ;
#105316 = CARTESIAN_POINT ( 'NONE',  ( 13.09999999999990195, 2.500000000000000000, -4.576537180435978236 ) ) ;
#105317 = LINE ( 'NONE', #35925, #11697 ) ;
#105319 = ORIENTED_EDGE ( 'NONE', *, *, #16278, .T. ) ;
#105318 = AXIS2_PLACEMENT_3D ( 'NONE', #113245, #45171, #102772 ) ;
#105320 = ORIENTED_EDGE ( 'NONE', *, *, #15389, .F. ) ;
#105321 = DIRECTION ( 'NONE',  ( -0.000000000000000000, 1.000000000000000000, -0.000000000000000000 ) ) ;
#105322 = VERTEX_POINT ( 'NONE', #2873 ) ;
#105323 = CARTESIAN_POINT ( 'NONE',  ( 6.649999999999930189, 2.500000000000000000, 7.188010851410848723 ) ) ;
#105324 = CARTESIAN_POINT ( 'NONE',  ( 4.399999999999940847, 2.500000000000000000, -3.883716857408426648 ) ) ;
#105325 = EDGE_CURVE ( 'NONE', #25509, #92080, #82738, .T. ) ;
#105326 = ORIENTED_EDGE ( 'NONE', *, *, #115710, .F. ) ;
#105328 = EDGE_CURVE ( 'NONE', #35395, #103698, #101199, .T. ) ;
#105327 = DIRECTION ( 'NONE',  ( 0.000000000000000000, 1.000000000000000000, 0.000000000000000000 ) ) ;
#105329 = DIRECTION ( 'NONE',  ( 0.000000000000000000, -0.9999939076577903929, 0.003490651415223739937 ) ) ;
#105330 = CARTESIAN_POINT ( 'NONE',  ( -7.100000000000017408, 2.500000000000000000, -0.7928203230275543412 ) ) ;
#105331 = DIRECTION ( 'NONE',  ( 0.000000000000000000, 1.000000000000000000, 0.000000000000000000 ) ) ;
#105332 = DIRECTION ( 'NONE',  ( 0.000000000000000000, -0.000000000000000000, 1.000000000000000000 ) ) ;
#105333 = CIRCLE ( 'NONE', #27966, 0.1000000000000000056 ) ;
#105334 = EDGE_CURVE ( 'NONE', #112676, #92091, #82432, .T. ) ;
#105335 = ORIENTED_EDGE ( 'NONE', *, *, #64653, .F. ) ;
#105336 = ORIENTED_EDGE ( 'NONE', *, *, #27251, .F. ) ;
#105337 = DIRECTION ( 'NONE',  ( 0.000000000000000000, -0.000000000000000000, 1.000000000000000000 ) ) ;
#105338 = ADVANCED_FACE ( 'NONE', ( #47309 ), #90815, .T. ) ;
#105339 = DIRECTION ( 'NONE',  ( 0.000000000000000000, -0.000000000000000000, 1.000000000000000000 ) ) ;
#105340 = DIRECTION ( 'NONE',  ( 0.000000000000000000, 0.000000000000000000, -1.000000000000000000 ) ) ;
#105342 = ORIENTED_EDGE ( 'NONE', *, *, #8226, .T. ) ;
#105341 = ORIENTED_EDGE ( 'NONE', *, *, #30969, .F. ) ;
#105343 = EDGE_LOOP ( 'NONE', ( #116208, #55890 ) ) ;
#105344 = DIRECTION ( 'NONE',  ( 0.000000000000000000, 0.000000000000000000, 1.000000000000000000 ) ) ;
#105345 = CIRCLE ( 'NONE', #40619, 0.06509327318403745899 ) ;
#105346 = DIRECTION ( 'NONE',  ( 0.000000000000000000, 1.000000000000000000, 0.000000000000000000 ) ) ;
#105347 = CARTESIAN_POINT ( 'NONE',  ( 3.949999999999942446, 12.50000000000000000, -6.841600689897078702 ) ) ;
#105348 = SURFACE_STYLE_USAGE ( .BOTH. , #85695 ) ;
#105349 = DIRECTION ( 'NONE',  ( 0.000000000000000000, 0.000000000000000000, 1.000000000000000000 ) ) ;
#105350 = DIRECTION ( 'NONE',  ( -0.000000000000000000, -1.000000000000000000, -0.000000000000000000 ) ) ;
#105351 = DIRECTION ( 'NONE',  ( 0.000000000000000000, -0.9999939076577903929, 0.003490651415223739937 ) ) ;
#105352 = DIRECTION ( 'NONE',  ( 0.000000000000000000, 0.000000000000000000, 1.000000000000000000 ) ) ;
#105353 = CARTESIAN_POINT ( 'NONE',  ( 3.749999999999978684, 2.500000000000000000, -2.165063509461101710 ) ) ;
#105354 = VECTOR ( 'NONE', #68565, 1000.000000000000000 ) ;
#105355 = FACE_OUTER_BOUND ( 'NONE', #118242, .T. ) ;
#105356 = AXIS2_PLACEMENT_3D ( 'NONE', #64434, #63806, #24521 ) ;
#105357 = ORIENTED_EDGE ( 'NONE', *, *, #17757, .T. ) ;
#105358 = CONICAL_SURFACE ( 'NONE', #119931, 0.1000000000000002554, 0.003490658503988666988 ) ;
#105359 = DIRECTION ( 'NONE',  ( 0.000000000000000000, 0.000000000000000000, 1.000000000000000000 ) ) ;
#105360 = ORIENTED_EDGE ( 'NONE', *, *, #79134, .T. ) ;
#105361 = ORIENTED_EDGE ( 'NONE', *, *, #90299, .F. ) ;
#105362 = DIRECTION ( 'NONE',  ( -0.000000000000000000, -1.000000000000000000, -0.000000000000000000 ) ) ;
#105363 = CARTESIAN_POINT ( 'NONE',  ( 8.349999999999923261, 12.50000000000000000, -6.560283801567339701 ) ) ;
#105364 = PLANE ( 'NONE',  #128021 ) ;
#105365 = ADVANCED_FACE ( 'NONE', ( #55832 ), #5030, .T. ) ;
#105366 = DIRECTION ( 'NONE',  ( 1.000000000000000000, 0.000000000000000000, 0.000000000000000000 ) ) ;
#105367 = CARTESIAN_POINT ( 'NONE',  ( 0.8499999999999545697, 12.50000000000000000, 2.857883832488649301 ) ) ;
#105368 = AXIS2_PLACEMENT_3D ( 'NONE', #124590, #65656, #64368 ) ;
#105369 = DIRECTION ( 'NONE',  ( 0.000000000000000000, 0.000000000000000000, -1.000000000000000000 ) ) ;
#105370 = AXIS2_PLACEMENT_3D ( 'NONE', #112786, #110205, #11355 ) ;
#105371 = DIRECTION ( 'NONE',  ( 0.000000000000000000, 1.000000000000000000, 0.000000000000000000 ) ) ;
#105372 = ORIENTED_EDGE ( 'NONE', *, *, #25234, .T. ) ;
#105373 = CARTESIAN_POINT ( 'NONE',  ( -5.650000000000023448, 2.500000000000000000, -6.741600689897078169 ) ) ;
#105374 = VECTOR ( 'NONE', #102410, 1000.000000000000000 ) ;
#105375 = AXIS2_PLACEMENT_3D ( 'NONE', #98023, #19462, #128809 ) ;
#105376 = CARTESIAN_POINT ( 'NONE',  ( 8.099999999999921485, 2.500000000000000000, -0.4464101615137783252 ) ) ;
#105377 = ORIENTED_EDGE ( 'NONE', *, *, #105572, .T. ) ;
#105378 = ORIENTED_EDGE ( 'NONE', *, *, #50410, .T. ) ;
#105379 = EDGE_LOOP ( 'NONE', ( #91545, #74477, #11650, #12735 ) ) ;
#105380 = EDGE_CURVE ( 'NONE', #39516, #58339, #78216, .T. ) ;
#105382 = EDGE_LOOP ( 'NONE', ( #14516, #64980 ) ) ;
#105381 = EDGE_CURVE ( 'NONE', #98489, #105260, #94935, .T. ) ;
#105383 = CARTESIAN_POINT ( 'NONE',  ( 187.5000000000000000, 0.000000000000000000, 0.000000000000000000 ) ) ;
#105384 = DIRECTION ( 'NONE',  ( 0.000000000000000000, 0.000000000000000000, -1.000000000000000000 ) ) ;
#105385 = CARTESIAN_POINT ( 'NONE',  ( -10.60000000000000142, 2.500000000000000000, 0.4464101615137736623 ) ) ;
#105386 = DIRECTION ( 'NONE',  ( 0.000000000000000000, 1.000000000000000000, 0.000000000000000000 ) ) ;
#105387 = AXIS2_PLACEMENT_3D ( 'NONE', #120987, #106800, #17103 ) ;
#105388 = DIRECTION ( 'NONE',  ( -0.000000000000000000, 1.000000000000000000, -0.000000000000000000 ) ) ;
#105389 = EDGE_LOOP ( 'NONE', ( #89362, #38358, #16002, #94818 ) ) ;
#105391 = AXIS2_PLACEMENT_3D ( 'NONE', #23246, #12134, #51451 ) ;
#105390 = DIRECTION ( 'NONE',  ( 0.000000000000000000, 0.000000000000000000, 1.000000000000000000 ) ) ;
#105392 = AXIS2_PLACEMENT_3D ( 'NONE', #112409, #122235, #11617 ) ;
#105393 = ADVANCED_FACE ( 'NONE', ( #127794 ), #15495, .T. ) ;
#105394 = LINE ( 'NONE', #83810, #41116 ) ;
#105395 = FACE_OUTER_BOUND ( 'NONE', #48707, .T. ) ;
#105396 = ORIENTED_EDGE ( 'NONE', *, *, #123153, .T. ) ;
#105397 = CONICAL_SURFACE ( 'NONE', #86601, 0.09999999999999982514, 0.003490658503988666988 ) ;
#105398 = VECTOR ( 'NONE', #4907, 1000.000000000000000 ) ;
#105399 = VECTOR ( 'NONE', #78202, 1000.000000000000000 ) ;
#105400 = EDGE_LOOP ( 'NONE', ( #57581, #92267, #60811, #43277 ) ) ;
#105401 = CIRCLE ( 'NONE', #48980, 0.1000000000000002554 ) ;
#105402 = ORIENTED_EDGE ( 'NONE', *, *, #69082, .T. ) ;
#105403 = CARTESIAN_POINT ( 'NONE',  ( 11.44999999999990870, 2.500000000000000000, -1.918653347947326004 ) ) ;
#105404 = DIRECTION ( 'NONE',  ( 0.000000000000000000, 0.000000000000000000, -1.000000000000000000 ) ) ;
#105405 = DIRECTION ( 'NONE',  ( 0.000000000000000000, 1.000000000000000000, 0.000000000000000000 ) ) ;
#105406 = CONICAL_SURFACE ( 'NONE', #15505, 0.09999999999999982514, 0.003490658503988666988 ) ;
#105407 = AXIS2_PLACEMENT_3D ( 'NONE', #110516, #60779, #100681 ) ;
#105408 = AXIS2_PLACEMENT_3D ( 'NONE', #113330, #4017, #92399 ) ;
#105409 = AXIS2_PLACEMENT_3D ( 'NONE', #83651, #64641, #12316 ) ;
#105410 = EDGE_LOOP ( 'NONE', ( #88941, #76164 ) ) ;
#105411 = DIRECTION ( 'NONE',  ( 0.000000000000000000, 0.000000000000000000, 1.000000000000000000 ) ) ;
#105412 = CARTESIAN_POINT ( 'NONE',  ( 9.349999999999919709, 12.50000000000000000, 1.753560074763284016 ) ) ;
#105413 = DIRECTION ( 'NONE',  ( -0.000000000000000000, 1.000000000000000000, -0.000000000000000000 ) ) ;
#105414 = DIRECTION ( 'NONE',  ( 0.000000000000000000, 0.000000000000000000, 1.000000000000000000 ) ) ;
#105415 = DIRECTION ( 'NONE',  ( 0.000000000000000000, 1.000000000000000000, 0.000000000000000000 ) ) ;
#105416 = EDGE_CURVE ( 'NONE', #10677, #30501, #36209, .T. ) ;
#105417 = VERTEX_POINT ( 'NONE', #46028 ) ;
#105418 = DIRECTION ( 'NONE',  ( 0.000000000000000000, 0.000000000000000000, 1.000000000000000000 ) ) ;
#105419 = ORIENTED_EDGE ( 'NONE', *, *, #36444, .T. ) ;
#105420 = ORIENTED_EDGE ( 'NONE', *, *, #16789, .F. ) ;
#105421 = ORIENTED_EDGE ( 'NONE', *, *, #126202, .F. ) ;
#105422 = EDGE_CURVE ( 'NONE', #7810, #72282, #76768, .T. ) ;
#105423 = DIRECTION ( 'NONE',  ( 0.000000000000000000, 0.000000000000000000, 1.000000000000000000 ) ) ;
#105424 = EDGE_CURVE ( 'NONE', #87604, #109569, #25985, .T. ) ;
#105425 = FACE_BOUND ( 'NONE', #77473, .T. ) ;
#105426 = ADVANCED_FACE ( 'NONE', ( #116041 ), #126330, .T. ) ;
#105427 = CARTESIAN_POINT ( 'NONE',  ( 3.349999999999945466, 2.500000000000000000, -7.088010851410853519 ) ) ;
#105428 = VECTOR ( 'NONE', #97323, 1000.000000000000000 ) ;
#105429 = LINE ( 'NONE', #66772, #104970 ) ;
#105430 = CARTESIAN_POINT ( 'NONE',  ( 12.89999999999989733, 2.500000000000000000, -0.1000000000000023925 ) ) ;
#105431 = EDGE_CURVE ( 'NONE', #78527, #102277, #55227, .T. ) ;
#105432 = ORIENTED_EDGE ( 'NONE', *, *, #4770, .T. ) ;
#105433 = CARTESIAN_POINT ( 'NONE',  ( -12.04999999999999538, 2.500000000000000000, 6.595190528383296780 ) ) ;
#105434 = DIRECTION ( 'NONE',  ( 0.000000000000000000, 1.000000000000000000, 0.000000000000000000 ) ) ;
#105435 = ADVANCED_FACE ( 'NONE', ( #97685 ), #26386, .T. ) ;
#105436 = CARTESIAN_POINT ( 'NONE',  ( 10.84999999999991260, 12.50000000000000000, 5.802370205355744659 ) ) ;
#105437 = DIRECTION ( 'NONE',  ( 0.000000000000000000, 0.000000000000000000, 1.000000000000000000 ) ) ;
#105438 = EDGE_LOOP ( 'NONE', ( #28115, #69741, #26909, #104892 ) ) ;
#105439 = AXIS2_PLACEMENT_3D ( 'NONE', #86448, #99997, #99355 ) ;
#105440 = CIRCLE ( 'NONE', #30245, 0.06509327318403745899 ) ;
#105441 = DIRECTION ( 'NONE',  ( 0.000000000000000000, 1.000000000000000000, 0.000000000000000000 ) ) ;
#105442 = EDGE_CURVE ( 'NONE', #30638, #32427, #68223, .T. ) ;
#105443 = FACE_OUTER_BOUND ( 'NONE', #26463, .T. ) ;
#105444 = ORIENTED_EDGE ( 'NONE', *, *, #96280, .F. ) ;
#105445 = CARTESIAN_POINT ( 'NONE',  ( 3.549999999999942979, 12.50000000000000000, 1.818653347947321475 ) ) ;
#105446 = EDGE_CURVE ( 'NONE', #126915, #44564, #65649, .T. ) ;
#105447 = ORIENTED_EDGE ( 'NONE', *, *, #13986, .F. ) ;
#105448 = FACE_BOUND ( 'NONE', #11438, .T. ) ;
#105449 = EDGE_CURVE ( 'NONE', #84838, #58093, #36462, .T. ) ;
#105450 = CARTESIAN_POINT ( 'NONE',  ( 7.099999999999928590, 12.50000000000000000, 4.330127018922196314 ) ) ;
#105451 = ORIENTED_EDGE ( 'NONE', *, *, #63914, .F. ) ;
#105452 = CARTESIAN_POINT ( 'NONE',  ( 6.249999999999968914, 2.500000000000000000, -6.595190528383302109 ) ) ;
#105453 = DIRECTION ( 'NONE',  ( 0.000000000000000000, 0.000000000000000000, -1.000000000000000000 ) ) ;
#105454 = VERTEX_POINT ( 'NONE', #16530 ) ;
#105455 = ORIENTED_EDGE ( 'NONE', *, *, #118446, .F. ) ;
#105456 = CARTESIAN_POINT ( 'NONE',  ( 185.0885416670080872, -6.551208109652273848, -3.782341765625003571 ) ) ;
#105457 = EDGE_LOOP ( 'NONE', ( #91714, #89185 ) ) ;
#105458 = CARTESIAN_POINT ( 'NONE',  ( 184.8385416670080872, 6.551208109652274736, 3.782341765625001351 ) ) ;
#105459 = DIRECTION ( 'NONE',  ( 0.000000000000000000, 1.000000000000000000, 0.000000000000000000 ) ) ;
#105460 = VECTOR ( 'NONE', #64852, 1000.000000000000000 ) ;
#105461 = CIRCLE ( 'NONE', #90881, 0.06509327318403745899 ) ;
#105462 = CARTESIAN_POINT ( 'NONE',  ( 3.149999999999946176, 2.500000000000000000, -1.918653347947325782 ) ) ;
#105463 = DIRECTION ( 'NONE',  ( 0.000000000000000000, -0.000000000000000000, 1.000000000000000000 ) ) ;
#105464 = DIRECTION ( 'NONE',  ( 0.000000000000000000, 0.000000000000000000, 1.000000000000000000 ) ) ;
#105465 = AXIS2_PLACEMENT_3D ( 'NONE', #29773, #69698, #109632 ) ;
#105466 = ORIENTED_EDGE ( 'NONE', *, *, #122880, .F. ) ;
#105467 = VERTEX_POINT ( 'NONE', #88503 ) ;
#105468 = DIRECTION ( 'NONE',  ( 0.000000000000000000, 0.000000000000000000, 1.000000000000000000 ) ) ;
#105469 = CARTESIAN_POINT ( 'NONE',  ( 10.19999999999991225, 2.500000000000000000, -4.776537180435978414 ) ) ;
#105470 = DIRECTION ( 'NONE',  ( 0.000000000000000000, 0.000000000000000000, 1.000000000000000000 ) ) ;
#105471 = DIRECTION ( 'NONE',  ( 0.000000000000000000, 0.000000000000000000, 1.000000000000000000 ) ) ;
#105473 = ORIENTED_EDGE ( 'NONE', *, *, #4436, .F. ) ;
#105472 = ORIENTED_EDGE ( 'NONE', *, *, #60029, .F. ) ;
#105474 = FACE_BOUND ( 'NONE', #105410, .T. ) ;
#105475 = ORIENTED_EDGE ( 'NONE', *, *, #124411, .T. ) ;
#105476 = DIRECTION ( 'NONE',  ( 0.000000000000000000, 0.000000000000000000, 1.000000000000000000 ) ) ;
#105477 = FACE_OUTER_BOUND ( 'NONE', #29233, .T. ) ;
#105478 = ORIENTED_EDGE ( 'NONE', *, *, #112943, .T. ) ;
#105479 = CARTESIAN_POINT ( 'NONE',  ( 12.04999999999990834, 12.50000000000000000, 6.495190528383297135 ) ) ;
#105480 = CARTESIAN_POINT ( 'NONE',  ( 154.1524742528378056, 0.5000000000000000000, -1.703575533167231537 ) ) ;
#105481 = ADVANCED_FACE ( 'NONE', ( #66295 ), #75467, .T. ) ;
#105482 = CARTESIAN_POINT ( 'NONE',  ( 8.549999999999920774, 12.50000000000000000, 6.083687093685483660 ) ) ;
#105484 = DIRECTION ( 'NONE',  ( 0.000000000000000000, -0.000000000000000000, 1.000000000000000000 ) ) ;
#105483 = VECTOR ( 'NONE', #94253, 1000.000000000000000 ) ;
#105485 = AXIS2_PLACEMENT_3D ( 'NONE', #16797, #86852, #56722 ) ;
#105487 = ADVANCED_FACE ( 'NONE', ( #126515 ), #105397, .T. ) ;
#105486 = CARTESIAN_POINT ( 'NONE',  ( 7.899999999999924860, 2.500000000000000000, -5.022947341949754119 ) ) ;
#105488 = CARTESIAN_POINT ( 'NONE',  ( -12.49999999999999467, 2.500000000000000000, 0.7928203230275536750 ) ) ;
#105489 = AXIS2_PLACEMENT_3D ( 'NONE', #97796, #87319, #49369 ) ;
#105490 = AXIS2_PLACEMENT_3D ( 'NONE', #77617, #59306, #27886 ) ;
#105491 = CARTESIAN_POINT ( 'NONE',  ( 11.64999999999990443, 2.500000000000000000, 2.957883832488649389 ) ) ;
#105492 = DIRECTION ( 'NONE',  ( -0.000000000000000000, -1.000000000000000000, -0.000000000000000000 ) ) ;
#105493 = DIRECTION ( 'NONE',  ( -0.000000000000000000, 1.000000000000000000, -0.000000000000000000 ) ) ;
#105494 = AXIS2_PLACEMENT_3D ( 'NONE', #94881, #45153, #35328 ) ;
#105495 = ORIENTED_EDGE ( 'NONE', *, *, #94206, .T. ) ;
#105497 = EDGE_LOOP ( 'NONE', ( #42576, #125849, #73666, #72532 ) ) ;
#105496 = CONICAL_SURFACE ( 'NONE', #111749, 0.1000000000000000472, 0.003490658503988666988 ) ;
#105499 = DIRECTION ( 'NONE',  ( 0.000000000000000000, 0.000000000000000000, 1.000000000000000000 ) ) ;
#105498 = AXIS2_PLACEMENT_3D ( 'NONE', #20684, #32462, #21986 ) ;
#105500 = ORIENTED_EDGE ( 'NONE', *, *, #57573, .T. ) ;
#105501 = DIRECTION ( 'NONE',  ( -4.274815082592931898E-19, -0.9999939076577903929, -0.003490651415223739937 ) ) ;
#105503 = VERTEX_POINT ( 'NONE', #82425 ) ;
#105502 = VERTEX_POINT ( 'NONE', #19784 ) ;
#105504 = ORIENTED_EDGE ( 'NONE', *, *, #4954, .T. ) ;
#105505 = CARTESIAN_POINT ( 'NONE',  ( -2.900000000000030109, 12.50000000000000000, -3.702399969078687292 ) ) ;
#105506 = AXIS2_PLACEMENT_3D ( 'NONE', #116940, #27280, #17450 ) ;
#105507 = VECTOR ( 'NONE', #92920, 1000.000000000000000 ) ;
#105508 = DIRECTION ( 'NONE',  ( 0.000000000000000000, 1.000000000000000000, 0.000000000000000000 ) ) ;
#105509 = DIRECTION ( 'NONE',  ( 0.000000000000000000, 0.000000000000000000, 1.000000000000000000 ) ) ;
#105510 = CARTESIAN_POINT ( 'NONE',  ( 7.899999999999924860, 12.50000000000000000, -4.330127018922201643 ) ) ;
#105511 = AXIS2_PLACEMENT_3D ( 'NONE', #73180, #23421, #84279 ) ;
#105512 = FACE_OUTER_BOUND ( 'NONE', #87278, .T. ) ;
#105513 = ORIENTED_EDGE ( 'NONE', *, *, #32619, .T. ) ;
#105514 = FACE_OUTER_BOUND ( 'NONE', #121726, .T. ) ;
#105515 = VERTEX_POINT ( 'NONE', #79355 ) ;
#105516 = ORIENTED_EDGE ( 'NONE', *, *, #646, .T. ) ;
#105517 = VERTEX_POINT ( 'NONE', #32037 ) ;
#105518 = ORIENTED_EDGE ( 'NONE', *, *, #109039, .F. ) ;
#105519 = CARTESIAN_POINT ( 'NONE',  ( 10.84999999999990905, 2.500000000000000000, -6.595190528383302109 ) ) ;
#105520 = ORIENTED_EDGE ( 'NONE', *, *, #118879, .F. ) ;
#105521 = ORIENTED_EDGE ( 'NONE', *, *, #87473, .F. ) ;
#105522 = AXIS2_PLACEMENT_3D ( 'NONE', #57401, #105201, #76400 ) ;
#105523 = CARTESIAN_POINT ( 'NONE',  ( 5.849999999999935696, 2.500000000000000000, -7.188010851410854052 ) ) ;
#105524 = EDGE_CURVE ( 'NONE', #25026, #129352, #48977, .T. ) ;
#105525 = CARTESIAN_POINT ( 'NONE',  ( -2.500000000000032863, 12.50000000000000000, 5.088040615133786027 ) ) ;
#105526 = DIRECTION ( 'NONE',  ( 0.000000000000000000, 0.000000000000000000, 1.000000000000000000 ) ) ;
#105527 = CARTESIAN_POINT ( 'NONE',  ( 8.549999999999920774, 2.500000000000000000, 6.048780366869521252 ) ) ;
#105528 = LINE ( 'NONE', #15842, #97256 ) ;
#105529 = CARTESIAN_POINT ( 'NONE',  ( -5.600000000000023626, 12.50000000000000000, -4.676537180435977881 ) ) ;
#105530 = ORIENTED_EDGE ( 'NONE', *, *, #59802, .F. ) ;
#105531 = DIRECTION ( 'NONE',  ( 0.000000000000000000, 0.000000000000000000, 1.000000000000000000 ) ) ;
#105532 = AXIS2_PLACEMENT_3D ( 'NONE', #36422, #84853, #55402 ) ;
#105533 = EDGE_CURVE ( 'NONE', #80302, #7899, #39449, .T. ) ;
#105534 = AXIS2_PLACEMENT_3D ( 'NONE', #20122, #60068, #22715 ) ;
#105535 = ORIENTED_EDGE ( 'NONE', *, *, #77254, .F. ) ;
#105536 = DIRECTION ( 'NONE',  ( 0.000000000000000000, 1.000000000000000000, 0.000000000000000000 ) ) ;
#105537 = ORIENTED_EDGE ( 'NONE', *, *, #65626, .T. ) ;
#105538 = CARTESIAN_POINT ( 'NONE',  ( -0.6500000000000389910, 2.500000000000000000, -6.148780366869526226 ) ) ;
#105539 = EDGE_LOOP ( 'NONE', ( #123558, #9198 ) ) ;
#105540 = EDGE_CURVE ( 'NONE', #60348, #87315, #42731, .T. ) ;
#105541 = EDGE_CURVE ( 'NONE', #107815, #3627, #19724, .T. ) ;
#105542 = ORIENTED_EDGE ( 'NONE', *, *, #103168, .T. ) ;
#105543 = UNCERTAINTY_MEASURE_WITH_UNIT (LENGTH_MEASURE( 1.000000000000000082E-05 ), #103418, 'distance_accuracy_value', 'NONE');
#105544 = DIRECTION ( 'NONE',  ( 0.000000000000000000, -0.000000000000000000, 1.000000000000000000 ) ) ;
#105545 = CARTESIAN_POINT ( 'NONE',  ( -2.500000000000032419, 12.50000000000000000, 0.6928203230275494784 ) ) ;
#105546 = AXIS2_PLACEMENT_3D ( 'NONE', #125221, #116037, #65645 ) ;
#105547 = FACE_OUTER_BOUND ( 'NONE', #84787, .T. ) ;
#105548 = DIRECTION ( 'NONE',  ( -0.000000000000000000, -1.000000000000000000, -0.000000000000000000 ) ) ;
#105549 = DIRECTION ( 'NONE',  ( -0.000000000000000000, 1.000000000000000000, -0.000000000000000000 ) ) ;
#105550 = ORIENTED_EDGE ( 'NONE', *, *, #54396, .T. ) ;
#105551 = DIRECTION ( 'NONE',  ( 0.000000000000000000, 0.000000000000000000, 1.000000000000000000 ) ) ;
#105552 = DIRECTION ( 'NONE',  ( 0.000000000000000000, -0.9999939076577903929, 0.003490651415223739937 ) ) ;
#105553 = EDGE_CURVE ( 'NONE', #70010, #22461, #103352, .T. ) ;
#105554 = LINE ( 'NONE', #127762, #60687 ) ;
#105555 = DIRECTION ( 'NONE',  ( 0.000000000000000000, -0.000000000000000000, 1.000000000000000000 ) ) ;
#105556 = DIRECTION ( 'NONE',  ( 0.000000000000000000, 0.000000000000000000, -1.000000000000000000 ) ) ;
#105557 = VERTEX_POINT ( 'NONE', #9957 ) ;
#105558 = AXIS2_PLACEMENT_3D ( 'NONE', #81761, #60847, #102065 ) ;
#105559 = CIRCLE ( 'NONE', #13596, 0.1000000000000002554 ) ;
#105560 = ORIENTED_EDGE ( 'NONE', *, *, #90543, .F. ) ;
#105561 = UNCERTAINTY_MEASURE_WITH_UNIT (LENGTH_MEASURE( 1.000000000000000082E-05 ), #92451, 'distance_accuracy_value', 'NONE');
#105562 = ORIENTED_EDGE ( 'NONE', *, *, #49179, .F. ) ;
#105563 = CARTESIAN_POINT ( 'NONE',  ( -4.350000000000023626, 2.500000000000000000, -1.718653347947325827 ) ) ;
#105564 = DIRECTION ( 'NONE',  ( 0.000000000000000000, 1.000000000000000000, 0.000000000000000000 ) ) ;
#105565 = CARTESIAN_POINT ( 'NONE',  ( 187.3333333333333144, 6.668395609140177704, -3.849999999999998312 ) ) ;
#105566 = LINE ( 'NONE', #123272, #34413 ) ;
#105567 = DIRECTION ( 'NONE',  ( 0.000000000000000000, 1.000000000000000000, 0.000000000000000000 ) ) ;
#105568 = FACE_OUTER_BOUND ( 'NONE', #35021, .T. ) ;
#105569 = AXIS2_PLACEMENT_3D ( 'NONE', #35331, #15003, #123677 ) ;
#105570 = CARTESIAN_POINT ( 'NONE',  ( 12.09999999999990550, 12.50000000000000000, -4.395220292106239768 ) ) ;
#105571 = VERTEX_POINT ( 'NONE', #49899 ) ;
#105572 = EDGE_CURVE ( 'NONE', #55495, #66544, #3211, .T. ) ;
#105574 = FACE_OUTER_BOUND ( 'NONE', #89116, .T. ) ;
#105573 = CIRCLE ( 'NONE', #88838, 0.1000000000000000472 ) ;
#105575 = DIRECTION ( 'NONE',  ( -0.000000000000000000, 1.000000000000000000, -0.000000000000000000 ) ) ;
#105576 = CONICAL_SURFACE ( 'NONE', #5297, 0.09999999999999982514, 0.003490658503988666988 ) ;
#105577 = ORIENTED_EDGE ( 'NONE', *, *, #92669, .F. ) ;
#105578 = AXIS2_PLACEMENT_3D ( 'NONE', #28225, #29512, #79891 ) ;
#105579 = EDGE_CURVE ( 'NONE', #110110, #20105, #103342, .T. ) ;
#105580 = DIRECTION ( 'NONE',  ( -4.274815082592931898E-19, -0.9999939076577903929, -0.003490651415223739937 ) ) ;
#105581 = DIRECTION ( 'NONE',  ( 0.000000000000000000, 0.000000000000000000, 1.000000000000000000 ) ) ;
#105582 = EDGE_CURVE ( 'NONE', #54150, #70834, #97075, .T. ) ;
#105583 = DIRECTION ( 'NONE',  ( 0.000000000000000000, -0.9999939076577903929, 0.003490651415223739937 ) ) ;
#105584 = AXIS2_PLACEMENT_3D ( 'NONE', #46935, #94719, #37745 ) ;
#105585 = AXIS2_PLACEMENT_3D ( 'NONE', #105323, #104035, #94857 ) ;
#105586 = EDGE_LOOP ( 'NONE', ( #91911, #99890 ) ) ;
#105587 = AXIS2_PLACEMENT_3D ( 'NONE', #72848, #70917, #11983 ) ;
#105588 = DIRECTION ( 'NONE',  ( -0.000000000000000000, -1.000000000000000000, -0.000000000000000000 ) ) ;
#105589 = ADVANCED_FACE ( 'NONE', ( #33324 ), #12667, .T. ) ;
#105590 = CONICAL_SURFACE ( 'NONE', #49174, 0.09999999999999982514, 0.003490658503988666988 ) ;
#105591 = EDGE_CURVE ( 'NONE', #56070, #4982, #41950, .T. ) ;
#105592 = ORIENTED_EDGE ( 'NONE', *, *, #118436, .T. ) ;
#105593 = CARTESIAN_POINT ( 'NONE',  ( 1.849999999999949019, 2.500000000000000000, 6.941600689897073018 ) ) ;
#105594 = FACE_OUTER_BOUND ( 'NONE', #29106, .T. ) ;
#105595 = EDGE_CURVE ( 'NONE', #33970, #28402, #94161, .T. ) ;
#105596 = EDGE_CURVE ( 'NONE', #90021, #124886, #110871, .T. ) ;
#105597 = ORIENTED_EDGE ( 'NONE', *, *, #42349, .T. ) ;
#105598 = CONICAL_SURFACE ( 'NONE', #78515, 0.1000000000000002554, 0.003490658503988666988 ) ;
#105599 = VECTOR ( 'NONE', #12087, 1000.000000000000000 ) ;
#105600 = DIRECTION ( 'NONE',  ( -0.000000000000000000, -1.000000000000000000, -0.000000000000000000 ) ) ;
#105601 = EDGE_CURVE ( 'NONE', #36661, #55739, #35682, .T. ) ;
#105602 = PLANE ( 'NONE',  #108122 ) ;
#105603 = VECTOR ( 'NONE', #22013, 1000.000000000000000 ) ;
#105604 = VERTEX_POINT ( 'NONE', #62776 ) ;
#105605 = EDGE_CURVE ( 'NONE', #79633, #94125, #71952, .T. ) ;
#105606 = FACE_OUTER_BOUND ( 'NONE', #115738, .T. ) ;
#105607 = EDGE_LOOP ( 'NONE', ( #48196, #114214, #75703, #112749 ) ) ;
#105608 = VERTEX_POINT ( 'NONE', #92209 ) ;
#105609 = CARTESIAN_POINT ( 'NONE',  ( 3.349999999999942801, 2.500000000000000000, 2.957883832488649389 ) ) ;
#105610 = CARTESIAN_POINT ( 'NONE',  ( -6.850000000000013856, 2.500000000000000000, 1.918653347947321564 ) ) ;
#105611 = EDGE_LOOP ( 'NONE', ( #22177, #24826, #116408, #93898 ) ) ;
#105612 = CARTESIAN_POINT ( 'NONE',  ( 2.699999999999946443, 12.50000000000000000, 0.4115034346978109769 ) ) ;
#105613 = PLANE ( 'NONE',  #98620 ) ;
#105614 = CIRCLE ( 'NONE', #90942, 0.06509327318403745899 ) ;
#105615 = ORIENTED_EDGE ( 'NONE', *, *, #30894, .T. ) ;
#105616 = LINE ( 'NONE', #94481, #9169 ) ;
#105617 = DIRECTION ( 'NONE',  ( 0.000000000000000000, 0.000000000000000000, 1.000000000000000000 ) ) ;
#105618 = CARTESIAN_POINT ( 'NONE',  ( 17.02136413300351947, -1.939324994459653118, -5.540650668389590194 ) ) ;
#105619 = DIRECTION ( 'NONE',  ( -4.274815082592931898E-19, -0.9999939076577903929, -0.003490651415223739937 ) ) ;
#105620 = CARTESIAN_POINT ( 'NONE',  ( 14.39999999999989555, 12.50000000000000000, 0.3464101615137736845 ) ) ;
#105621 = CIRCLE ( 'NONE', #22015, 0.1000000000000002554 ) ;
#105622 = CARTESIAN_POINT ( 'NONE',  ( -13.34999999999999076, 2.500000000000000000, 1.472243186433549456 ) ) ;
#105623 = AXIS2_PLACEMENT_3D ( 'NONE', #92596, #72326, #91952 ) ;
#105624 = AXIS2_PLACEMENT_3D ( 'NONE', #16072, #124763, #126038 ) ;
#105625 = VERTEX_POINT ( 'NONE', #2533 ) ;
#105626 = ORIENTED_EDGE ( 'NONE', *, *, #123720, .T. ) ;
#105627 = VERTEX_POINT ( 'NONE', #42496 ) ;
#105628 = EDGE_LOOP ( 'NONE', ( #36449, #86379 ) ) ;
#105629 = LINE ( 'NONE', #103035, #28603 ) ;
#105630 = DIRECTION ( 'NONE',  ( 0.000000000000000000, 1.000000000000000000, 0.000000000000000000 ) ) ;
#105631 = DIRECTION ( 'NONE',  ( -0.000000000000000000, 1.000000000000000000, -0.000000000000000000 ) ) ;
#105632 = ORIENTED_EDGE ( 'NONE', *, *, #46976, .F. ) ;
#105633 = FACE_BOUND ( 'NONE', #42219, .T. ) ;
#105634 = FACE_OUTER_BOUND ( 'NONE', #20653, .T. ) ;
#105635 = CARTESIAN_POINT ( 'NONE',  ( -12.04999999999999716, 12.50000000000000000, -2.165063509461097713 ) ) ;
#105636 = CIRCLE ( 'NONE', #7322, 0.09999999999999982514 ) ;
#105637 = DIRECTION ( 'NONE',  ( 0.000000000000000000, 1.000000000000000000, 0.000000000000000000 ) ) ;
#105638 = EDGE_CURVE ( 'NONE', #10224, #97917, #54446, .T. ) ;
#105639 = LINE ( 'NONE', #6127, #63797 ) ;
#105640 = AXIS2_PLACEMENT_3D ( 'NONE', #41739, #111746, #122219 ) ;
#105641 = LINE ( 'NONE', #15941, #63893 ) ;
#105642 = CARTESIAN_POINT ( 'NONE',  ( 2.099999999999948574, 2.500000000000000000, 4.430127018922196847 ) ) ;
#105643 = CARTESIAN_POINT ( 'NONE',  ( -4.150000000000025224, 2.500000000000000000, 2.757883832488649656 ) ) ;
#105644 = DIRECTION ( 'NONE',  ( 0.000000000000000000, 1.000000000000000000, 0.000000000000000000 ) ) ;
#105645 = DIRECTION ( 'NONE',  ( 0.000000000000000000, 0.000000000000000000, -1.000000000000000000 ) ) ;
#105646 = FACE_OUTER_BOUND ( 'NONE', #38480, .T. ) ;
#105647 = ADVANCED_FACE ( 'NONE', ( #52952 ), #56496, .T. ) ;
#105648 = VECTOR ( 'NONE', #57961, 1000.000000000000000 ) ;
#105649 = VERTEX_POINT ( 'NONE', #19102 ) ;
#105650 = ORIENTED_EDGE ( 'NONE', *, *, #49030, .F. ) ;
#105651 = ORIENTED_EDGE ( 'NONE', *, *, #114143, .F. ) ;
#105652 = EDGE_LOOP ( 'NONE', ( #20774, #70876, #110662, #104728 ) ) ;
#105653 = CARTESIAN_POINT ( 'NONE',  ( 2.899999999999945732, 12.50000000000000000, -2.385244779468109755E-15 ) ) ;
#105654 = EDGE_LOOP ( 'NONE', ( #17586, #49807 ) ) ;
#105655 = PLANE ( 'NONE',  #109132 ) ;
#105656 = VERTEX_POINT ( 'NONE', #59061 ) ;
#105657 = EDGE_LOOP ( 'NONE', ( #61189, #99098, #50241, #14672 ) ) ;
#105658 = CARTESIAN_POINT ( 'NONE',  ( -1.900000000000034994, 12.50000000000000000, -0.3464101615137783474 ) ) ;
#105659 = AXIS2_PLACEMENT_3D ( 'NONE', #91480, #81659, #100023 ) ;
#105661 = CARTESIAN_POINT ( 'NONE',  ( -13.54999999999999005, 2.500000000000000000, -1.818653347947323917 ) ) ;
#105660 = PRODUCT_DEFINITION_CONTEXT ( 'detailed design', #114080, 'design' ) ;
#105662 = PLANE ( 'NONE',  #20682 ) ;
#105663 = CARTESIAN_POINT ( 'NONE',  ( 184.0312500006828031, 9.429780353434619030E-16, -7.700000000000000178 ) ) ;
#105664 = FACE_OUTER_BOUND ( 'NONE', #94115, .T. ) ;
#105665 = AXIS2_PLACEMENT_3D ( 'NONE', #16927, #87628, #98736 ) ;
#105666 = EDGE_LOOP ( 'NONE', ( #83243, #9488, #17376, #34291 ) ) ;
#105667 = ORIENTED_EDGE ( 'NONE', *, *, #101864, .F. ) ;
#105669 = VERTEX_POINT ( 'NONE', #64053 ) ;
#105668 = CONICAL_SURFACE ( 'NONE', #101460, 0.09999999999999999167, 0.003490658503988666988 ) ;
#105670 = ORIENTED_EDGE ( 'NONE', *, *, #54792, .T. ) ;
#105671 = VECTOR ( 'NONE', #114082, 1000.000000000000000 ) ;
#105672 = CARTESIAN_POINT ( 'NONE',  ( -9.600000000000006750, 12.50000000000000000, -0.6928203230275542523 ) ) ;
#105673 = EDGE_LOOP ( 'NONE', ( #419, #103722 ) ) ;
#105674 = VERTEX_POINT ( 'NONE', #24779 ) ;
#105675 = FACE_OUTER_BOUND ( 'NONE', #48329, .T. ) ;
#105676 = CIRCLE ( 'NONE', #65953, 0.1000000000000000056 ) ;
#105677 = ADVANCED_FACE ( 'NONE', ( #65980 ), #64906, .T. ) ;
#105678 = CARTESIAN_POINT ( 'NONE',  ( -4.800000000000028244, 12.50000000000000000, -3.983716857408426293 ) ) ;
#105679 = DIRECTION ( 'NONE',  ( 0.000000000000000000, 1.000000000000000000, 0.000000000000000000 ) ) ;
#105680 = CARTESIAN_POINT ( 'NONE',  ( 7.699999999999925571, 12.50000000000000000, 4.048810130592458201 ) ) ;
#105681 = AXIS2_PLACEMENT_3D ( 'NONE', #37643, #25873, #5567 ) ;
#105682 = DIRECTION ( 'NONE',  ( 0.000000000000000000, 0.000000000000000000, -1.000000000000000000 ) ) ;
#105683 = DIRECTION ( 'NONE',  ( 0.000000000000000000, 1.224646799147353454E-16, 1.000000000000000000 ) ) ;
#105684 = EDGE_LOOP ( 'NONE', ( #34085, #28968 ) ) ;
#105685 = CARTESIAN_POINT ( 'NONE',  ( -2.300000000000033129, 12.50000000000000000, 3.918623584224382839 ) ) ;
#105686 = CIRCLE ( 'NONE', #3277, 0.06509327318403745899 ) ;
#105688 = EDGE_CURVE ( 'NONE', #87698, #45516, #66, .T. ) ;
#105687 = VECTOR ( 'NONE', #98370, 1000.000000000000000 ) ;
#105689 = ORIENTED_EDGE ( 'NONE', *, *, #27423, .T. ) ;
#105690 = DIRECTION ( 'NONE',  ( -0.000000000000000000, -1.000000000000000000, -0.000000000000000000 ) ) ;
#105691 = VECTOR ( 'NONE', #32281, 1000.000000000000000 ) ;
#105692 = EDGE_LOOP ( 'NONE', ( #106008, #72070 ) ) ;
#105693 = CARTESIAN_POINT ( 'NONE',  ( -2.950000000000029932, 2.500000000000000000, -2.165063509461101710 ) ) ;
#105694 = FACE_OUTER_BOUND ( 'NONE', #19451, .T. ) ;
#105695 = AXIS2_PLACEMENT_3D ( 'NONE', #110058, #111313, #21679 ) ;
#105696 = EDGE_LOOP ( 'NONE', ( #128634, #74854 ) ) ;
#105698 = ADVANCED_FACE ( 'NONE', ( #103983 ), #125548, .T. ) ;
#105697 = DIRECTION ( 'NONE',  ( -0.000000000000000000, -1.000000000000000000, -0.000000000000000000 ) ) ;
#105699 = DIRECTION ( 'NONE',  ( 0.000000000000000000, 1.000000000000000000, 0.000000000000000000 ) ) ;
#105700 = EDGE_CURVE ( 'NONE', #118817, #34687, #121343, .T. ) ;
#105701 = ORIENTED_EDGE ( 'NONE', *, *, #32031, .T. ) ;
#105702 = CARTESIAN_POINT ( 'NONE',  ( -14.39999999999998614, 2.500000000000000000, -0.2464101615137760659 ) ) ;
#105703 = EDGE_CURVE ( 'NONE', #85431, #121481, #6381, .T. ) ;
#105704 = CARTESIAN_POINT ( 'NONE',  ( 10.59999999999991260, 12.50000000000000000, -0.3464101615137783474 ) ) ;
#105705 = ORIENTED_EDGE ( 'NONE', *, *, #3200, .F. ) ;
#105706 = ORIENTED_EDGE ( 'NONE', *, *, #93014, .F. ) ;
#105707 = CARTESIAN_POINT ( 'NONE',  ( -11.64999999999999680, 12.50000000000000000, -7.122917578226813262 ) ) ;
#105708 = CARTESIAN_POINT ( 'NONE',  ( 11.89999999999990798, 2.500000000000000000, -4.083716857408426826 ) ) ;
#105709 = EDGE_CURVE ( 'NONE', #81765, #35406, #102483, .T. ) ;
#105710 = CARTESIAN_POINT ( 'NONE',  ( 187.2135416670080588, 4.367472073101518859, -7.564683531249999149 ) ) ;
#105711 = AXIS2_PLACEMENT_3D ( 'NONE', #106741, #38013, #75999 ) ;
#105712 = CARTESIAN_POINT ( 'NONE',  ( -8.150000000000012790, 2.500000000000000000, 2.511473670974873507 ) ) ;
#105713 = CARTESIAN_POINT ( 'NONE',  ( 0.4499999999999573785, 2.500000000000000000, -6.495190528383302464 ) ) ;
#105714 = FACE_OUTER_BOUND ( 'NONE', #106412, .T. ) ;
#105715 = CIRCLE ( 'NONE', #107851, 0.1000000000000000056 ) ;
#105716 = AXIS2_PLACEMENT_3D ( 'NONE', #44108, #64393, #73556 ) ;
#105717 = ORIENTED_EDGE ( 'NONE', *, *, #104692, .T. ) ;
#105718 = CIRCLE ( 'NONE', #40985, 0.1000000000000002554 ) ;
#105719 = CARTESIAN_POINT ( 'NONE',  ( 15.79999999999989058, 2.500000000000000000, -0.1000000000000023925 ) ) ;
#105720 = VERTEX_POINT ( 'NONE', #14291 ) ;
#105721 = DIRECTION ( 'NONE',  ( -0.000000000000000000, 1.000000000000000000, -0.000000000000000000 ) ) ;
#105722 = DIRECTION ( 'NONE',  ( 0.000000000000000000, 0.000000000000000000, 1.000000000000000000 ) ) ;
#105723 = DIRECTION ( 'NONE',  ( -0.000000000000000000, 1.000000000000000000, -0.000000000000000000 ) ) ;
#105724 = VERTEX_POINT ( 'NONE', #114429 ) ;
#105725 = AXIS2_PLACEMENT_3D ( 'NONE', #89654, #98813, #99483 ) ;
#105727 = CIRCLE ( 'NONE', #55643, 0.1000000000000000472 ) ;
#105726 = VECTOR ( 'NONE', #60896, 1000.000000000000000 ) ;
#105728 = LINE ( 'NONE', #116173, #26360 ) ;
#105729 = PLANE ( 'NONE',  #1597 ) ;
#105730 = ORIENTED_EDGE ( 'NONE', *, *, #93143, .T. ) ;
#105731 = DIRECTION ( 'NONE',  ( -0.000000000000000000, -1.000000000000000000, -0.000000000000000000 ) ) ;
#105732 = CONICAL_SURFACE ( 'NONE', #93135, 0.1000000000000002554, 0.003490658503988666988 ) ;
#105733 = EDGE_LOOP ( 'NONE', ( #98064, #23502, #8592, #51346 ) ) ;
#105734 = ORIENTED_EDGE ( 'NONE', *, *, #48875, .T. ) ;
#105735 = DIRECTION ( 'NONE',  ( 0.000000000000000000, 0.000000000000000000, -1.000000000000000000 ) ) ;
#105736 = EDGE_CURVE ( 'NONE', #28294, #27245, #85619, .T. ) ;
#105737 = ADVANCED_FACE ( 'NONE', ( #93515 ), #86249, .T. ) ;
#105738 = VERTEX_POINT ( 'NONE', #4449 ) ;
#105739 = DIRECTION ( 'NONE',  ( 0.000000000000000000, -0.000000000000000000, 1.000000000000000000 ) ) ;
#105741 = ADVANCED_FACE ( 'NONE', ( #105261 ), #37736, .T. ) ;
#105740 = PLANE ( 'NONE',  #8735 ) ;
#105742 = EDGE_CURVE ( 'NONE', #98508, #34124, #104610, .T. ) ;
#105743 = CARTESIAN_POINT ( 'NONE',  ( 12.09999999999990195, 2.500000000000000000, 0.6928203230275494784 ) ) ;
#105744 = VERTEX_POINT ( 'NONE', #115718 ) ;
#105745 = FACE_BOUND ( 'NONE', #24436, .T. ) ;
#105746 = EDGE_CURVE ( 'NONE', #110810, #33973, #8465, .T. ) ;
#105748 = ORIENTED_EDGE ( 'NONE', *, *, #75664, .F. ) ;
#105747 = DIRECTION ( 'NONE',  ( 0.000000000000000000, 0.000000000000000000, -1.000000000000000000 ) ) ;
#105749 = DIRECTION ( 'NONE',  ( 0.000000000000000000, 1.000000000000000000, 0.000000000000000000 ) ) ;
#105750 = LINE ( 'NONE', #16053, #126178 ) ;
#105751 = ORIENTED_EDGE ( 'NONE', *, *, #118973, .T. ) ;
#105752 = EDGE_CURVE ( 'NONE', #23200, #32927, #46056, .T. ) ;
#105753 = ADVANCED_FACE ( 'NONE', ( #115062 ), #89950, .T. ) ;
#105754 = CIRCLE ( 'NONE', #49347, 0.1000000000000000056 ) ;
#105755 = ORIENTED_EDGE ( 'NONE', *, *, #77619, .T. ) ;
#105756 = AXIS2_PLACEMENT_3D ( 'NONE', #118576, #108117, #17124 ) ;
#105757 = ORIENTED_EDGE ( 'NONE', *, *, #18375, .F. ) ;
#105758 = DIRECTION ( 'NONE',  ( 0.000000000000000000, -0.9999939076577903929, 0.003490651415223739937 ) ) ;
#105759 = CARTESIAN_POINT ( 'NONE',  ( 6.714630671518470706, 1.500000000000127010, 9.763603585529398998 ) ) ;
#105760 = DIRECTION ( 'NONE',  ( 0.000000000000000000, 0.000000000000000000, 1.000000000000000000 ) ) ;
#105761 = FACE_BOUND ( 'NONE', #27513, .T. ) ;
#105762 = ORIENTED_EDGE ( 'NONE', *, *, #93664, .F. ) ;
#105763 = CARTESIAN_POINT ( 'NONE',  ( 184.8593750003413732, 0.000000000000000000, 7.564683531250000925 ) ) ;
#105764 = EDGE_CURVE ( 'NONE', #31868, #32290, #4255, .T. ) ;
#105765 = CARTESIAN_POINT ( 'NONE',  ( 10.64999999999991331, 12.50000000000000000, 6.841600689897072485 ) ) ;
#105766 = CARTESIAN_POINT ( 'NONE',  ( -6.900000000000019007, 2.500000000000000000, -3.983716857408426293 ) ) ;
#105767 = CARTESIAN_POINT ( 'NONE',  ( -4.600000000000024514, 2.500000000000000000, -0.6928203230275542523 ) ) ;
#105768 = DIRECTION ( 'NONE',  ( 0.000000000000000000, 0.000000000000000000, -1.000000000000000000 ) ) ;
#105769 = DIRECTION ( 'NONE',  ( 0.000000000000000000, 1.846105847067148761E-16, 1.000000000000000000 ) ) ;
#105770 = CARTESIAN_POINT ( 'NONE',  ( 11.04999999999991012, 12.50000000000000000, 6.906693963081109722 ) ) ;
#105771 = DIRECTION ( 'NONE',  ( -0.000000000000000000, 1.000000000000000000, -0.000000000000000000 ) ) ;
#105772 = CONICAL_SURFACE ( 'NONE', #49262, 0.09999999999999999167, 0.003490658503988666988 ) ;
#105773 = CARTESIAN_POINT ( 'NONE',  ( -2.950000000000029932, 2.500000000000000000, 2.165063509461097713 ) ) ;
#105774 = AXIS2_PLACEMENT_3D ( 'NONE', #110651, #21636, #79906 ) ;
#105775 = ORIENTED_EDGE ( 'NONE', *, *, #40138, .T. ) ;
#105776 = VERTEX_POINT ( 'NONE', #94801 ) ;
#105777 = EDGE_LOOP ( 'NONE', ( #46205, #81834 ) ) ;
#105778 = VERTEX_POINT ( 'NONE', #76452 ) ;
#105779 = CIRCLE ( 'NONE', #128787, 0.1000000000000002554 ) ;
#105780 = ORIENTED_EDGE ( 'NONE', *, *, #79570, .T. ) ;
#105781 = CARTESIAN_POINT ( 'NONE',  ( 115.5000000000000000, -2.000000000000000000, -4.999999999999997335 ) ) ;
#105782 = DIRECTION ( 'NONE',  ( -4.274815082592931898E-19, -0.9999939076577903929, -0.003490651415223739937 ) ) ;
#105783 = EDGE_LOOP ( 'NONE', ( #15519, #102228 ) ) ;
#105784 = FACE_BOUND ( 'NONE', #50304, .T. ) ;
#105785 = CARTESIAN_POINT ( 'NONE',  ( -5.200000000000020606, 12.50000000000000000, -0.3464101615137782364 ) ) ;
#105786 = DIRECTION ( 'NONE',  ( -0.000000000000000000, -1.000000000000000000, -0.000000000000000000 ) ) ;
#105787 = CARTESIAN_POINT ( 'NONE',  ( 2.099999999999948574, 12.50000000000000000, 3.637306695894644726 ) ) ;
#105788 = CARTESIAN_POINT ( 'NONE',  ( 13.29999999999990301, 2.500000000000000000, 4.330127018922196314 ) ) ;
#105789 = CARTESIAN_POINT ( 'NONE',  ( 1.899999999999951283, 12.50000000000000000, -4.048810130592463530 ) ) ;
#105791 = ORIENTED_EDGE ( 'NONE', *, *, #104336, .T. ) ;
#105790 = CONICAL_SURFACE ( 'NONE', #20028, 0.1000000000000002554, 0.003490658503988666988 ) ;
#105792 = DIRECTION ( 'NONE',  ( 0.000000000000000000, 0.000000000000000000, -1.000000000000000000 ) ) ;
#105793 = VERTEX_POINT ( 'NONE', #116362 ) ;
#105794 = EDGE_CURVE ( 'NONE', #9476, #3359, #117125, .T. ) ;
#105795 = PRODUCT_DEFINITION_SHAPE ( 'NONE', 'NONE',  #129623 ) ;
#105796 = ORIENTED_EDGE ( 'NONE', *, *, #92849, .F. ) ;
#105797 = ORIENTED_EDGE ( 'NONE', *, *, #112779, .T. ) ;
#105798 = CARTESIAN_POINT ( 'NONE',  ( 3.149999999999944400, 12.50000000000000000, 1.818653347947321475 ) ) ;
#105799 = DIRECTION ( 'NONE',  ( 0.000000000000000000, 0.000000000000000000, 1.000000000000000000 ) ) ;
#105800 = VECTOR ( 'NONE', #24182, 1000.000000000000000 ) ;
#105801 = CARTESIAN_POINT ( 'NONE',  ( 4.549999999999939426, 2.500000000000000000, -6.495190528383302464 ) ) ;
#105802 = EDGE_LOOP ( 'NONE', ( #21973, #13891, #41814, #82571 ) ) ;
#105803 = CARTESIAN_POINT ( 'NONE',  ( 15.50772381900151942, 2.499999999999936939, -6.996973298636524952 ) ) ;
#105804 = CIRCLE ( 'NONE', #114115, 0.06509327318403745899 ) ;
#105805 = CONICAL_SURFACE ( 'NONE', #89167, 0.1000000000000002554, 0.003490658503988666988 ) ;
#105806 = DIRECTION ( 'NONE',  ( 0.000000000000000000, 0.000000000000000000, 1.000000000000000000 ) ) ;
#105807 = AXIS2_PLACEMENT_3D ( 'NONE', #97549, #18345, #117166 ) ;
#105808 = DIRECTION ( 'NONE',  ( -0.000000000000000000, -1.000000000000000000, -0.000000000000000000 ) ) ;
#105809 = CARTESIAN_POINT ( 'NONE',  ( 186.6927083336747160, 6.551208109652275624, -3.782341765624998686 ) ) ;
#105810 = CARTESIAN_POINT ( 'NONE',  ( -9.600000000000008527, 2.500000000000000000, -4.430127018922197735 ) ) ;
#105811 = CARTESIAN_POINT ( 'NONE',  ( -1.650000000000034772, 12.50000000000000000, 1.537336459617582918 ) ) ;
#105812 = ORIENTED_EDGE ( 'NONE', *, *, #34660, .T. ) ;
#105813 = DIRECTION ( 'NONE',  ( -0.000000000000000000, -1.000000000000000000, -0.000000000000000000 ) ) ;
#105814 = CIRCLE ( 'NONE', #11718, 0.09999999999999999167 ) ;
#105815 = ORIENTED_EDGE ( 'NONE', *, *, #64874, .F. ) ;
#105817 = CIRCLE ( 'NONE', #66096, 0.09999999999999982514 ) ;
#105816 = AXIS2_PLACEMENT_3D ( 'NONE', #21464, #41775, #101325 ) ;
#105818 = ORIENTED_EDGE ( 'NONE', *, *, #14386, .F. ) ;
#105819 = DIRECTION ( 'NONE',  ( -0.000000000000000000, 1.000000000000000000, -0.000000000000000000 ) ) ;
#105820 = DIRECTION ( 'NONE',  ( 0.000000000000000000, 1.000000000000000000, 0.000000000000000000 ) ) ;
#105821 = DIRECTION ( 'NONE',  ( 0.000000000000000000, -0.000000000000000000, 1.000000000000000000 ) ) ;
#105822 = EDGE_LOOP ( 'NONE', ( #23281, #36451, #20662, #26930 ) ) ;
#105823 = ORIENTED_EDGE ( 'NONE', *, *, #122642, .F. ) ;
#105824 = CARTESIAN_POINT ( 'NONE',  ( 7.899999999999924860, 12.50000000000000000, -3.702399969078687292 ) ) ;
#105825 = DIRECTION ( 'NONE',  ( -0.000000000000000000, 1.000000000000000000, -0.000000000000000000 ) ) ;
#105826 = CARTESIAN_POINT ( 'NONE',  ( -11.25000000000000000, 2.500000000000000000, 2.857883832488649301 ) ) ;
#105827 = VERTEX_POINT ( 'NONE', #65323 ) ;
#105828 = ORIENTED_EDGE ( 'NONE', *, *, #120648, .F. ) ;
#105829 = CARTESIAN_POINT ( 'NONE',  ( -7.700000000000014388, 12.50000000000000000, -4.676537180435977881 ) ) ;
#105830 = ORIENTED_EDGE ( 'NONE', *, *, #120957, .F. ) ;
#105831 = DIRECTION ( 'NONE',  ( -0.000000000000000000, -1.000000000000000000, -0.000000000000000000 ) ) ;
#105832 = EDGE_CURVE ( 'NONE', #57299, #44421, #15578, .T. ) ;
#105833 = LINE ( 'NONE', #16139, #42914 ) ;
#105834 = ORIENTED_EDGE ( 'NONE', *, *, #120009, .T. ) ;
#105835 = DIRECTION ( 'NONE',  ( 0.000000000000000000, 1.000000000000000000, 0.000000000000000000 ) ) ;
#105836 = CARTESIAN_POINT ( 'NONE',  ( -6.450000000000014388, 12.50000000000000000, 1.818653347947321475 ) ) ;
#105837 = DIRECTION ( 'NONE',  ( -0.000000000000000000, -1.000000000000000000, -0.000000000000000000 ) ) ;
#105838 = ADVANCED_FACE ( 'NONE', ( #48281 ), #85744, .T. ) ;
#105839 = CARTESIAN_POINT ( 'NONE',  ( -0.6000000000000323963, 2.500000000000000000, -0.3464101615137759604 ) ) ;
#105840 = EDGE_CURVE ( 'NONE', #105656, #63009, #119208, .T. ) ;
#105841 = VERTEX_POINT ( 'NONE', #39772 ) ;
#105842 = CARTESIAN_POINT ( 'NONE',  ( -14.14999999999998614, 2.500000000000000000, -2.165063509461099489 ) ) ;
#105843 = AXIS2_PLACEMENT_3D ( 'NONE', #111421, #40793, #122560 ) ;
#105844 = AXIS2_PLACEMENT_3D ( 'NONE', #120375, #71258, #39894 ) ;
#105845 = DIRECTION ( 'NONE',  ( 0.000000000000000000, 0.000000000000000000, 1.000000000000000000 ) ) ;
#105846 = EDGE_CURVE ( 'NONE', #51555, #54758, #104619, .T. ) ;
#105847 = ORIENTED_EDGE ( 'NONE', *, *, #38316, .T. ) ;
#105848 = EDGE_CURVE ( 'NONE', #128976, #54553, #6307, .T. ) ;
#105849 = ORIENTED_EDGE ( 'NONE', *, *, #109057, .T. ) ;
#105850 = ADVANCED_FACE ( 'NONE', ( #27993 ), #96202, .T. ) ;
#105851 = CARTESIAN_POINT ( 'NONE',  ( 185.0052083336747444, -6.551208109652278289, 3.782341765624995134 ) ) ;
#105853 = ADVANCED_FACE ( 'NONE', ( #29936 ), #27326, .T. ) ;
#105852 = CARTESIAN_POINT ( 'NONE',  ( 5.399999999999935518, 2.500000000000000000, -4.330127018922201643 ) ) ;
#105854 = DIRECTION ( 'NONE',  ( 0.000000000000000000, 0.000000000000000000, -1.000000000000000000 ) ) ;
#105855 = ADVANCED_FACE ( 'NONE', ( #97374 ), #117633, .T. ) ;
#105856 = CARTESIAN_POINT ( 'NONE',  ( 108.0000000000000142, 8.500000000000000000, 0.000000000000000000 ) ) ;
#105857 = FACE_OUTER_BOUND ( 'NONE', #51632, .T. ) ;
#105859 = CONICAL_SURFACE ( 'NONE', #99606, 0.1000000000000000472, 0.003490658503988666988 ) ;
#105858 = DIRECTION ( 'NONE',  ( -0.000000000000000000, 1.000000000000000000, -0.000000000000000000 ) ) ;
#105860 = CARTESIAN_POINT ( 'NONE',  ( 5.599999999999933031, 12.50000000000000000, -0.3464101615137783474 ) ) ;
#105861 = CARTESIAN_POINT ( 'NONE',  ( 13.94999999999989271, 12.50000000000000000, -1.818653347947326138 ) ) ;
#105862 = CARTESIAN_POINT ( 'NONE',  ( 11.04999999999991189, 12.50000000000000000, -2.511473670974877948 ) ) ;
#105863 = EDGE_CURVE ( 'NONE', #25898, #57277, #16771, .T. ) ;
#105864 = CARTESIAN_POINT ( 'NONE',  ( -6.450000000000017941, 2.500000000000000000, -6.941600689897077459 ) ) ;
#105866 = AXIS2_PLACEMENT_3D ( 'NONE', #119922, #32849, #23014 ) ;
#105865 = AXIS2_PLACEMENT_3D ( 'NONE', #2833, #44699, #95084 ) ;
#105867 = ORIENTED_EDGE ( 'NONE', *, *, #45030, .T. ) ;
#105868 = AXIS2_PLACEMENT_3D ( 'NONE', #107920, #115132, #47086 ) ;
#105869 = ORIENTED_EDGE ( 'NONE', *, *, #3279, .T. ) ;
#105870 = DIRECTION ( 'NONE',  ( 0.000000000000000000, 0.000000000000000000, -1.000000000000000000 ) ) ;
#105871 = ORIENTED_EDGE ( 'NONE', *, *, #113412, .F. ) ;
#105872 = CARTESIAN_POINT ( 'NONE',  ( -13.34999999999999076, 12.50000000000000000, -1.472243186433547901 ) ) ;
#105873 = DIRECTION ( 'NONE',  ( 0.000000000000000000, 0.000000000000000000, 1.000000000000000000 ) ) ;
#105874 = LINE ( 'NONE', #113271, #35356 ) ;
#105875 = ORIENTED_EDGE ( 'NONE', *, *, #73031, .T. ) ;
#105876 = CARTESIAN_POINT ( 'NONE',  ( 8.749999999999921840, 2.500000000000000000, -5.802370205355749988 ) ) ;
#105877 = LINE ( 'NONE', #77688, #17741 ) ;
#105879 = ORIENTED_EDGE ( 'NONE', *, *, #99843, .T. ) ;
#105878 = CARTESIAN_POINT ( 'NONE',  ( -13.94999999999998863, 2.500000000000000000, 2.411473670974877415 ) ) ;
#105880 = CIRCLE ( 'NONE', #41066, 0.06509327318403745899 ) ;
#105881 = DIRECTION ( 'NONE',  ( 0.000000000000000000, -0.9999939076577903929, 0.003490651415223739937 ) ) ;
#105882 = VERTEX_POINT ( 'NONE', #99319 ) ;
#105883 = AXIS2_PLACEMENT_3D ( 'NONE', #82082, #40901, #32376 ) ;
#105884 = EDGE_LOOP ( 'NONE', ( #31287, #39733 ) ) ;
#105885 = ORIENTED_EDGE ( 'NONE', *, *, #117922, .F. ) ;
#105886 = ORIENTED_EDGE ( 'NONE', *, *, #13351, .F. ) ;
#105887 = CARTESIAN_POINT ( 'NONE',  ( 12.89999999999989910, 12.50000000000000000, -0.7579135962115917113 ) ) ;
#105888 = VECTOR ( 'NONE', #70541, 1000.000000000000000 ) ;
#105889 = ADVANCED_FACE ( 'NONE', ( #69857 ), #16855, .T. ) ;
#105890 = CONICAL_SURFACE ( 'NONE', #112159, 0.1000000000000002554, 0.003490658503988666988 ) ;
#105891 = CARTESIAN_POINT ( 'NONE',  ( -1.650000000000035216, 2.500000000000000000, -5.802370205355749988 ) ) ;
#105893 = EDGE_CURVE ( 'NONE', #59034, #107306, #73315, .T. ) ;
#105892 = DIRECTION ( 'NONE',  ( 0.000000000000000000, 1.000000000000000000, 0.000000000000000000 ) ) ;
#105894 = CONICAL_SURFACE ( 'NONE', #70393, 0.1000000000000002554, 0.003490658503988666988 ) ;
#105895 = DIRECTION ( 'NONE',  ( 0.000000000000000000, 1.000000000000000000, 0.000000000000000000 ) ) ;
#105896 = ORIENTED_EDGE ( 'NONE', *, *, #123033, .T. ) ;
#105897 = AXIS2_PLACEMENT_3D ( 'NONE', #76104, #47942, #116020 ) ;
#105898 = EDGE_CURVE ( 'NONE', #42353, #28403, #27335, .T. ) ;
#105899 = DIRECTION ( 'NONE',  ( -0.000000000000000000, -1.000000000000000000, -0.000000000000000000 ) ) ;
#105900 = ORIENTED_EDGE ( 'NONE', *, *, #56890, .T. ) ;
#105901 = CARTESIAN_POINT ( 'NONE',  ( 43.31961220472146579, -2.029667686315419939, -5.113275312223934499 ) ) ;
#105902 = LINE ( 'NONE', #7029, #7866 ) ;
#105903 = CARTESIAN_POINT ( 'NONE',  ( 9.399999999999915090, 2.500000000000000000, -3.983716857408426293 ) ) ;
#105904 = CARTESIAN_POINT ( 'NONE',  ( 18.93069778776427370, -2.571126379696592856, 2.451182541063249953 ) ) ;
#105905 = ADVANCED_FACE ( 'NONE', ( #56778 ), #47638, .T. ) ;
#105906 = CONICAL_SURFACE ( 'NONE', #32776, 0.09999999999999982514, 0.003490658503988666988 ) ;
#105907 = EDGE_CURVE ( 'NONE', #14967, #51095, #47000, .T. ) ;
#105908 = ORIENTED_EDGE ( 'NONE', *, *, #88728, .T. ) ;
#105909 = ADVANCED_FACE ( 'NONE', ( #38483 ), #37822, .T. ) ;
#105912 = EDGE_CURVE ( 'NONE', #80364, #73565, #67232, .T. ) ;
#105911 = CIRCLE ( 'NONE', #49404, 0.09999999999999982514 ) ;
#105910 = AXIS2_PLACEMENT_3D ( 'NONE', #78963, #119501, #60613 ) ;
#105913 = EDGE_LOOP ( 'NONE', ( #6343, #100617 ) ) ;
#105914 = ORIENTED_EDGE ( 'NONE', *, *, #16617, .F. ) ;
#105915 = CARTESIAN_POINT ( 'NONE',  ( -13.74999999999998757, 2.500000000000000000, -2.757883832488651876 ) ) ;
#105916 = DIRECTION ( 'NONE',  ( -4.274815082592931898E-19, -0.9999939076577903929, -0.003490651415223739937 ) ) ;
#105917 = DIRECTION ( 'NONE',  ( -0.000000000000000000, -1.000000000000000000, -0.000000000000000000 ) ) ;
#105918 = FACE_BOUND ( 'NONE', #113428, .T. ) ;
#105919 = CARTESIAN_POINT ( 'NONE',  ( 2.899999999999946620, 2.500000000000000000, -0.5928203230275542746 ) ) ;
#105920 = DIRECTION ( 'NONE',  ( 0.000000000000000000, 1.000000000000000000, 0.000000000000000000 ) ) ;
#105921 = EDGE_CURVE ( 'NONE', #71628, #7939, #78401, .T. ) ;
#105922 = CARTESIAN_POINT ( 'NONE',  ( 14.39999999999989555, 2.500000000000000000, -0.3464101615137782364 ) ) ;
#105923 = DIRECTION ( 'NONE',  ( 0.000000000000000000, 0.000000000000000000, 1.000000000000000000 ) ) ;
#105924 = CARTESIAN_POINT ( 'NONE',  ( 185.0885416670080872, -6.551208109652273848, -3.782341765625003571 ) ) ;
#105925 = DIRECTION ( 'NONE',  ( 0.000000000000000000, 0.000000000000000000, 1.000000000000000000 ) ) ;
#105926 = DIRECTION ( 'NONE',  ( 0.000000000000000000, 0.000000000000000000, 1.000000000000000000 ) ) ;
#105927 = CARTESIAN_POINT ( 'NONE',  ( -1.250000000000001110, 2.500000000000000000, -6.395190528383301931 ) ) ;
#105928 = VERTEX_POINT ( 'NONE', #107841 ) ;
#105929 = ORIENTED_EDGE ( 'NONE', *, *, #70582, .T. ) ;
#105930 = VERTEX_POINT ( 'NONE', #18165 ) ;
#105931 = EDGE_LOOP ( 'NONE', ( #82255, #52021, #124619, #127540 ) ) ;
#105932 = DIRECTION ( 'NONE',  ( 0.000000000000000000, 0.000000000000000000, 1.000000000000000000 ) ) ;
#105933 = EDGE_CURVE ( 'NONE', #38823, #80116, #8343, .T. ) ;
#105934 = FACE_BOUND ( 'NONE', #18523, .T. ) ;
#105935 = FACE_OUTER_BOUND ( 'NONE', #68887, .T. ) ;
#105936 = CIRCLE ( 'NONE', #34858, 0.1000000000000002554 ) ;
#105937 = CONICAL_SURFACE ( 'NONE', #55844, 0.1000000000000000472, 0.003490658503988666988 ) ;
#105938 = ORIENTED_EDGE ( 'NONE', *, *, #62297, .T. ) ;
#105939 = CARTESIAN_POINT ( 'NONE',  ( 11.64999999999990443, 12.50000000000000000, 1.472243186433545459 ) ) ;
#105940 = CARTESIAN_POINT ( 'NONE',  ( 0.5999999999999555689, 12.50000000000000000, 4.676537180435972552 ) ) ;
#105941 = EDGE_LOOP ( 'NONE', ( #99747, #118476 ) ) ;
#105942 = CYLINDRICAL_SURFACE ( 'NONE', #57382, 7.699999999999999289 ) ;
#105943 = CARTESIAN_POINT ( 'NONE',  ( -10.45000000000000462, 2.500000000000000000, -2.065063509461098068 ) ) ;
#105945 = CIRCLE ( 'NONE', #9802, 0.06509327318403745899 ) ;
#105944 = CONICAL_SURFACE ( 'NONE', #66226, 0.09999999999999982514, 0.003490658503988666988 ) ;
#105946 = EDGE_CURVE ( 'NONE', #73985, #92776, #79591, .T. ) ;
#105947 = ORIENTED_EDGE ( 'NONE', *, *, #90454, .T. ) ;
#105948 = FACE_OUTER_BOUND ( 'NONE', #36916, .T. ) ;
#105950 = CONICAL_SURFACE ( 'NONE', #22347, 0.1000000000000000056, 0.003490658503988666988 ) ;
#105949 = CARTESIAN_POINT ( 'NONE',  ( -12.69999999999999396, 2.500000000000000000, -4.083716857408424161 ) ) ;
#105952 = AXIS2_PLACEMENT_3D ( 'NONE', #41230, #20278, #40598 ) ;
#105951 = AXIS2_PLACEMENT_3D ( 'NONE', #62257, #63538, #12491 ) ;
#105953 = EDGE_LOOP ( 'NONE', ( #114917, #13554, #110158, #40690 ) ) ;
#105954 = AXIS2_PLACEMENT_3D ( 'NONE', #110916, #111576, #110286 ) ;
#105955 = CARTESIAN_POINT ( 'NONE',  ( 8.099999999999921485, 12.50000000000000000, -0.2813168883297409439 ) ) ;
#105956 = DIRECTION ( 'NONE',  ( 0.000000000000000000, 1.000000000000000000, 0.000000000000000000 ) ) ;
#105957 = ORIENTED_EDGE ( 'NONE', *, *, #98418, .F. ) ;
#105958 = DIRECTION ( 'NONE',  ( -0.000000000000000000, 1.000000000000000000, -0.000000000000000000 ) ) ;
#105959 = ORIENTED_EDGE ( 'NONE', *, *, #4892, .T. ) ;
#105960 = ORIENTED_EDGE ( 'NONE', *, *, #35577, .F. ) ;
#105961 = EDGE_CURVE ( 'NONE', #92955, #46558, #42027, .T. ) ;
#105962 = PLANE ( 'NONE',  #43133 ) ;
#105963 = ORIENTED_EDGE ( 'NONE', *, *, #46467, .T. ) ;
#105964 = CARTESIAN_POINT ( 'NONE',  ( 5.199999999999935341, 12.50000000000000000, -0.3464101615137783474 ) ) ;
#105965 = CARTESIAN_POINT ( 'NONE',  ( -0.4500000000000402012, 2.500000000000000000, 2.065063509461097624 ) ) ;
#105966 = VERTEX_POINT ( 'NONE', #22056 ) ;
#105967 = DIRECTION ( 'NONE',  ( -0.000000000000000000, 1.000000000000000000, -0.000000000000000000 ) ) ;
#105968 = CARTESIAN_POINT ( 'NONE',  ( 8.949999999999915801, 12.50000000000000000, -1.753560074763288679 ) ) ;
#105969 = FACE_OUTER_BOUND ( 'NONE', #79272, .T. ) ;
#105970 = CARTESIAN_POINT ( 'NONE',  ( 6.049999999999934097, 2.500000000000000000, -6.148780366869526226 ) ) ;
#105971 = DIRECTION ( 'NONE',  ( 0.000000000000000000, 0.000000000000000000, -1.000000000000000000 ) ) ;
#105972 = CONICAL_SURFACE ( 'NONE', #24410, 0.09999999999999982514, 0.003490658503988666988 ) ;
#105974 = AXIS2_PLACEMENT_3D ( 'NONE', #13048, #62827, #60885 ) ;
#105973 = CARTESIAN_POINT ( 'NONE',  ( 17.41716098457701634, 1.872967139268043146, -4.643356076170611857 ) ) ;
#105975 = VECTOR ( 'NONE', #21782, 1000.000000000000000 ) ;
#105976 = EDGE_LOOP ( 'NONE', ( #78076, #123138 ) ) ;
#105977 = VERTEX_POINT ( 'NONE', #112357 ) ;
#105978 = CARTESIAN_POINT ( 'NONE',  ( -2.300000000000033573, 2.500000000000000000, -4.083716857408426826 ) ) ;
#105979 = AXIS2_PLACEMENT_3D ( 'NONE', #45393, #46673, #55212 ) ;
#105980 = DIRECTION ( 'NONE',  ( 0.000000000000000000, 0.000000000000000000, 1.000000000000000000 ) ) ;
#105981 = CARTESIAN_POINT ( 'NONE',  ( 0.8499999999999557909, 12.50000000000000000, -6.560283801567339701 ) ) ;
#105983 = ORIENTED_EDGE ( 'NONE', *, *, #4467, .T. ) ;
#105982 = EDGE_LOOP ( 'NONE', ( #11557, #67078 ) ) ;
#105984 = ORIENTED_EDGE ( 'NONE', *, *, #109057, .F. ) ;
#105985 = FACE_OUTER_BOUND ( 'NONE', #116694, .T. ) ;
#105986 = AXIS2_PLACEMENT_3D ( 'NONE', #105787, #27870, #126720 ) ;
#105987 = CONICAL_SURFACE ( 'NONE', #30702, 0.09999999999999982514, 0.003490658503988666988 ) ;
#105988 = DIRECTION ( 'NONE',  ( 0.000000000000000000, 0.000000000000000000, -1.000000000000000000 ) ) ;
#105989 = DIRECTION ( 'NONE',  ( 0.000000000000000000, 0.000000000000000000, -1.000000000000000000 ) ) ;
#105990 = CONICAL_SURFACE ( 'NONE', #114297, 0.1000000000000000056, 0.003490658503988666988 ) ;
#105991 = EDGE_CURVE ( 'NONE', #18296, #118526, #52477, .T. ) ;
#105992 = DIRECTION ( 'NONE',  ( 1.000000000000000000, 0.000000000000000000, 0.000000000000000000 ) ) ;
#105993 = CARTESIAN_POINT ( 'NONE',  ( 4.399999999999937295, 2.500000000000000000, 3.983716857408420964 ) ) ;
#105994 = CARTESIAN_POINT ( 'NONE',  ( 6.049999999999930544, 12.50000000000000000, 2.511473670974873507 ) ) ;
#105995 = CARTESIAN_POINT ( 'NONE',  ( -13.29999999999999005, 2.500000000000000000, 1.843143693225357538E-15 ) ) ;
#105996 = DIRECTION ( 'NONE',  ( 0.000000000000000000, 1.000000000000000000, 0.000000000000000000 ) ) ;
#105997 = CARTESIAN_POINT ( 'NONE',  ( -3.150000000000033218, 2.500000000000000000, -6.841600689897078702 ) ) ;
#105998 = AXIS2_PLACEMENT_3D ( 'NONE', #70718, #32102, #11137 ) ;
#105999 = FACE_OUTER_BOUND ( 'NONE', #102674, .T. ) ;
#106000 = CIRCLE ( 'NONE', #91327, 0.06509327318403745899 ) ;
#106001 = ORIENTED_EDGE ( 'NONE', *, *, #67390, .F. ) ;
#106003 = CIRCLE ( 'NONE', #122728, 0.1000000000000002554 ) ;
#106002 = VECTOR ( 'NONE', #62541, 1000.000000000000000 ) ;
#106004 = DIRECTION ( 'NONE',  ( 0.000000000000000000, 0.000000000000000000, 1.000000000000000000 ) ) ;
#106005 = EDGE_CURVE ( 'NONE', #45696, #2267, #121505, .T. ) ;
#106006 = VERTEX_POINT ( 'NONE', #50227 ) ;
#106007 = EDGE_CURVE ( 'NONE', #17553, #119696, #87971, .T. ) ;
#106008 = ORIENTED_EDGE ( 'NONE', *, *, #116165, .F. ) ;
#106009 = EDGE_CURVE ( 'NONE', #37406, #11230, #1739, .T. ) ;
#106010 = DIRECTION ( 'NONE',  ( 0.000000000000000000, 1.000000000000000000, 0.000000000000000000 ) ) ;
#106012 = EDGE_CURVE ( 'NONE', #26373, #100348, #56583, .T. ) ;
#106011 = LINE ( 'NONE', #76549, #69810 ) ;
#106013 = DIRECTION ( 'NONE',  ( 0.000000000000000000, 0.000000000000000000, -1.000000000000000000 ) ) ;
#106014 = CARTESIAN_POINT ( 'NONE',  ( 1.899999999999951283, 2.500000000000000000, 0.3464101615137736845 ) ) ;
#106015 = CARTESIAN_POINT ( 'NONE',  ( -2.700000000000029932, 12.50000000000000000, -4.676537180435977881 ) ) ;
#106016 = DIRECTION ( 'NONE',  ( -0.000000000000000000, 1.000000000000000000, -0.000000000000000000 ) ) ;
#106017 = CARTESIAN_POINT ( 'NONE',  ( 5.849999999999933920, 12.50000000000000000, -2.922977105672691422 ) ) ;
#106018 = ORIENTED_EDGE ( 'NONE', *, *, #81654, .T. ) ;
#106019 = CARTESIAN_POINT ( 'NONE',  ( -6.250000000000017764, 2.500000000000000000, 2.857883832488649301 ) ) ;
#106020 = ADVANCED_FACE ( 'NONE', ( #33164 ), #102526, .T. ) ;
#106022 = EDGE_CURVE ( 'NONE', #4486, #11304, #58757, .T. ) ;
#106021 = CARTESIAN_POINT ( 'NONE',  ( -12.94999999999999218, 2.500000000000000000, -2.265063509461099578 ) ) ;
#106023 = ORIENTED_EDGE ( 'NONE', *, *, #44728, .F. ) ;
#106024 = EDGE_CURVE ( 'NONE', #34064, #35601, #125634, .T. ) ;
#106025 = ORIENTED_EDGE ( 'NONE', *, *, #3334, .T. ) ;
#106026 = VERTEX_POINT ( 'NONE', #40409 ) ;
#106027 = EDGE_LOOP ( 'NONE', ( #16824, #88620 ) ) ;
#106028 = DIRECTION ( 'NONE',  ( 0.000000000000000000, -0.9999939076577903929, 0.003490651415223739937 ) ) ;
#106029 = DIRECTION ( 'NONE',  ( 0.000000000000000000, 0.000000000000000000, -1.000000000000000000 ) ) ;
#106030 = CONICAL_SURFACE ( 'NONE', #103882, 0.09999999999999999167, 0.003490658503988666988 ) ;
#106031 = CARTESIAN_POINT ( 'NONE',  ( -12.04999999999999538, 12.50000000000000000, 6.430097255199259010 ) ) ;
#106033 = DIRECTION ( 'NONE',  ( 0.000000000000000000, 0.000000000000000000, 1.000000000000000000 ) ) ;
#106032 = AXIS2_PLACEMENT_3D ( 'NONE', #29738, #90582, #17975 ) ;
#106034 = DIRECTION ( 'NONE',  ( 0.000000000000000000, -0.000000000000000000, 1.000000000000000000 ) ) ;
#106035 = ORIENTED_EDGE ( 'NONE', *, *, #98475, .T. ) ;
#106036 = DIRECTION ( 'NONE',  ( -4.274815082592931898E-19, -0.9999939076577903929, -0.003490651415223739937 ) ) ;
#106037 = CIRCLE ( 'NONE', #89312, 0.06509327318403745899 ) ;
#106038 = DIRECTION ( 'NONE',  ( 0.000000000000000000, 0.000000000000000000, 1.000000000000000000 ) ) ;
#106039 = ORIENTED_EDGE ( 'NONE', *, *, #53365, .F. ) ;
#106040 = CONICAL_SURFACE ( 'NONE', #74746, 0.09999999999999982514, 0.003490658503988666988 ) ;
#106041 = ORIENTED_EDGE ( 'NONE', *, *, #30964, .T. ) ;
#106042 = VERTEX_POINT ( 'NONE', #111709 ) ;
#106043 = CARTESIAN_POINT ( 'NONE',  ( -6.250000000000019540, 2.500000000000000000, -7.088010851410853519 ) ) ;
#106044 = CIRCLE ( 'NONE', #87162, 0.1000000000000002554 ) ;
#106045 = DIRECTION ( 'NONE',  ( 0.000000000000000000, 0.000000000000000000, -1.000000000000000000 ) ) ;
#106046 = CARTESIAN_POINT ( 'NONE',  ( -9.350000000000006750, 12.50000000000000000, 1.818653347947321475 ) ) ;
#106047 = VECTOR ( 'NONE', #70211, 1000.000000000000000 ) ;
#106048 = ORIENTED_EDGE ( 'NONE', *, *, #20340, .T. ) ;
#106049 = FACE_OUTER_BOUND ( 'NONE', #69577, .T. ) ;
#106050 = DIRECTION ( 'NONE',  ( 0.000000000000000000, 0.000000000000000000, 1.000000000000000000 ) ) ;
#106051 = CARTESIAN_POINT ( 'NONE',  ( -12.49999999999999289, 2.500000000000000000, 3.637306695894644726 ) ) ;
#106052 = DIRECTION ( 'NONE',  ( 0.000000000000000000, 1.000000000000000000, 0.000000000000000000 ) ) ;
#106053 = ADVANCED_FACE ( 'NONE', ( #1102 ), #41697, .T. ) ;
#106054 = FACE_OUTER_BOUND ( 'NONE', #55393, .T. ) ;
#106055 = ADVANCED_FACE ( 'NONE', ( #3053 ), #31564, .T. ) ;
#106056 = VERTEX_POINT ( 'NONE', #80326 ) ;
#106057 = AXIS2_PLACEMENT_3D ( 'NONE', #104966, #36265, #75515 ) ;
#106058 = CARTESIAN_POINT ( 'NONE',  ( -7.050000000000013145, 12.50000000000000000, 2.230156782645134950 ) ) ;
#106059 = EDGE_CURVE ( 'NONE', #16889, #127557, #30591, .T. ) ;
#106060 = ORIENTED_EDGE ( 'NONE', *, *, #19780, .T. ) ;
#106061 = VERTEX_POINT ( 'NONE', #81597 ) ;
#106062 = EDGE_LOOP ( 'NONE', ( #31727, #95114, #113145, #67005 ) ) ;
#106063 = DIRECTION ( 'NONE',  ( -4.274815082592931898E-19, -0.9999939076577903929, -0.003490651415223739937 ) ) ;
#106064 = FACE_BOUND ( 'NONE', #73209, .T. ) ;
#106065 = AXIS2_PLACEMENT_3D ( 'NONE', #41117, #100641, #120937 ) ;
#106066 = CARTESIAN_POINT ( 'NONE',  ( -8.550000000000011369, 2.500000000000000000, 1.718653347947321386 ) ) ;
#106067 = CARTESIAN_POINT ( 'NONE',  ( -4.150000000000025224, 2.500000000000000000, 5.802370205355744659 ) ) ;
#106068 = AXIS2_PLACEMENT_3D ( 'NONE', #120457, #42564, #1957 ) ;
#106069 = ADVANCED_FACE ( 'NONE', ( #20750 ), #123489, .T. ) ;
#106070 = CARTESIAN_POINT ( 'NONE',  ( 3.149999999999946176, 12.50000000000000000, -2.446380397790840266 ) ) ;
#106071 = CIRCLE ( 'NONE', #53847, 0.09999999999999982514 ) ;
#106072 = ORIENTED_EDGE ( 'NONE', *, *, #109584, .T. ) ;
#106073 = DIRECTION ( 'NONE',  ( -0.000000000000000000, -1.000000000000000000, -0.000000000000000000 ) ) ;
#106074 = DIRECTION ( 'NONE',  ( 0.000000000000000000, 0.000000000000000000, 1.000000000000000000 ) ) ;
#106076 = DIRECTION ( 'NONE',  ( 0.000000000000000000, 0.000000000000000000, -1.000000000000000000 ) ) ;
#106075 = CONICAL_SURFACE ( 'NONE', #93471, 0.1000000000000000056, 0.003490658503988666988 ) ;
#106078 = CARTESIAN_POINT ( 'NONE',  ( -1.450000000000036371, 2.500000000000000000, 2.511473670974873507 ) ) ;
#106077 = AXIS2_PLACEMENT_3D ( 'NONE', #86120, #25272, #126061 ) ;
#106079 = EDGE_LOOP ( 'NONE', ( #48000, #37388 ) ) ;
#106080 = DIRECTION ( 'NONE',  ( 0.000000000000000000, 0.000000000000000000, 1.000000000000000000 ) ) ;
#106081 = AXIS2_PLACEMENT_3D ( 'NONE', #35987, #15680, #115831 ) ;
#106082 = CIRCLE ( 'NONE', #127022, 0.06509327318403745899 ) ;
#106083 = FACE_OUTER_BOUND ( 'NONE', #50392, .T. ) ;
#106084 = ORIENTED_EDGE ( 'NONE', *, *, #103781, .T. ) ;
#106085 = CARTESIAN_POINT ( 'NONE',  ( 5.599999999999931255, 2.500000000000000000, 4.776537180435972196 ) ) ;
#106086 = AXIS2_PLACEMENT_3D ( 'NONE', #9059, #77165, #20176 ) ;
#106087 = FACE_BOUND ( 'NONE', #9533, .T. ) ;
#106088 = CARTESIAN_POINT ( 'NONE',  ( 179.5000000000000000, -0.6250000000000000000, 7.634788798650553154 ) ) ;
#106090 = AXIS2_PLACEMENT_3D ( 'NONE', #92771, #103874, #62668 ) ;
#106089 = AXIS2_PLACEMENT_3D ( 'NONE', #124018, #14047, #37591 ) ;
#106091 = VERTEX_POINT ( 'NONE', #90772 ) ;
#106092 = LINE ( 'NONE', #8513, #105065 ) ;
#106093 = FACE_OUTER_BOUND ( 'NONE', #103894, .T. ) ;
#106094 = ORIENTED_EDGE ( 'NONE', *, *, #88398, .T. ) ;
#106095 = ORIENTED_EDGE ( 'NONE', *, *, #1557, .T. ) ;
#106096 = CARTESIAN_POINT ( 'NONE',  ( 187.2916666666666572, 4.445597072760120838, -7.699999999999998401 ) ) ;
#106097 = ORIENTED_EDGE ( 'NONE', *, *, #27200, .F. ) ;
#106098 = CARTESIAN_POINT ( 'NONE',  ( 185.0885416670080872, -6.551208109652273848, -3.782341765625003571 ) ) ;
#106099 = CARTESIAN_POINT ( 'NONE',  ( -4.350000000000023626, 2.500000000000000000, 6.841600689897072485 ) ) ;
#106100 = EDGE_CURVE ( 'NONE', #9122, #105841, #46137, .T. ) ;
#106101 = DIRECTION ( 'NONE',  ( 0.000000000000000000, 0.000000000000000000, 1.000000000000000000 ) ) ;
#106102 = CARTESIAN_POINT ( 'NONE',  ( -8.550000000000011369, 2.500000000000000000, 1.818653347947321475 ) ) ;
#106103 = DIRECTION ( 'NONE',  ( 0.000000000000000000, 0.000000000000000000, 1.000000000000000000 ) ) ;
#106104 = AXIS2_PLACEMENT_3D ( 'NONE', #36857, #67573, #117972 ) ;
#106105 = EDGE_LOOP ( 'NONE', ( #110760, #24206, #116992, #31936 ) ) ;
#106106 = DIRECTION ( 'NONE',  ( 0.000000000000000000, 1.000000000000000000, 0.000000000000000000 ) ) ;
#106107 = CARTESIAN_POINT ( 'NONE',  ( 9.999999999999912959, 2.500000000000000000, 3.737306695894644371 ) ) ;
#106108 = DIRECTION ( 'NONE',  ( 0.000000000000000000, -0.9999939076577903929, 0.003490651415223739937 ) ) ;
#106109 = ADVANCED_FACE ( 'NONE', ( #71131 ), #111036, .T. ) ;
#106110 = CARTESIAN_POINT ( 'NONE',  ( 130.5000000000000000, 0.5000000000000000000, -7.500000000000001776 ) ) ;
#106112 = EDGE_LOOP ( 'NONE', ( #75996, #78022 ) ) ;
#106111 = VERTEX_POINT ( 'NONE', #3683 ) ;
#106113 = FACE_BOUND ( 'NONE', #49192, .T. ) ;
#106114 = ORIENTED_EDGE ( 'NONE', *, *, #110114, .F. ) ;
#106115 = EDGE_CURVE ( 'NONE', #95740, #38693, #119286, .T. ) ;
#106116 = DIRECTION ( 'NONE',  ( 0.000000000000000000, 1.000000000000000000, 0.000000000000000000 ) ) ;
#106117 = DIRECTION ( 'NONE',  ( 0.000000000000000000, 0.000000000000000000, -1.000000000000000000 ) ) ;
#106118 = EDGE_LOOP ( 'NONE', ( #112724, #67981, #16323, #69576 ) ) ;
#106119 = PLANE ( 'NONE',  #78600 ) ;
#106120 = CARTESIAN_POINT ( 'NONE',  ( 7.949999999999922018, 12.50000000000000000, 6.430097255199259010 ) ) ;
#106121 = FACE_OUTER_BOUND ( 'NONE', #34846, .T. ) ;
#106122 = CIRCLE ( 'NONE', #24554, 0.06509327318403745899 ) ;
#106123 = CARTESIAN_POINT ( 'NONE',  ( 9.199999999999915801, 12.50000000000000000, -4.265033745738164406 ) ) ;
#106124 = ORIENTED_EDGE ( 'NONE', *, *, #38690, .F. ) ;
#106125 = FACE_OUTER_BOUND ( 'NONE', #120374, .T. ) ;
#106126 = LINE ( 'NONE', #56372, #60647 ) ;
#106127 = EDGE_CURVE ( 'NONE', #29957, #22780, #102559, .T. ) ;
#106128 = CARTESIAN_POINT ( 'NONE',  ( 186.8593750003414016, 0.000000000000000000, 7.564683531250000925 ) ) ;
#106129 = DIRECTION ( 'NONE',  ( 0.000000000000000000, 1.000000000000000000, 0.000000000000000000 ) ) ;
#106130 = CARTESIAN_POINT ( 'NONE',  ( -9.400000000000007461, 12.50000000000000000, 3.983716857408420076 ) ) ;
#106131 = VERTEX_POINT ( 'NONE', #55995 ) ;
#106132 = AXIS2_PLACEMENT_3D ( 'NONE', #111443, #41453, #120635 ) ;
#106134 = ORIENTED_EDGE ( 'NONE', *, *, #1288, .F. ) ;
#106133 = AXIS2_PLACEMENT_3D ( 'NONE', #79821, #47793, #128951 ) ;
#106135 = DIRECTION ( 'NONE',  ( 0.000000000000000000, 0.000000000000000000, -1.000000000000000000 ) ) ;
#106136 = VERTEX_POINT ( 'NONE', #65157 ) ;
#106137 = CARTESIAN_POINT ( 'NONE',  ( 6.849999999999930367, 12.50000000000000000, -6.148780366869526226 ) ) ;
#106139 = ORIENTED_EDGE ( 'NONE', *, *, #112731, .F. ) ;
#106138 = ORIENTED_EDGE ( 'NONE', *, *, #125767, .T. ) ;
#106140 = EDGE_LOOP ( 'NONE', ( #39540, #21524, #58108, #16967 ) ) ;
#106141 = CARTESIAN_POINT ( 'NONE',  ( -8.350000000000013856, 2.500000000000000000, 2.165063509461097713 ) ) ;
#106143 = CARTESIAN_POINT ( 'NONE',  ( 13.74999999999989342, 2.500000000000000000, -1.372243186433550033 ) ) ;
#106142 = VECTOR ( 'NONE', #118496, 1000.000000000000000 ) ;
#106144 = DIRECTION ( 'NONE',  ( 0.000000000000000000, 0.000000000000000000, -1.000000000000000000 ) ) ;
#106145 = ADVANCED_FACE ( 'NONE', ( #53446 ), #54525, .T. ) ;
#106146 = FACE_OUTER_BOUND ( 'NONE', #60231, .T. ) ;
#106147 = LINE ( 'NONE', #85846, #8276 ) ;
#106148 = DIRECTION ( 'NONE',  ( 0.000000000000000000, 0.000000000000000000, 1.000000000000000000 ) ) ;
#106149 = AXIS2_PLACEMENT_3D ( 'NONE', #116792, #18604, #58548 ) ;
#106150 = ORIENTED_EDGE ( 'NONE', *, *, #126217, .T. ) ;
#106151 = CARTESIAN_POINT ( 'NONE',  ( -13.09999999999999076, 12.50000000000000000, 3.983716857408420964 ) ) ;
#106152 = ORIENTED_EDGE ( 'NONE', *, *, #95508, .T. ) ;
#106153 = EDGE_CURVE ( 'NONE', #90081, #80887, #105088, .T. ) ;
#106154 = AXIS2_PLACEMENT_3D ( 'NONE', #75797, #66624, #7049 ) ;
#106155 = ORIENTED_EDGE ( 'NONE', *, *, #1546, .F. ) ;
#106156 = EDGE_LOOP ( 'NONE', ( #19743, #59685, #104220, #14319 ) ) ;
#106157 = ORIENTED_EDGE ( 'NONE', *, *, #8467, .F. ) ;
#106158 = AXIS2_PLACEMENT_3D ( 'NONE', #111607, #122082, #72346 ) ;
#106159 = CARTESIAN_POINT ( 'NONE',  ( 2.099999999999949463, 2.500000000000000000, -3.537306695894649966 ) ) ;
#106160 = EDGE_CURVE ( 'NONE', #48527, #12263, #113029, .T. ) ;
#106161 = ORIENTED_EDGE ( 'NONE', *, *, #68193, .F. ) ;
#106162 = ADVANCED_FACE ( 'NONE', ( #55368 ), #67041, .T. ) ;
#106163 = VERTEX_POINT ( 'NONE', #103826 ) ;
#106164 = EDGE_CURVE ( 'NONE', #93502, #50283, #114276, .T. ) ;
#106165 = AXIS2_PLACEMENT_3D ( 'NONE', #67003, #57859, #58514 ) ;
#106166 = ADVANCED_FACE ( 'NONE', ( #95292 ), #35726, .T. ) ;
#106167 = VECTOR ( 'NONE', #123670, 1000.000000000000114 ) ;
#106168 = CARTESIAN_POINT ( 'NONE',  ( -2.900000000000029221, 12.50000000000000000, -4.957854068765716882 ) ) ;
#106170 = VECTOR ( 'NONE', #74824, 1000.000000000000000 ) ;
#106169 = DIRECTION ( 'NONE',  ( 0.000000000000000000, 0.000000000000000000, 1.000000000000000000 ) ) ;
#106171 = DIRECTION ( 'NONE',  ( 0.000000000000000000, 1.000000000000000000, 0.000000000000000000 ) ) ;
#106172 = CARTESIAN_POINT ( 'NONE',  ( 6.849999999999930367, 2.500000000000000000, -6.841600689897078702 ) ) ;
#106173 = EDGE_CURVE ( 'NONE', #115875, #60164, #117208, .T. ) ;
#106174 = CARTESIAN_POINT ( 'NONE',  ( 8.299999999999922551, 2.500000000000000000, 4.330127018922196314 ) ) ;
#106175 = EDGE_LOOP ( 'NONE', ( #76232, #67683 ) ) ;
#106176 = EDGE_CURVE ( 'NONE', #127833, #82531, #85463, .T. ) ;
#106177 = VECTOR ( 'NONE', #129172, 1000.000000000000000 ) ;
#106178 = CARTESIAN_POINT ( 'NONE',  ( -2.900000000000029221, 2.500000000000000000, 0.09999999999999772959 ) ) ;
#106179 = ADVANCED_FACE ( 'NONE', ( #83546 ), #121434, .T. ) ;
#106180 = EDGE_LOOP ( 'NONE', ( #86490, #127339, #41464, #41741 ) ) ;
#106181 = AXIS2_PLACEMENT_3D ( 'NONE', #117619, #75784, #128123 ) ;
#106182 = DIRECTION ( 'NONE',  ( -4.274815082592931898E-19, -0.9999939076577903929, -0.003490651415223739937 ) ) ;
#106183 = EDGE_CURVE ( 'NONE', #16039, #84307, #94251, .T. ) ;
#106184 = ORIENTED_EDGE ( 'NONE', *, *, #23535, .T. ) ;
#106185 = DIRECTION ( 'NONE',  ( 0.000000000000000000, 0.000000000000000000, 1.000000000000000000 ) ) ;
#106186 = ORIENTED_EDGE ( 'NONE', *, *, #3868, .F. ) ;
#106187 = AXIS2_PLACEMENT_3D ( 'NONE', #78960, #119500, #96624 ) ;
#106188 = ORIENTED_EDGE ( 'NONE', *, *, #62246, .F. ) ;
#106189 = EDGE_CURVE ( 'NONE', #104360, #52455, #247, .T. ) ;
#106190 = CARTESIAN_POINT ( 'NONE',  ( -9.350000000000006750, 12.50000000000000000, 2.511473670974873507 ) ) ;
#106191 = FACE_OUTER_BOUND ( 'NONE', #35300, .T. ) ;
#106192 = AXIS2_PLACEMENT_3D ( 'NONE', #102935, #112129, #51289 ) ;
#106193 = CARTESIAN_POINT ( 'NONE',  ( -4.150000000000024336, 2.500000000000000000, -2.857883832488653741 ) ) ;
#106194 = CARTESIAN_POINT ( 'NONE',  ( 185.2500000000000000, 9.429780353434619030E-16, -7.700000000000000178 ) ) ;
#106195 = DIRECTION ( 'NONE',  ( 0.000000000000000000, 1.000000000000000000, 0.000000000000000000 ) ) ;
#106196 = ORIENTED_EDGE ( 'NONE', *, *, #113835, .T. ) ;
#106197 = DIRECTION ( 'NONE',  ( 0.000000000000000000, 0.000000000000000000, -1.000000000000000000 ) ) ;
#106198 = CARTESIAN_POINT ( 'NONE',  ( 8.749999999999920064, 12.50000000000000000, -2.792790559304616504 ) ) ;
#106199 = DIRECTION ( 'NONE',  ( -0.000000000000000000, -1.000000000000000000, -0.000000000000000000 ) ) ;
#106200 = CARTESIAN_POINT ( 'NONE',  ( 12.49999999999990230, 12.50000000000000000, -0.6928203230275541413 ) ) ;
#106201 = DIRECTION ( 'NONE',  ( -0.000000000000000000, -1.000000000000000000, -0.000000000000000000 ) ) ;
#106202 = EDGE_LOOP ( 'NONE', ( #55297, #26255 ) ) ;
#106203 = ORIENTED_EDGE ( 'NONE', *, *, #15112, .F. ) ;
#106204 = LINE ( 'NONE', #26361, #113292 ) ;
#106205 = ORIENTED_EDGE ( 'NONE', *, *, #89942, .T. ) ;
#106206 = DIRECTION ( 'NONE',  ( 0.000000000000000000, 1.000000000000000000, 0.000000000000000000 ) ) ;
#106207 = DIRECTION ( 'NONE',  ( 0.000000000000000000, 1.000000000000000000, 0.000000000000000000 ) ) ;
#106208 = AXIS2_PLACEMENT_3D ( 'NONE', #10488, #20327, #119810 ) ;
#106210 = ORIENTED_EDGE ( 'NONE', *, *, #44438, .F. ) ;
#106209 = CIRCLE ( 'NONE', #49790, 0.09999999999999982514 ) ;
#106211 = CARTESIAN_POINT ( 'NONE',  ( 185.4583333333333144, 4.445597072760117285, 7.699999999999999289 ) ) ;
#106212 = LINE ( 'NONE', #97672, #91232 ) ;
#106213 = CARTESIAN_POINT ( 'NONE',  ( -10.65000000000000213, 2.500000000000000000, 1.818653347947321475 ) ) ;
#106214 = CARTESIAN_POINT ( 'NONE',  ( 2.499999999999947153, 2.500000000000000000, 3.537306695894645081 ) ) ;
#106215 = ORIENTED_EDGE ( 'NONE', *, *, #62137, .T. ) ;
#106216 = CONICAL_SURFACE ( 'NONE', #108266, 0.1000000000000002554, 0.003490658503988666988 ) ;
#106217 = EDGE_CURVE ( 'NONE', #109827, #127552, #112995, .T. ) ;
#106218 = CIRCLE ( 'NONE', #74822, 0.1000000000000002554 ) ;
#106219 = DIRECTION ( 'NONE',  ( -0.000000000000000000, 1.000000000000000000, -0.000000000000000000 ) ) ;
#106220 = CARTESIAN_POINT ( 'NONE',  ( 7.099999999999928590, 12.50000000000000000, 4.395220292106234439 ) ) ;
#106221 = ADVANCED_FACE ( 'NONE', ( #73699 ), #4296, .T. ) ;
#106222 = ORIENTED_EDGE ( 'NONE', *, *, #116970, .F. ) ;
#106223 = DIRECTION ( 'NONE',  ( 0.000000000000000000, 0.000000000000000000, 1.000000000000000000 ) ) ;
#106224 = DIRECTION ( 'NONE',  ( -0.000000000000000000, -1.000000000000000000, -0.000000000000000000 ) ) ;
#106225 = CIRCLE ( 'NONE', #97895, 0.09999999999999982514 ) ;
#106226 = CARTESIAN_POINT ( 'NONE',  ( -8.550000000000007816, 2.500000000000000000, 6.248780366869520542 ) ) ;
#106227 = VECTOR ( 'NONE', #608, 1000.000000000000000 ) ;
#106228 = ORIENTED_EDGE ( 'NONE', *, *, #42323, .F. ) ;
#106229 = DIRECTION ( 'NONE',  ( 0.000000000000000000, 1.000000000000000000, 0.000000000000000000 ) ) ;
#106230 = EDGE_LOOP ( 'NONE', ( #37639, #107185, #107426, #58834 ) ) ;
#106231 = DIRECTION ( 'NONE',  ( 0.000000000000000000, 1.000000000000000000, 0.000000000000000000 ) ) ;
#106232 = CARTESIAN_POINT ( 'NONE',  ( -8.550000000000013145, 2.500000000000000000, -6.841600689897073373 ) ) ;
#106233 = CARTESIAN_POINT ( 'NONE',  ( -8.950000000000006395, 2.500000000000000000, 6.841600689897072485 ) ) ;
#106234 = ORIENTED_EDGE ( 'NONE', *, *, #72212, .T. ) ;
#106235 = AXIS2_PLACEMENT_3D ( 'NONE', #84381, #43192, #33371 ) ;
#106236 = CARTESIAN_POINT ( 'NONE',  ( 3.349999999999941025, 2.500000000000000000, 7.188010851410848723 ) ) ;
#106237 = FACE_OUTER_BOUND ( 'NONE', #95258, .T. ) ;
#106238 = CIRCLE ( 'NONE', #49826, 0.09999999999999999167 ) ;
#106239 = VERTEX_POINT ( 'NONE', #74360 ) ;
#106240 = ORIENTED_EDGE ( 'NONE', *, *, #108357, .T. ) ;
#106241 = DIRECTION ( 'NONE',  ( -0.000000000000000000, -1.000000000000000000, -0.000000000000000000 ) ) ;
#106242 = ORIENTED_EDGE ( 'NONE', *, *, #112253, .T. ) ;
#106243 =( GEOMETRIC_REPRESENTATION_CONTEXT ( 3 ) GLOBAL_UNCERTAINTY_ASSIGNED_CONTEXT ( ( #52159 ) ) GLOBAL_UNIT_ASSIGNED_CONTEXT ( ( #103580, #44015, #34197 ) ) REPRESENTATION_CONTEXT ( 'NONE', 'WORKASPACE' ) );
#106244 = CARTESIAN_POINT ( 'NONE',  ( 3.749999999999944045, 2.500000000000000000, -2.757883832488654097 ) ) ;
#106245 = FACE_OUTER_BOUND ( 'NONE', #77979, .T. ) ;
#106246 = ORIENTED_EDGE ( 'NONE', *, *, #30277, .T. ) ;
#106247 = DIRECTION ( 'NONE',  ( -4.274815082592931898E-19, -0.9999939076577903929, -0.003490651415223739937 ) ) ;
#106248 = CARTESIAN_POINT ( 'NONE',  ( 10.44999999999991047, 12.50000000000000000, 2.165063509461097713 ) ) ;
#106249 = AXIS2_PLACEMENT_3D ( 'NONE', #16295, #5833, #24852 ) ;
#106250 = ORIENTED_EDGE ( 'NONE', *, *, #61977, .T. ) ;
#106252 = ADVANCED_FACE ( 'NONE', ( #104458 ), #127792, .T. ) ;
#106251 = DIRECTION ( 'NONE',  ( -0.000000000000000000, -1.000000000000000000, -0.000000000000000000 ) ) ;
#106253 = DIRECTION ( 'NONE',  ( 0.000000000000000000, 0.000000000000000000, -1.000000000000000000 ) ) ;
#106254 = CONICAL_SURFACE ( 'NONE', #62357, 0.1000000000000000472, 0.003490658503988666988 ) ;
#106255 = FACE_OUTER_BOUND ( 'NONE', #87637, .T. ) ;
#106256 = CARTESIAN_POINT ( 'NONE',  ( 12.89999999999990266, 12.50000000000000000, 5.022947341949748790 ) ) ;
#106257 = CARTESIAN_POINT ( 'NONE',  ( 10.64999999999990976, 2.500000000000000000, -6.048780366869526581 ) ) ;
#106258 = CARTESIAN_POINT ( 'NONE',  ( 185.1979166673494603, 6.668395609140176816, 3.850000000000000977 ) ) ;
#106259 = VERTEX_POINT ( 'NONE', #114912 ) ;
#106260 = EDGE_LOOP ( 'NONE', ( #49873, #22505, #80094, #60680 ) ) ;
#106261 = ORIENTED_EDGE ( 'NONE', *, *, #26232, .T. ) ;
#106262 = VERTEX_POINT ( 'NONE', #84815 ) ;
#106263 = DIRECTION ( 'NONE',  ( -0.000000000000000000, 1.000000000000000000, -0.000000000000000000 ) ) ;
#106264 = DIRECTION ( 'NONE',  ( 0.000000000000000000, 1.000000000000000000, 0.000000000000000000 ) ) ;
#106265 = ADVANCED_FACE ( 'NONE', ( #88691 ), #90122, .T. ) ;
#106266 = CARTESIAN_POINT ( 'NONE',  ( -8.749999999999975131, 12.50000000000000000, -2.165063509461101710 ) ) ;
#106267 = AXIS2_PLACEMENT_3D ( 'NONE', #121221, #123780, #42692 ) ;
#106268 = EDGE_LOOP ( 'NONE', ( #108582, #97315, #90284, #84588 ) ) ;
#106269 = FACE_BOUND ( 'NONE', #93996, .T. ) ;
#106270 = EDGE_CURVE ( 'NONE', #107875, #63897, #6477, .T. ) ;
#106271 = DIRECTION ( 'NONE',  ( 0.000000000000000000, -0.000000000000000000, 1.000000000000000000 ) ) ;
#106272 = DIRECTION ( 'NONE',  ( 0.000000000000000000, 1.000000000000000000, 0.000000000000000000 ) ) ;
#106273 = CARTESIAN_POINT ( 'NONE',  ( 9.149999999999920419, 12.50000000000000000, 2.857883832488649301 ) ) ;
#106275 = CIRCLE ( 'NONE', #41460, 0.09999999999999982514 ) ;
#106274 = CONICAL_SURFACE ( 'NONE', #35190, 0.1000000000000000472, 0.003490658503988666988 ) ;
#106276 = FACE_OUTER_BOUND ( 'NONE', #12335, .T. ) ;
#106277 = FACE_OUTER_BOUND ( 'NONE', #118776, .T. ) ;
#106278 = DIRECTION ( 'NONE',  ( -0.000000000000000000, 1.000000000000000000, -0.000000000000000000 ) ) ;
#106279 = CARTESIAN_POINT ( 'NONE',  ( -14.79999999999998295, 2.500000000000000000, -0.3464101615137760715 ) ) ;
#106280 = DIRECTION ( 'NONE',  ( 0.000000000000000000, 0.000000000000000000, 1.000000000000000000 ) ) ;
#106281 = EDGE_CURVE ( 'NONE', #23602, #64836, #68396, .T. ) ;
#106282 = LINE ( 'NONE', #6132, #99629 ) ;
#106283 = DIRECTION ( 'NONE',  ( -0.000000000000000000, 1.000000000000000000, -0.000000000000000000 ) ) ;
#106284 = ORIENTED_EDGE ( 'NONE', *, *, #85798, .F. ) ;
#106285 = EDGE_LOOP ( 'NONE', ( #48933, #115433 ) ) ;
#106286 = ORIENTED_EDGE ( 'NONE', *, *, #58873, .F. ) ;
#106287 = VERTEX_POINT ( 'NONE', #88015 ) ;
#106288 = DIRECTION ( 'NONE',  ( 0.000000000000000000, 1.000000000000000000, 0.000000000000000000 ) ) ;
#106289 = AXIS2_PLACEMENT_3D ( 'NONE', #32716, #3869, #74546 ) ;
#106290 = DIRECTION ( 'NONE',  ( 0.000000000000000000, 0.000000000000000000, -1.000000000000000000 ) ) ;
#106291 = EDGE_LOOP ( 'NONE', ( #47895, #17102 ) ) ;
#106292 = ORIENTED_EDGE ( 'NONE', *, *, #105381, .F. ) ;
#106293 = DIRECTION ( 'NONE',  ( 0.000000000000000000, 0.000000000000000000, -1.000000000000000000 ) ) ;
#106294 = CIRCLE ( 'NONE', #66571, 0.06509327318403745899 ) ;
#106295 = AXIS2_PLACEMENT_3D ( 'NONE', #120817, #20052, #31169 ) ;
#106296 = DIRECTION ( 'NONE',  ( 0.000000000000000000, 1.000000000000000000, 0.000000000000000000 ) ) ;
#106298 = DIRECTION ( 'NONE',  ( -0.000000000000000000, -1.000000000000000000, -0.000000000000000000 ) ) ;
#106297 = VECTOR ( 'NONE', #25319, 1000.000000000000000 ) ;
#106299 = CARTESIAN_POINT ( 'NONE',  ( -11.69999999999999929, 2.500000000000000000, -4.230127018922199333 ) ) ;
#106300 = DIRECTION ( 'NONE',  ( -0.000000000000000000, -1.000000000000000000, -0.000000000000000000 ) ) ;
#106301 = EDGE_LOOP ( 'NONE', ( #88689, #97680, #110411, #77170 ) ) ;
#106302 = CIRCLE ( 'NONE', #70794, 0.1000000000000002554 ) ;
#106303 = AXIS2_PLACEMENT_3D ( 'NONE', #20353, #22305, #61580 ) ;
#106304 = ORIENTED_EDGE ( 'NONE', *, *, #104282, .T. ) ;
#106305 = EDGE_CURVE ( 'NONE', #20680, #55512, #71343, .T. ) ;
#106306 = AXIS2_PLACEMENT_3D ( 'NONE', #52873, #2457, #71215 ) ;
#106307 = ORIENTED_EDGE ( 'NONE', *, *, #38958, .F. ) ;
#106308 = ORIENTED_EDGE ( 'NONE', *, *, #129402, .F. ) ;
#106309 = EDGE_LOOP ( 'NONE', ( #46975, #79366 ) ) ;
#106310 = EDGE_CURVE ( 'NONE', #25449, #20272, #38984, .T. ) ;
#106311 = VERTEX_POINT ( 'NONE', #48776 ) ;
#106313 = EDGE_CURVE ( 'NONE', #45263, #6533, #113120, .T. ) ;
#106312 = CONICAL_SURFACE ( 'NONE', #45779, 0.1000000000000000472, 0.003490658503988666988 ) ;
#106314 = DIRECTION ( 'NONE',  ( -0.000000000000000000, 1.000000000000000000, -0.000000000000000000 ) ) ;
#106315 = DIRECTION ( 'NONE',  ( 0.000000000000000000, 0.000000000000000000, 1.000000000000000000 ) ) ;
#106316 = PLANE ( 'NONE',  #70833 ) ;
#106317 = CARTESIAN_POINT ( 'NONE',  ( -6.071532165918824830E-15, 2.500000000000000000, -4.330127018922201643 ) ) ;
#106318 = ADVANCED_FACE ( 'NONE', ( #49427 ), #28489, .T. ) ;
#106319 = EDGE_CURVE ( 'NONE', #86214, #125645, #29590, .T. ) ;
#106320 = CARTESIAN_POINT ( 'NONE',  ( 7.099999999999926814, 2.500000000000000000, -0.5928203230275541635 ) ) ;
#106321 = CARTESIAN_POINT ( 'NONE',  ( 10.79999999999991367, 12.50000000000000000, -2.385244779468109755E-15 ) ) ;
#106322 = EDGE_CURVE ( 'NONE', #122166, #59725, #88052, .T. ) ;
#106323 = EDGE_LOOP ( 'NONE', ( #23493, #352 ) ) ;
#106324 = DIRECTION ( 'NONE',  ( 0.000000000000000000, 0.000000000000000000, -1.000000000000000000 ) ) ;
#106325 = CIRCLE ( 'NONE', #8115, 0.09999999999999982514 ) ;
#106326 = ORIENTED_EDGE ( 'NONE', *, *, #128440, .F. ) ;
#106327 = DIRECTION ( 'NONE',  ( 0.000000000000000000, 0.000000000000000000, 1.000000000000000000 ) ) ;
#106328 = EDGE_CURVE ( 'NONE', #8654, #105036, #108951, .T. ) ;
#106329 = ORIENTED_EDGE ( 'NONE', *, *, #103535, .T. ) ;
#106330 = DIRECTION ( 'NONE',  ( 0.000000000000000000, 0.000000000000000000, 1.000000000000000000 ) ) ;
#106331 = CARTESIAN_POINT ( 'NONE',  ( 9.999999999999948486, 2.500000000000000000, -4.330127018922201643 ) ) ;
#106332 = AXIS2_PLACEMENT_3D ( 'NONE', #48018, #10016, #97742 ) ;
#106333 = AXIS2_PLACEMENT_3D ( 'NONE', #24735, #27294, #65285 ) ;
#106334 = ORIENTED_EDGE ( 'NONE', *, *, #72385, .T. ) ;
#106335 = DIRECTION ( 'NONE',  ( -0.000000000000000000, 1.000000000000000000, -0.000000000000000000 ) ) ;
#106336 = CARTESIAN_POINT ( 'NONE',  ( -8.550000000000009592, 2.500000000000000000, 6.941600689897073018 ) ) ;
#106337 = EDGE_LOOP ( 'NONE', ( #18749, #64295 ) ) ;
#106338 = EDGE_CURVE ( 'NONE', #83523, #85122, #10695, .T. ) ;
#106339 = DIRECTION ( 'NONE',  ( 0.000000000000000000, 0.000000000000000000, -1.000000000000000000 ) ) ;
#106340 = ORIENTED_EDGE ( 'NONE', *, *, #1380, .T. ) ;
#106341 = ORIENTED_EDGE ( 'NONE', *, *, #53289, .F. ) ;
#106342 = DIRECTION ( 'NONE',  ( -0.000000000000000000, -1.000000000000000000, -0.000000000000000000 ) ) ;
#106343 = CARTESIAN_POINT ( 'NONE',  ( -0.6500000000000398792, 2.500000000000000000, -2.511473670974877948 ) ) ;
#106344 = CARTESIAN_POINT ( 'NONE',  ( 185.9218750003414016, 0.000000000000000000, 7.564683531250000925 ) ) ;
#106346 = AXIS2_PLACEMENT_3D ( 'NONE', #8110, #38234, #65738 ) ;
#106345 = CARTESIAN_POINT ( 'NONE',  ( -7.900000000000011013, 12.50000000000000000, 4.265033745738159077 ) ) ;
#106347 = CONICAL_SURFACE ( 'NONE', #93827, 0.1000000000000002554, 0.003490658503988666988 ) ;
#106348 = DIRECTION ( 'NONE',  ( -0.000000000000000000, -1.000000000000000000, -0.000000000000000000 ) ) ;
#106349 = DIRECTION ( 'NONE',  ( -0.000000000000000000, -1.000000000000000000, -0.000000000000000000 ) ) ;
#106350 = CIRCLE ( 'NONE', #91686, 0.1000000000000002554 ) ;
#106351 = EDGE_LOOP ( 'NONE', ( #105296, #103060 ) ) ;
#106352 = DIRECTION ( 'NONE',  ( 0.000000000000000000, -0.000000000000000000, 1.000000000000000000 ) ) ;
#106353 = ORIENTED_EDGE ( 'NONE', *, *, #100305, .F. ) ;
#106355 = AXIS2_PLACEMENT_3D ( 'NONE', #24142, #115068, #3218 ) ;
#106354 = VECTOR ( 'NONE', #110690, 1000.000000000000000 ) ;
#106356 = AXIS2_PLACEMENT_3D ( 'NONE', #64560, #63930, #103855 ) ;
#106357 = DIRECTION ( 'NONE',  ( 0.000000000000000000, 1.000000000000000000, 0.000000000000000000 ) ) ;
#106358 = CARTESIAN_POINT ( 'NONE',  ( -11.05000000000000249, 2.500000000000000000, -1.818653347947322141 ) ) ;
#106359 = CARTESIAN_POINT ( 'NONE',  ( -8.350000000000012079, 2.500000000000000000, -2.857883832488653741 ) ) ;
#106360 = CARTESIAN_POINT ( 'NONE',  ( -1.900000000000034106, 12.50000000000000000, 0.3464101615137735735 ) ) ;
#106361 = ORIENTED_EDGE ( 'NONE', *, *, #12176, .T. ) ;
#106363 = AXIS2_PLACEMENT_3D ( 'NONE', #84959, #63396, #34602 ) ;
#106362 = AXIS2_PLACEMENT_3D ( 'NONE', #109882, #42436, #21493 ) ;
#106364 = EDGE_CURVE ( 'NONE', #16861, #7100, #17346, .T. ) ;
#106365 = DIRECTION ( 'NONE',  ( -0.000000000000000000, -1.000000000000000000, -0.000000000000000000 ) ) ;
#106366 = CARTESIAN_POINT ( 'NONE',  ( 6.249999999999932498, 2.500000000000000000, 5.902370205355745192 ) ) ;
#106367 = ORIENTED_EDGE ( 'NONE', *, *, #14908, .T. ) ;
#106368 = CARTESIAN_POINT ( 'NONE',  ( 6.249999999999930722, 2.500000000000000000, 7.188010851410848723 ) ) ;
#106369 = ADVANCED_FACE ( 'NONE', ( #59251 ), #67758, .T. ) ;
#106370 = ORIENTED_EDGE ( 'NONE', *, *, #85536, .T. ) ;
#106371 = ORIENTED_EDGE ( 'NONE', *, *, #57550, .T. ) ;
#106372 = FACE_OUTER_BOUND ( 'NONE', #23530, .T. ) ;
#106373 = AXIS2_PLACEMENT_3D ( 'NONE', #47675, #57491, #127518 ) ;
#106374 = ORIENTED_EDGE ( 'NONE', *, *, #43108, .F. ) ;
#106375 = DIRECTION ( 'NONE',  ( 0.000000000000000000, 0.000000000000000000, -1.000000000000000000 ) ) ;
#106376 = DIRECTION ( 'NONE',  ( 0.000000000000000000, 0.000000000000000000, 1.000000000000000000 ) ) ;
#106377 = CARTESIAN_POINT ( 'NONE',  ( -2.050000000000032685, 2.500000000000000000, -2.165063509461101710 ) ) ;
#106378 = EDGE_LOOP ( 'NONE', ( #45598, #116137, #44003, #57716 ) ) ;
#106379 = VECTOR ( 'NONE', #79795, 1000.000000000000000 ) ;
#106380 = FACE_BOUND ( 'NONE', #52143, .T. ) ;
#106382 = EDGE_LOOP ( 'NONE', ( #6959, #118229 ) ) ;
#106381 = LINE ( 'NONE', #65146, #56258 ) ;
#106383 = DIRECTION ( 'NONE',  ( 0.000000000000000000, 0.000000000000000000, -1.000000000000000000 ) ) ;
#106384 = CARTESIAN_POINT ( 'NONE',  ( 9.599999999999914380, 2.500000000000000000, -4.330127018922201643 ) ) ;
#106385 = AXIS2_PLACEMENT_3D ( 'NONE', #10696, #51318, #31040 ) ;
#106386 = ORIENTED_EDGE ( 'NONE', *, *, #40576, .F. ) ;
#106387 = AXIS2_PLACEMENT_3D ( 'NONE', #78493, #107925, #69275 ) ;
#106388 = AXIS2_PLACEMENT_3D ( 'NONE', #107105, #76382, #25995 ) ;
#106389 = VERTEX_POINT ( 'NONE', #27185 ) ;
#106390 = ORIENTED_EDGE ( 'NONE', *, *, #7591, .F. ) ;
#106391 = DIRECTION ( 'NONE',  ( 0.000000000000000000, 1.000000000000000000, 0.000000000000000000 ) ) ;
#106392 = CARTESIAN_POINT ( 'NONE',  ( -15.79999999999998117, 2.500000000000000000, 0.1000000000000000056 ) ) ;
#106393 = DIRECTION ( 'NONE',  ( -4.274815082592931898E-19, -0.9999939076577903929, -0.003490651415223739937 ) ) ;
#106394 = FACE_BOUND ( 'NONE', #2367, .T. ) ;
#106395 = ORIENTED_EDGE ( 'NONE', *, *, #73947, .F. ) ;
#106396 = CARTESIAN_POINT ( 'NONE',  ( 185.5677083336747160, -4.367472073101514418, -7.564683531250002702 ) ) ;
#106397 = VECTOR ( 'NONE', #12056, 1000.000000000000000 ) ;
#106398 = CARTESIAN_POINT ( 'NONE',  ( 10.64999999999991331, 12.50000000000000000, 6.148780366869520897 ) ) ;
#106399 = DIRECTION ( 'NONE',  ( -0.000000000000000000, 1.000000000000000000, -0.000000000000000000 ) ) ;
#106401 = EDGE_CURVE ( 'NONE', #41959, #66137, #106847, .T. ) ;
#106400 = CIRCLE ( 'NONE', #100157, 0.06509327318403745899 ) ;
#106402 = FACE_OUTER_BOUND ( 'NONE', #80954, .T. ) ;
#106403 = CARTESIAN_POINT ( 'NONE',  ( 1.049999999999954525, 2.500000000000000000, 1.918653347947321564 ) ) ;
#106404 = CARTESIAN_POINT ( 'NONE',  ( 1.249999999999954259, 12.50000000000000000, -7.188010851410854052 ) ) ;
#106405 = FACE_OUTER_BOUND ( 'NONE', #37810, .T. ) ;
#106406 = DIRECTION ( 'NONE',  ( 0.000000000000000000, 0.000000000000000000, -1.000000000000000000 ) ) ;
#106408 = ADVANCED_FACE ( 'NONE', ( #8185 ), #76943, .T. ) ;
#106407 = AXIS2_PLACEMENT_3D ( 'NONE', #97112, #126581, #76837 ) ;
#106409 = DIRECTION ( 'NONE',  ( -0.000000000000000000, -1.000000000000000000, -0.000000000000000000 ) ) ;
#106410 = ORIENTED_EDGE ( 'NONE', *, *, #112538, .F. ) ;
#106411 = ORIENTED_EDGE ( 'NONE', *, *, #12913, .T. ) ;
#106412 = EDGE_LOOP ( 'NONE', ( #119008, #35431, #111376, #51024 ) ) ;
#106413 = ORIENTED_EDGE ( 'NONE', *, *, #124805, .T. ) ;
#106414 = VERTEX_POINT ( 'NONE', #48130 ) ;
#106415 = AXIS2_PLACEMENT_3D ( 'NONE', #16608, #87286, #87919 ) ;
#106416 = CARTESIAN_POINT ( 'NONE',  ( -2.900000000000030109, 2.500000000000000000, -3.537306695894649966 ) ) ;
#106417 = EDGE_CURVE ( 'NONE', #115797, #68417, #31657, .T. ) ;
#106418 = FACE_OUTER_BOUND ( 'NONE', #31626, .T. ) ;
#106419 = ORIENTED_EDGE ( 'NONE', *, *, #16541, .T. ) ;
#106420 = FACE_BOUND ( 'NONE', #51412, .T. ) ;
#106421 = EDGE_CURVE ( 'NONE', #112463, #76648, #8639, .T. ) ;
#106422 = DIRECTION ( 'NONE',  ( 0.000000000000000000, -0.000000000000000000, 1.000000000000000000 ) ) ;
#106423 = AXIS2_PLACEMENT_3D ( 'NONE', #6819, #56577, #76248 ) ;
#106424 = EDGE_CURVE ( 'NONE', #128284, #16041, #115235, .T. ) ;
#106425 = DIRECTION ( 'NONE',  ( 0.000000000000000000, 1.000000000000000000, 0.000000000000000000 ) ) ;
#106426 = CARTESIAN_POINT ( 'NONE',  ( 5.449999999999934452, 2.500000000000000000, 2.265063509461097357 ) ) ;
#106427 = CARTESIAN_POINT ( 'NONE',  ( -0.6000000000000323963, 12.50000000000000000, 0.3464101615137759604 ) ) ;
#106428 = EDGE_CURVE ( 'NONE', #32665, #72747, #81456, .T. ) ;
#106429 = DIRECTION ( 'NONE',  ( -0.000000000000000000, -1.000000000000000000, -0.000000000000000000 ) ) ;
#106430 = EDGE_LOOP ( 'NONE', ( #36407, #66748 ) ) ;
#106431 = CIRCLE ( 'NONE', #102334, 0.06509327318403745899 ) ;
#106432 = DIRECTION ( 'NONE',  ( 0.000000000000000000, 0.000000000000000000, -1.000000000000000000 ) ) ;
#106434 = VERTEX_POINT ( 'NONE', #82090 ) ;
#106433 = AXIS2_PLACEMENT_3D ( 'NONE', #43619, #103816, #42988 ) ;
#106435 = ORIENTED_EDGE ( 'NONE', *, *, #65847, .F. ) ;
#106436 = EDGE_LOOP ( 'NONE', ( #98926, #77316, #42, #27856 ) ) ;
#106437 = CARTESIAN_POINT ( 'NONE',  ( -7.050000000000016698, 2.500000000000000000, -6.495190528383302464 ) ) ;
#106438 = DIRECTION ( 'NONE',  ( 0.000000000000000000, 0.000000000000000000, -1.000000000000000000 ) ) ;
#106439 = PLANE ( 'NONE',  #121999 ) ;
#106440 = AXIS2_PLACEMENT_3D ( 'NONE', #30496, #62526, #82153 ) ;
#106441 = ORIENTED_EDGE ( 'NONE', *, *, #69363, .F. ) ;
#106442 = DIRECTION ( 'NONE',  ( -0.000000000000000000, -1.000000000000000000, -0.000000000000000000 ) ) ;
#106443 = DIRECTION ( 'NONE',  ( 0.000000000000000000, 0.000000000000000000, 1.000000000000000000 ) ) ;
#106446 = AXIS2_PLACEMENT_3D ( 'NONE', #81606, #128810, #100593 ) ;
#106445 = DIRECTION ( 'NONE',  ( -0.000000000000000000, 1.000000000000000000, -0.000000000000000000 ) ) ;
#106444 = AXIS2_PLACEMENT_3D ( 'NONE', #26673, #39090, #126157 ) ;
#106447 = CARTESIAN_POINT ( 'NONE',  ( 184.3229166673494603, -4.445597072760122614, 7.699999999999998401 ) ) ;
#106448 = FACE_OUTER_BOUND ( 'NONE', #114952, .T. ) ;
#106449 = CARTESIAN_POINT ( 'NONE',  ( 12.09999999999990550, 2.500000000000000000, -4.922947341949753586 ) ) ;
#106450 = AXIS2_PLACEMENT_3D ( 'NONE', #95959, #36416, #48157 ) ;
#106451 = DIRECTION ( 'NONE',  ( 0.000000000000000000, 1.000000000000000000, 0.000000000000000000 ) ) ;
#106452 = VERTEX_POINT ( 'NONE', #10135 ) ;
#106453 = PLANE ( 'NONE',  #106892 ) ;
#106455 = VECTOR ( 'NONE', #118285, 1000.000000000000000 ) ;
#106454 = AXIS2_PLACEMENT_3D ( 'NONE', #103923, #45011, #35827 ) ;
#106456 = ORIENTED_EDGE ( 'NONE', *, *, #40576, .T. ) ;
#106457 = ORIENTED_EDGE ( 'NONE', *, *, #103796, .F. ) ;
#106458 = FACE_OUTER_BOUND ( 'NONE', #27531, .T. ) ;
#106459 = DIRECTION ( 'NONE',  ( 0.000000000000000000, 0.000000000000000000, -1.000000000000000000 ) ) ;
#106460 = CARTESIAN_POINT ( 'NONE',  ( -8.750000000000010658, 12.50000000000000000, 2.857883832488649301 ) ) ;
#106461 = ORIENTED_EDGE ( 'NONE', *, *, #24860, .T. ) ;
#106463 = EDGE_CURVE ( 'NONE', #92990, #77408, #52579, .T. ) ;
#106462 = ORIENTED_EDGE ( 'NONE', *, *, #114965, .T. ) ;
#106464 = CARTESIAN_POINT ( 'NONE',  ( -7.499999999999980460, 12.50000000000000000, -4.330127018922201643 ) ) ;
#106465 = DIRECTION ( 'NONE',  ( 0.000000000000000000, 0.000000000000000000, -1.000000000000000000 ) ) ;
#106467 = EDGE_CURVE ( 'NONE', #36022, #61453, #54622, .T. ) ;
#106466 = DIRECTION ( 'NONE',  ( 0.000000000000000000, 1.000000000000000000, 0.000000000000000000 ) ) ;
#106469 = EDGE_LOOP ( 'NONE', ( #44988, #19126, #109860, #1386, #42774 ) ) ;
#106468 = AXIS2_PLACEMENT_3D ( 'NONE', #46070, #66338, #106271 ) ;
#106470 = ORIENTED_EDGE ( 'NONE', *, *, #40688, .F. ) ;
#106471 = ADVANCED_FACE ( 'NONE', ( #52624 ), #41545, .T. ) ;
#106472 = LINE ( 'NONE', #6954, #115018 ) ;
#106473 = ADVANCED_FACE ( 'NONE', ( #89967 ), #12842, .T. ) ;
#106474 = ADVANCED_FACE ( 'NONE', ( #21231 ), #123578, .T. ) ;
#106475 = EDGE_LOOP ( 'NONE', ( #55182, #87534, #45639, #87455 ) ) ;
#106476 = CARTESIAN_POINT ( 'NONE',  ( -6.900000000000019007, 2.500000000000000000, 0.3464101615137735735 ) ) ;
#106477 = AXIS2_PLACEMENT_3D ( 'NONE', #114406, #115039, #64664 ) ;
#106479 = PLANE ( 'NONE',  #84649 ) ;
#106478 = VECTOR ( 'NONE', #83793, 1000.000000000000000 ) ;
#106480 = ORIENTED_EDGE ( 'NONE', *, *, #114715, .T. ) ;
#106481 = CARTESIAN_POINT ( 'NONE',  ( 1.449999999999950440, 12.50000000000000000, 6.148780366869520009 ) ) ;
#106482 = EDGE_CURVE ( 'NONE', #935, #83109, #83869, .T. ) ;
#106483 = FACE_OUTER_BOUND ( 'NONE', #121880, .T. ) ;
#106484 = CARTESIAN_POINT ( 'NONE',  ( 8.349999999999923261, 12.50000000000000000, 2.792790559304612064 ) ) ;
#106485 = CARTESIAN_POINT ( 'NONE',  ( -6.050000000000017586, 2.500000000000000000, 6.048780366869520364 ) ) ;
#106486 = CIRCLE ( 'NONE', #37545, 0.06509327318403745899 ) ;
#106487 = ORIENTED_EDGE ( 'NONE', *, *, #45714, .T. ) ;
#106489 = ADVANCED_FACE ( 'NONE', ( #72287 ), #96384, .T. ) ;
#106488 = AXIS2_PLACEMENT_3D ( 'NONE', #92817, #23401, #63343 ) ;
#106490 = DIRECTION ( 'NONE',  ( 0.000000000000000000, 0.000000000000000000, 1.000000000000000000 ) ) ;
#106491 = EDGE_CURVE ( 'NONE', #111625, #35458, #69289, .T. ) ;
#106492 = DIRECTION ( 'NONE',  ( 0.000000000000000000, 0.000000000000000000, 1.000000000000000000 ) ) ;
#106493 = ORIENTED_EDGE ( 'NONE', *, *, #104834, .F. ) ;
#106494 = EDGE_LOOP ( 'NONE', ( #95850, #93147, #63008, #68090 ) ) ;
#106495 = CARTESIAN_POINT ( 'NONE',  ( -0.6500000000000398792, 2.500000000000000000, -6.741600689897078169 ) ) ;
#106496 = CARTESIAN_POINT ( 'NONE',  ( 10.39999999999991509, 2.500000000000000000, -0.6928203230275542523 ) ) ;
#106497 = CARTESIAN_POINT ( 'NONE',  ( 10.84999999999990905, 2.500000000000000000, 2.957883832488649389 ) ) ;
#106498 = DIRECTION ( 'NONE',  ( 0.000000000000000000, 0.000000000000000000, 1.000000000000000000 ) ) ;
#106499 = CARTESIAN_POINT ( 'NONE',  ( -11.89999999999999680, 2.500000000000000000, -3.983716857408423628 ) ) ;
#106500 = DIRECTION ( 'NONE',  ( 0.000000000000000000, 0.000000000000000000, 1.000000000000000000 ) ) ;
#106501 = VECTOR ( 'NONE', #32201, 1000.000000000000000 ) ;
#106502 = CARTESIAN_POINT ( 'NONE',  ( 18.00406199218825876, 1.510509990051560170, -4.944015969580407344 ) ) ;
#106503 = DIRECTION ( 'NONE',  ( 0.000000000000000000, -0.000000000000000000, 1.000000000000000000 ) ) ;
#106504 = DIRECTION ( 'NONE',  ( 0.000000000000000000, -0.000000000000000000, 1.000000000000000000 ) ) ;
#106505 = CARTESIAN_POINT ( 'NONE',  ( 13.09999999999989839, 2.500000000000000000, 0.2464101615137735679 ) ) ;
#106506 = ORIENTED_EDGE ( 'NONE', *, *, #52520, .T. ) ;
#106507 = ORIENTED_EDGE ( 'NONE', *, *, #23526, .T. ) ;
#106508 = AXIS2_PLACEMENT_3D ( 'NONE', #23075, #102909, #44012 ) ;
#106509 = DIRECTION ( 'NONE',  ( -0.000000000000000000, -1.000000000000000000, -0.000000000000000000 ) ) ;
#106510 = ORIENTED_EDGE ( 'NONE', *, *, #63862, .F. ) ;
#106511 = FACE_OUTER_BOUND ( 'NONE', #114033, .T. ) ;
#106512 = DIRECTION ( 'NONE',  ( -0.000000000000000000, -1.000000000000000000, -0.000000000000000000 ) ) ;
#106513 = DIRECTION ( 'NONE',  ( -0.000000000000000000, 1.000000000000000000, -0.000000000000000000 ) ) ;
#106514 = VERTEX_POINT ( 'NONE', #121360 ) ;
#106515 = DIRECTION ( 'NONE',  ( 0.000000000000000000, 0.000000000000000000, 1.000000000000000000 ) ) ;
#106516 = LINE ( 'NONE', #96051, #111855 ) ;
#106518 = ORIENTED_EDGE ( 'NONE', *, *, #119044, .T. ) ;
#106517 = DIRECTION ( 'NONE',  ( 0.000000000000000000, 0.000000000000000000, 1.000000000000000000 ) ) ;
#106519 = DIRECTION ( 'NONE',  ( 0.000000000000000000, -0.9999939076577903929, 0.003490651415223739937 ) ) ;
#106520 = ORIENTED_EDGE ( 'NONE', *, *, #48272, .F. ) ;
#106521 = EDGE_CURVE ( 'NONE', #55512, #72078, #79522, .T. ) ;
#106522 = ORIENTED_EDGE ( 'NONE', *, *, #51756, .T. ) ;
#106523 = ORIENTED_EDGE ( 'NONE', *, *, #72879, .T. ) ;
#106524 = ORIENTED_EDGE ( 'NONE', *, *, #80871, .T. ) ;
#106525 = DIRECTION ( 'NONE',  ( 0.000000000000000000, -0.000000000000000000, 1.000000000000000000 ) ) ;
#106526 = CIRCLE ( 'NONE', #108592, 0.06509327318403745899 ) ;
#106527 = FACE_OUTER_BOUND ( 'NONE', #97520, .T. ) ;
#106528 = LINE ( 'NONE', #15562, #125712 ) ;
#106529 = FACE_OUTER_BOUND ( 'NONE', #3670, .T. ) ;
#106530 = ORIENTED_EDGE ( 'NONE', *, *, #85308, .F. ) ;
#106532 = AXIS2_PLACEMENT_3D ( 'NONE', #124758, #54086, #12214 ) ;
#106531 = CONICAL_SURFACE ( 'NONE', #96160, 0.1000000000000000472, 0.003490658503988666988 ) ;
#106533 = CARTESIAN_POINT ( 'NONE',  ( -9.200000000000006395, 12.50000000000000000, -2.385244779468109755E-15 ) ) ;
#106534 = EDGE_LOOP ( 'NONE', ( #102765, #123248, #117425, #61664 ) ) ;
#106535 = DIRECTION ( 'NONE',  ( -0.000000000000000000, -1.000000000000000000, -0.000000000000000000 ) ) ;
#106537 = VECTOR ( 'NONE', #1463, 1000.000000000000000 ) ;
#106536 = CARTESIAN_POINT ( 'NONE',  ( 13.39473262194572101, -2.500000000000000000, -7.044698189558706858 ) ) ;
#106538 = CARTESIAN_POINT ( 'NONE',  ( -4.800000000000024691, 12.50000000000000000, 0.3464101615137735735 ) ) ;
#106539 = CARTESIAN_POINT ( 'NONE',  ( -4.350000000000023626, 12.50000000000000000, -1.818653347947325916 ) ) ;
#106540 = VERTEX_POINT ( 'NONE', #70338 ) ;
#106542 = AXIS2_PLACEMENT_3D ( 'NONE', #125063, #13150, #125688 ) ;
#106541 = AXIS2_PLACEMENT_3D ( 'NONE', #29094, #11364, #39571 ) ;
#106543 = ORIENTED_EDGE ( 'NONE', *, *, #117971, .F. ) ;
#106544 = ORIENTED_EDGE ( 'NONE', *, *, #116089, .F. ) ;
#106545 = DIRECTION ( 'NONE',  ( 0.000000000000000000, -0.9999939076577903929, 0.003490651415223739937 ) ) ;
#106546 = DIRECTION ( 'NONE',  ( 0.000000000000000000, 0.000000000000000000, 1.000000000000000000 ) ) ;
#106547 = DIRECTION ( 'NONE',  ( -4.274815082592931898E-19, -0.9999939076577903929, -0.003490651415223739937 ) ) ;
#106548 = FACE_BOUND ( 'NONE', #38523, .T. ) ;
#106549 = CARTESIAN_POINT ( 'NONE',  ( 127.5000000000000000, 1.500000000000000000, 6.000000000000000000 ) ) ;
#106550 = FACE_OUTER_BOUND ( 'NONE', #30152, .T. ) ;
#106551 = PLANE ( 'NONE',  #39287 ) ;
#106552 = DIRECTION ( 'NONE',  ( 0.000000000000000000, 0.000000000000000000, 1.000000000000000000 ) ) ;
#106553 = CARTESIAN_POINT ( 'NONE',  ( 185.7552083336747444, 6.551208109652275624, -3.782341765624998686 ) ) ;
#106554 = CARTESIAN_POINT ( 'NONE',  ( 0.6499999999999561684, 2.500000000000000000, 2.411473670974873862 ) ) ;
#106555 = DIRECTION ( 'NONE',  ( -4.274815082592931898E-19, -0.9999939076577903929, -0.003490651415223739937 ) ) ;
#106556 = AXIS2_PLACEMENT_3D ( 'NONE', #109598, #19930, #81430 ) ;
#106557 = EDGE_CURVE ( 'NONE', #8586, #113064, #12684, .T. ) ;
#106558 = DIRECTION ( 'NONE',  ( 0.000000000000000000, 0.000000000000000000, 1.000000000000000000 ) ) ;
#106559 = ORIENTED_EDGE ( 'NONE', *, *, #87975, .T. ) ;
#106560 = ORIENTED_EDGE ( 'NONE', *, *, #94154, .F. ) ;
#106561 = ORIENTED_EDGE ( 'NONE', *, *, #116275, .F. ) ;
#106562 = ORIENTED_EDGE ( 'NONE', *, *, #40519, .T. ) ;
#106563 = ADVANCED_FACE ( 'NONE', ( #110261 ), #77607, .T. ) ;
#106564 = CARTESIAN_POINT ( 'NONE',  ( 11.44999999999990870, 2.500000000000000000, -1.918653347947326004 ) ) ;
#106565 = FACE_BOUND ( 'NONE', #50022, .T. ) ;
#106566 = ADVANCED_FACE ( 'NONE', ( #10741 ), #21273, .T. ) ;
#106567 = DIRECTION ( 'NONE',  ( 0.000000000000000000, 0.000000000000000000, 1.000000000000000000 ) ) ;
#106569 = AXIS2_PLACEMENT_3D ( 'NONE', #30833, #88425, #29527 ) ;
#106568 = CIRCLE ( 'NONE', #48010, 0.06509327318403743123 ) ;
#106570 = DIRECTION ( 'NONE',  ( 0.000000000000000000, 1.000000000000000000, 0.000000000000000000 ) ) ;
#106571 = ADVANCED_FACE ( 'NONE', ( #951 ), #39621, .T. ) ;
#106572 = ADVANCED_FACE ( 'NONE', ( #51365 ), #91913, .T. ) ;
#106573 = EDGE_LOOP ( 'NONE', ( #94618, #23331 ) ) ;
#106574 = CARTESIAN_POINT ( 'NONE',  ( -11.05000000000000249, 2.500000000000000000, -1.718653347947322052 ) ) ;
#106575 = EDGE_CURVE ( 'NONE', #77408, #92990, #23320, .T. ) ;
#106576 = PLANE ( 'NONE',  #85442 ) ;
#106577 = ADVANCED_FACE ( 'NONE', ( #13979 ), #52670, .T. ) ;
#106578 = CONICAL_SURFACE ( 'NONE', #110692, 0.09999999999999982514, 0.003490658503988666988 ) ;
#106579 = EDGE_LOOP ( 'NONE', ( #85976, #110372, #65180, #23254 ) ) ;
#106580 = DIRECTION ( 'NONE',  ( -4.274815082592931898E-19, -0.9999939076577903929, -0.003490651415223739937 ) ) ;
#106581 = CARTESIAN_POINT ( 'NONE',  ( 18.70618316909983392, 2.558637580971244496, -2.503050677946455416 ) ) ;
#106582 = CIRCLE ( 'NONE', #125370, 0.06509327318403745899 ) ;
#106583 = CIRCLE ( 'NONE', #123313, 0.1000000000000002554 ) ;
#106584 = EDGE_LOOP ( 'NONE', ( #84081, #33839 ) ) ;
#106585 = DIRECTION ( 'NONE',  ( 0.000000000000000000, 1.000000000000000000, 0.000000000000000000 ) ) ;
#106588 = ADVANCED_FACE ( 'NONE', ( #42846 ), #33011, .T. ) ;
#106587 = CONICAL_SURFACE ( 'NONE', #43918, 0.09999999999999982514, 0.003490658503988666988 ) ;
#106586 = CARTESIAN_POINT ( 'NONE',  ( -3.950000000000024603, 2.500000000000000000, 1.718653347947321386 ) ) ;
#106589 = CONICAL_SURFACE ( 'NONE', #117033, 0.09999999999999982514, 0.003490658503988666988 ) ;
#106590 = VERTEX_POINT ( 'NONE', #53923 ) ;
#106591 = DIRECTION ( 'NONE',  ( 0.000000000000000000, 1.000000000000000000, 0.000000000000000000 ) ) ;
#106592 = DIRECTION ( 'NONE',  ( 0.000000000000000000, 1.000000000000000000, 0.000000000000000000 ) ) ;
#106593 = VERTEX_POINT ( 'NONE', #54543 ) ;
#106594 = CARTESIAN_POINT ( 'NONE',  ( -1.650000000000035660, 2.500000000000000000, 7.288010851410849256 ) ) ;
#106595 = CIRCLE ( 'NONE', #94088, 0.06509327318403745899 ) ;
#106596 = ORIENTED_EDGE ( 'NONE', *, *, #19105, .F. ) ;
#106597 = VERTEX_POINT ( 'NONE', #84667 ) ;
#106598 = CARTESIAN_POINT ( 'NONE',  ( 9.349999999999919709, 2.500000000000000000, -6.841600689897078702 ) ) ;
#106599 = ORIENTED_EDGE ( 'NONE', *, *, #113890, .T. ) ;
#106600 = LINE ( 'NONE', #25444, #95120 ) ;
#106601 = DIRECTION ( 'NONE',  ( 0.000000000000000000, 1.000000000000000000, 0.000000000000000000 ) ) ;
#106602 = ORIENTED_EDGE ( 'NONE', *, *, #99721, .F. ) ;
#106603 = DIRECTION ( 'NONE',  ( 0.000000000000000000, 0.000000000000000000, 1.000000000000000000 ) ) ;
#106604 = DIRECTION ( 'NONE',  ( 0.000000000000000000, 0.000000000000000000, 1.000000000000000000 ) ) ;
#106605 = LINE ( 'NONE', #66040, #54937 ) ;
#106606 = DIRECTION ( 'NONE',  ( 0.000000000000000000, 0.000000000000000000, -1.000000000000000000 ) ) ;
#106607 = EDGE_CURVE ( 'NONE', #63275, #59954, #96473, .T. ) ;
#106608 = FACE_OUTER_BOUND ( 'NONE', #110528, .T. ) ;
#106609 = CARTESIAN_POINT ( 'NONE',  ( 17.50000000000011369, 2.262047038896492612, -3.993694673355268066 ) ) ;
#106610 = VERTEX_POINT ( 'NONE', #74856 ) ;
#106611 = ORIENTED_EDGE ( 'NONE', *, *, #44545, .T. ) ;
#106612 = DIRECTION ( 'NONE',  ( 0.000000000000000000, 1.000000000000000000, 0.000000000000000000 ) ) ;
#106613 = DIRECTION ( 'NONE',  ( 0.000000000000000000, 0.000000000000000000, 1.000000000000000000 ) ) ;
#106615 = ADVANCED_FACE ( 'NONE', ( #82757 ), #35581, .T. ) ;
#106614 = FACE_OUTER_BOUND ( 'NONE', #90040, .T. ) ;
#106617 = EDGE_LOOP ( 'NONE', ( #24091, #72589 ) ) ;
#106616 = ORIENTED_EDGE ( 'NONE', *, *, #17340, .T. ) ;
#106618 = EDGE_LOOP ( 'NONE', ( #102508, #97277, #126841, #54607 ) ) ;
#106619 = EDGE_CURVE ( 'NONE', #61864, #104101, #14614, .T. ) ;
#106620 = VECTOR ( 'NONE', #88925, 1000.000000000000000 ) ;
#106621 = DIRECTION ( 'NONE',  ( 0.000000000000000000, 0.000000000000000000, -1.000000000000000000 ) ) ;
#106622 = ADVANCED_FACE ( 'NONE', ( #64379 ), #19202, .T. ) ;
#106623 = DIRECTION ( 'NONE',  ( 0.000000000000000000, 0.000000000000000000, -1.000000000000000000 ) ) ;
#106624 = DIRECTION ( 'NONE',  ( 0.000000000000000000, 1.000000000000000000, 0.000000000000000000 ) ) ;
#106625 = ADVANCED_FACE ( 'NONE', ( #93848 ), #114765, .T. ) ;
#106626 = PRODUCT_CONTEXT ( 'NONE', #53873, 'mechanical' ) ;
#106628 = AXIS2_PLACEMENT_3D ( 'NONE', #42336, #75017, #12839 ) ;
#106627 = VECTOR ( 'NONE', #63714, 1000.000000000000000 ) ;
#106629 = DIRECTION ( 'NONE',  ( -0.000000000000000000, -1.000000000000000000, -0.000000000000000000 ) ) ;
#106630 = DIRECTION ( 'NONE',  ( -4.274815082592931898E-19, -0.9999939076577903929, -0.003490651415223739937 ) ) ;
#106631 = DIRECTION ( 'NONE',  ( 0.000000000000000000, -0.9999939076577903929, 0.003490651415223739937 ) ) ;
#106632 = CARTESIAN_POINT ( 'NONE',  ( 6.249999999999928946, 2.500000000000000000, 2.857883832488649301 ) ) ;
#106633 = CARTESIAN_POINT ( 'NONE',  ( 9.149999999999918643, 2.500000000000000000, 2.065063509461097624 ) ) ;
#106634 = EDGE_CURVE ( 'NONE', #90933, #112226, #119464, .T. ) ;
#106635 = EDGE_CURVE ( 'NONE', #39561, #65655, #63135, .T. ) ;
#106636 = CARTESIAN_POINT ( 'NONE',  ( -2.300000000000032685, 2.500000000000000000, -4.776537180435978414 ) ) ;
#106637 = ADVANCED_FACE ( 'NONE', ( #74209 ), #38002, .T. ) ;
#106638 = AXIS2_PLACEMENT_3D ( 'NONE', #95735, #17123, #47282 ) ;
#106640 = EDGE_LOOP ( 'NONE', ( #13552, #46099 ) ) ;
#106639 = EDGE_CURVE ( 'NONE', #92080, #46749, #81901, .T. ) ;
#106641 = ADVANCED_FACE ( 'NONE', ( #115385 ), #85306, .T. ) ;
#106642 = DIRECTION ( 'NONE',  ( 0.000000000000000000, -1.000000000000000000, -0.000000000000000000 ) ) ;
#106643 = EDGE_LOOP ( 'NONE', ( #93231, #75135 ) ) ;
#106644 = ORIENTED_EDGE ( 'NONE', *, *, #54149, .T. ) ;
#106645 = CARTESIAN_POINT ( 'NONE',  ( -9.350000000000004974, 12.50000000000000000, 6.148780366869520897 ) ) ;
#106646 = DIRECTION ( 'NONE',  ( 0.000000000000000000, -0.000000000000000000, 1.000000000000000000 ) ) ;
#106647 = CARTESIAN_POINT ( 'NONE',  ( 0.8499999999999536815, 12.50000000000000000, 5.737276932171707422 ) ) ;
#106648 = EDGE_CURVE ( 'NONE', #96223, #75562, #12944, .T. ) ;
#106649 = FACE_OUTER_BOUND ( 'NONE', #6624, .T. ) ;
#106650 = DIRECTION ( 'NONE',  ( -0.000000000000000000, -1.000000000000000000, -0.000000000000000000 ) ) ;
#106651 = CARTESIAN_POINT ( 'NONE',  ( -11.05000000000000071, 2.500000000000000000, -6.841600689897075149 ) ) ;
#106652 = DIRECTION ( 'NONE',  ( -0.000000000000000000, 1.000000000000000000, -0.000000000000000000 ) ) ;
#106653 = EDGE_LOOP ( 'NONE', ( #6850, #14700 ) ) ;
#106654 = DIRECTION ( 'NONE',  ( -0.000000000000000000, 1.000000000000000000, -0.000000000000000000 ) ) ;
#106655 = DIRECTION ( 'NONE',  ( -4.274815082592931898E-19, -0.9999939076577903929, -0.003490651415223739937 ) ) ;
#106656 = VERTEX_POINT ( 'NONE', #65662 ) ;
#106657 = CIRCLE ( 'NONE', #8440, 0.1000000000000002554 ) ;
#106658 = EDGE_LOOP ( 'NONE', ( #83, #14985, #73656, #121410 ) ) ;
#106659 = ORIENTED_EDGE ( 'NONE', *, *, #109368, .F. ) ;
#106660 = ORIENTED_EDGE ( 'NONE', *, *, #59997, .T. ) ;
#106661 = VERTEX_POINT ( 'NONE', #105609 ) ;
#106662 = CARTESIAN_POINT ( 'NONE',  ( 1.049999999999954525, 2.500000000000000000, -2.611473670974877592 ) ) ;
#106663 = CARTESIAN_POINT ( 'NONE',  ( -11.25000000000000000, 12.50000000000000000, -2.857883832488649745 ) ) ;
#106664 = VECTOR ( 'NONE', #120388, 1000.000000000000000 ) ;
#106665 = ORIENTED_EDGE ( 'NONE', *, *, #85031, .F. ) ;
#106666 = CARTESIAN_POINT ( 'NONE',  ( -10.00000000000000355, 12.50000000000000000, -0.6928203230275541413 ) ) ;
#106667 = CARTESIAN_POINT ( 'NONE',  ( -6.250000000000021316, 2.500000000000000000, -5.902370205355750521 ) ) ;
#106668 = FACE_OUTER_BOUND ( 'NONE', #106494, .T. ) ;
#106669 = ORIENTED_EDGE ( 'NONE', *, *, #75127, .F. ) ;
#106670 = CARTESIAN_POINT ( 'NONE',  ( 12.49999999999993960, 2.500000000000000000, -4.430127018922202176 ) ) ;
#106671 = VECTOR ( 'NONE', #73097, 1000.000000000000000 ) ;
#106672 = CARTESIAN_POINT ( 'NONE',  ( -8.350000000000008527, 2.500000000000000000, 7.088010851410848190 ) ) ;
#106673 = VECTOR ( 'NONE', #64183, 1000.000000000000000 ) ;
#106674 = ORIENTED_EDGE ( 'NONE', *, *, #89787, .F. ) ;
#106675 = AXIS2_PLACEMENT_3D ( 'NONE', #98981, #13647, #108785 ) ;
#106676 = EDGE_CURVE ( 'NONE', #37339, #89951, #104885, .T. ) ;
#106677 = VERTEX_POINT ( 'NONE', #112848 ) ;
#106678 = ORIENTED_EDGE ( 'NONE', *, *, #128287, .F. ) ;
#106679 = DIRECTION ( 'NONE',  ( 0.000000000000000000, 1.000000000000000000, 0.000000000000000000 ) ) ;
#106680 = VECTOR ( 'NONE', #113149, 1000.000000000000000 ) ;
#106681 = DIRECTION ( 'NONE',  ( 0.000000000000000000, 0.000000000000000000, 1.000000000000000000 ) ) ;
#106682 = CIRCLE ( 'NONE', #75381, 0.1000000000000002554 ) ;
#106683 = ORIENTED_EDGE ( 'NONE', *, *, #35200, .T. ) ;
#106684 = DIRECTION ( 'NONE',  ( -0.000000000000000000, -1.000000000000000000, -0.000000000000000000 ) ) ;
#106685 = CARTESIAN_POINT ( 'NONE',  ( -8.550000000000014921, 12.50000000000000000, -6.148780366869520897 ) ) ;
#106686 = ADVANCED_FACE ( 'NONE', ( #83392 ), #73499, .T. ) ;
#106687 = DIRECTION ( 'NONE',  ( 0.000000000000000000, 0.000000000000000000, 1.000000000000000000 ) ) ;
#106688 = CARTESIAN_POINT ( 'NONE',  ( -9.150000000000009237, 12.50000000000000000, -2.857883832488653741 ) ) ;
#106689 = ORIENTED_EDGE ( 'NONE', *, *, #40403, .F. ) ;
#106690 = FACE_OUTER_BOUND ( 'NONE', #123178, .T. ) ;
#106691 = ORIENTED_EDGE ( 'NONE', *, *, #78854, .F. ) ;
#106692 = ORIENTED_EDGE ( 'NONE', *, *, #110405, .T. ) ;
#106693 = EDGE_LOOP ( 'NONE', ( #94138, #10275, #66608, #4407 ) ) ;
#106694 = DIRECTION ( 'NONE',  ( 0.000000000000000000, 0.000000000000000000, 1.000000000000000000 ) ) ;
#106695 = FACE_BOUND ( 'NONE', #16435, .T. ) ;
#106696 = DIRECTION ( 'NONE',  ( 0.000000000000000000, 0.000000000000000000, 1.000000000000000000 ) ) ;
#106697 = DIRECTION ( 'NONE',  ( 0.000000000000000000, 0.000000000000000000, 1.000000000000000000 ) ) ;
#106698 = DIRECTION ( 'NONE',  ( -0.000000000000000000, 1.000000000000000000, -0.000000000000000000 ) ) ;
#106699 = AXIS2_PLACEMENT_3D ( 'NONE', #17428, #18736, #7617 ) ;
#106700 = VERTEX_POINT ( 'NONE', #107534 ) ;
#106702 = AXIS2_PLACEMENT_3D ( 'NONE', #12275, #123520, #101326 ) ;
#106701 = CARTESIAN_POINT ( 'NONE',  ( 6.849999999999930367, 2.500000000000000000, -6.048780366869526581 ) ) ;
#106703 = LINE ( 'NONE', #47160, #61526 ) ;
#106704 = CARTESIAN_POINT ( 'NONE',  ( -9.150000000000005684, 2.500000000000000000, 6.495190528383297135 ) ) ;
#106705 = CARTESIAN_POINT ( 'NONE',  ( -14.14999999999998792, 2.500000000000000000, 2.857883832488652853 ) ) ;
#106706 = ORIENTED_EDGE ( 'NONE', *, *, #95407, .F. ) ;
#106707 = CARTESIAN_POINT ( 'NONE',  ( 14.59999999999989484, 2.500000000000000000, 0.5928203230275495006 ) ) ;
#106708 = ADVANCED_FACE ( 'NONE', ( #128481 ), #63049, .T. ) ;
#106709 = AXIS2_PLACEMENT_3D ( 'NONE', #51335, #80128, #91881 ) ;
#106710 = DIRECTION ( 'NONE',  ( -0.000000000000000000, 1.000000000000000000, -0.000000000000000000 ) ) ;
#106711 = ORIENTED_EDGE ( 'NONE', *, *, #76312, .T. ) ;
#106712 = CARTESIAN_POINT ( 'NONE',  ( -7.100000000000013856, 2.500000000000000000, 4.922947341949748257 ) ) ;
#106713 = DIRECTION ( 'NONE',  ( 0.000000000000000000, 0.000000000000000000, -1.000000000000000000 ) ) ;
#106714 = FACE_BOUND ( 'NONE', #118609, .T. ) ;
#106715 = ADVANCED_FACE ( 'NONE', ( #28337 ), #17028, .T. ) ;
#106716 = CARTESIAN_POINT ( 'NONE',  ( 142.3152275665817115, 2.500000000000000000, 2.763522878056728693 ) ) ;
#106717 = EDGE_LOOP ( 'NONE', ( #91693, #7400, #90967, #92626 ) ) ;
#106718 = FACE_OUTER_BOUND ( 'NONE', #63669, .T. ) ;
#106719 = ADVANCED_FACE ( 'NONE', ( #125868 ), #117985, .T. ) ;
#106720 = VERTEX_POINT ( 'NONE', #8029 ) ;
#106721 = EDGE_CURVE ( 'NONE', #54523, #82469, #329, .T. ) ;
#106722 = EDGE_LOOP ( 'NONE', ( #13899, #95598, #53588, #48680 ) ) ;
#106723 = DIRECTION ( 'NONE',  ( -4.274815082592931898E-19, -0.9999939076577903929, -0.003490651415223739937 ) ) ;
#106724 = ADVANCED_FACE ( 'NONE', ( #68243 ), #67205, .T. ) ;
#106725 = EDGE_CURVE ( 'NONE', #30920, #55758, #48468, .T. ) ;
#106726 = CARTESIAN_POINT ( 'NONE',  ( 187.2500000000000000, 9.429780353434619030E-16, -7.700000000000000178 ) ) ;
#106727 = EDGE_CURVE ( 'NONE', #19758, #69648, #36227, .T. ) ;
#106728 = VERTEX_POINT ( 'NONE', #127190 ) ;
#106729 = CARTESIAN_POINT ( 'NONE',  ( -8.150000000000012790, 12.50000000000000000, 2.446380397790835826 ) ) ;
#106730 = DIRECTION ( 'NONE',  ( -0.000000000000000000, -1.000000000000000000, -0.000000000000000000 ) ) ;
#106731 = DIRECTION ( 'NONE',  ( -0.000000000000000000, -1.000000000000000000, -0.000000000000000000 ) ) ;
#106732 = CARTESIAN_POINT ( 'NONE',  ( 185.6562500006828031, 8.891194145520236347, 5.444286225454521982E-16 ) ) ;
#106733 = EDGE_CURVE ( 'NONE', #66584, #41461, #75638, .T. ) ;
#106734 = EDGE_CURVE ( 'NONE', #126401, #75118, #76789, .T. ) ;
#106735 = AXIS2_PLACEMENT_3D ( 'NONE', #78006, #117924, #29553 ) ;
#106736 = ADVANCED_FACE ( 'NONE', ( #19124 ), #26409, .T. ) ;
#106737 = CIRCLE ( 'NONE', #18910, 0.1000000000000002554 ) ;
#106738 = VERTEX_POINT ( 'NONE', #46681 ) ;
#106739 = DIRECTION ( 'NONE',  ( -0.000000000000000000, 1.000000000000000000, -0.000000000000000000 ) ) ;
#106740 = DIRECTION ( 'NONE',  ( 0.000000000000000000, 0.000000000000000000, 1.000000000000000000 ) ) ;
#106741 = CARTESIAN_POINT ( 'NONE',  ( 0.8499999999999557909, 12.50000000000000000, -7.188010851410854052 ) ) ;
#106742 = DIRECTION ( 'NONE',  ( 0.000000000000000000, 0.000000000000000000, 1.000000000000000000 ) ) ;
#106743 = ORIENTED_EDGE ( 'NONE', *, *, #73398, .T. ) ;
#106744 = CARTESIAN_POINT ( 'NONE',  ( -10.85000000000000142, 2.500000000000000000, -7.288010851410851032 ) ) ;
#106745 = VERTEX_POINT ( 'NONE', #8658 ) ;
#106746 = DIRECTION ( 'NONE',  ( 0.000000000000000000, 0.000000000000000000, -1.000000000000000000 ) ) ;
#106747 = CARTESIAN_POINT ( 'NONE',  ( 13.74999999999989519, 2.500000000000000000, -2.857883832488653741 ) ) ;
#106748 = AXIS2_PLACEMENT_3D ( 'NONE', #82246, #71778, #52138 ) ;
#106749 = ORIENTED_EDGE ( 'NONE', *, *, #93165, .T. ) ;
#106750 = DIRECTION ( 'NONE',  ( 0.000000000000000000, -0.9999939076577903929, 0.003490651415223739937 ) ) ;
#106751 = DIRECTION ( 'NONE',  ( 0.000000000000000000, 0.000000000000000000, -1.000000000000000000 ) ) ;
#106752 = CARTESIAN_POINT ( 'NONE',  ( -10.65000000000000391, 2.500000000000000000, -2.511473670974873951 ) ) ;
#106753 = DIRECTION ( 'NONE',  ( 0.000000000000000000, 1.000000000000000000, 0.000000000000000000 ) ) ;
#106754 = EDGE_LOOP ( 'NONE', ( #48935, #109044, #16678, #78555 ) ) ;
#106755 = DIRECTION ( 'NONE',  ( 0.000000000000000000, 1.000000000000000000, 0.000000000000000000 ) ) ;
#106756 = CARTESIAN_POINT ( 'NONE',  ( -5.650000000000023448, 2.500000000000000000, -2.411473670974877859 ) ) ;
#106757 = DIRECTION ( 'NONE',  ( -0.000000000000000000, -1.000000000000000000, -0.000000000000000000 ) ) ;
#106758 = DIRECTION ( 'NONE',  ( -0.000000000000000000, -1.000000000000000000, -0.000000000000000000 ) ) ;
#106759 = DIRECTION ( 'NONE',  ( -4.274815082592931898E-19, -0.9999939076577903929, -0.003490651415223739937 ) ) ;
#106760 = CIRCLE ( 'NONE', #90032, 0.1000000000000000472 ) ;
#106761 = ORIENTED_EDGE ( 'NONE', *, *, #10260, .F. ) ;
#106762 = AXIS2_PLACEMENT_3D ( 'NONE', #23979, #36388, #63249 ) ;
#106763 = EDGE_LOOP ( 'NONE', ( #37008, #7690, #49115, #61489 ) ) ;
#106764 = DIRECTION ( 'NONE',  ( 0.000000000000000000, 1.846105847067148761E-16, 1.000000000000000000 ) ) ;
#106765 = VERTEX_POINT ( 'NONE', #106244 ) ;
#106766 = CARTESIAN_POINT ( 'NONE',  ( 11.89999999999990798, 12.50000000000000000, 4.611443907251934426 ) ) ;
#106768 = ORIENTED_EDGE ( 'NONE', *, *, #5764, .F. ) ;
#106767 = ORIENTED_EDGE ( 'NONE', *, *, #41319, .F. ) ;
#106769 = EDGE_LOOP ( 'NONE', ( #102446, #20977, #10154, #65635 ) ) ;
#106770 = DIRECTION ( 'NONE',  ( 0.000000000000000000, 0.000000000000000000, 1.000000000000000000 ) ) ;
#106771 = AXIS2_PLACEMENT_3D ( 'NONE', #32692, #72596, #22864 ) ;
#106772 = CARTESIAN_POINT ( 'NONE',  ( -15.59999999999998010, 2.500000000000000000, 0.3464101615137759604 ) ) ;
#106773 = DIRECTION ( 'NONE',  ( 0.000000000000000000, 0.000000000000000000, -1.000000000000000000 ) ) ;
#106774 = CARTESIAN_POINT ( 'NONE',  ( 10.59999999999991260, 2.500000000000000000, 0.3464101615137735735 ) ) ;
#106775 = AXIS2_PLACEMENT_3D ( 'NONE', #89984, #80181, #118808 ) ;
#106776 = DIRECTION ( 'NONE',  ( -0.000000000000000000, 1.000000000000000000, -0.000000000000000000 ) ) ;
#106777 = DIRECTION ( 'NONE',  ( 0.000000000000000000, 1.000000000000000000, 0.000000000000000000 ) ) ;
#106778 = EDGE_LOOP ( 'NONE', ( #109670, #112047, #39416, #94698 ) ) ;
#106779 = EDGE_CURVE ( 'NONE', #82663, #115112, #86097, .T. ) ;
#106780 = FACE_OUTER_BOUND ( 'NONE', #33226, .T. ) ;
#106781 = ORIENTED_EDGE ( 'NONE', *, *, #98807, .T. ) ;
#106782 = ADVANCED_FACE ( 'NONE', ( #57797 ), #48616, .F. ) ;
#106783 = ORIENTED_EDGE ( 'NONE', *, *, #122220, .T. ) ;
#106784 = EDGE_LOOP ( 'NONE', ( #77069, #53482 ) ) ;
#106785 = ORIENTED_EDGE ( 'NONE', *, *, #28316, .F. ) ;
#106786 = EDGE_CURVE ( 'NONE', #120673, #127817, #10783, .T. ) ;
#106787 = CARTESIAN_POINT ( 'NONE',  ( 2.899999999999944844, 2.500000000000000000, 3.637306695894644726 ) ) ;
#106788 = ORIENTED_EDGE ( 'NONE', *, *, #40833, .T. ) ;
#106789 = EDGE_LOOP ( 'NONE', ( #28073, #101649, #87446, #12412 ) ) ;
#106790 = EDGE_CURVE ( 'NONE', #14841, #896, #127811, .T. ) ;
#106791 = CARTESIAN_POINT ( 'NONE',  ( -9.600000000000006750, 2.500000000000000000, 3.737306695894644371 ) ) ;
#106792 = DIRECTION ( 'NONE',  ( 0.000000000000000000, 0.000000000000000000, -1.000000000000000000 ) ) ;
#106793 = CARTESIAN_POINT ( 'NONE',  ( 13.14999999999989733, 12.50000000000000000, -1.818653347947325916 ) ) ;
#106794 = DIRECTION ( 'NONE',  ( 0.000000000000000000, 1.000000000000000000, 0.000000000000000000 ) ) ;
#106795 = CIRCLE ( 'NONE', #90070, 0.1000000000000002554 ) ;
#106796 = DIRECTION ( 'NONE',  ( 0.000000000000000000, 0.000000000000000000, -1.000000000000000000 ) ) ;
#106797 = ORIENTED_EDGE ( 'NONE', *, *, #69950, .T. ) ;
#106798 = CONICAL_SURFACE ( 'NONE', #50371, 0.09999999999999982514, 0.003490658503988666988 ) ;
#106799 = VECTOR ( 'NONE', #4232, 1000.000000000000000 ) ;
#106800 = DIRECTION ( 'NONE',  ( -0.000000000000000000, -1.000000000000000000, -0.000000000000000000 ) ) ;
#106801 = ORIENTED_EDGE ( 'NONE', *, *, #5386, .F. ) ;
#106802 = DIRECTION ( 'NONE',  ( -4.274815082592931898E-19, -0.9999939076577903929, -0.003490651415223739937 ) ) ;
#106803 = VECTOR ( 'NONE', #78702, 1000.000000000000000 ) ;
#106804 = ORIENTED_EDGE ( 'NONE', *, *, #12466, .F. ) ;
#106805 = CARTESIAN_POINT ( 'NONE',  ( -13.74999999999998934, 12.50000000000000000, -1.472243186433547901 ) ) ;
#106806 = ORIENTED_EDGE ( 'NONE', *, *, #51906, .T. ) ;
#106807 = ADVANCED_FACE ( 'NONE', ( #97703 ), #54710, .T. ) ;
#106808 = EDGE_LOOP ( 'NONE', ( #87038, #10338, #91415, #88651 ) ) ;
#106809 = DIRECTION ( 'NONE',  ( -0.000000000000000000, -1.000000000000000000, -0.000000000000000000 ) ) ;
#106810 = DIRECTION ( 'NONE',  ( -0.000000000000000000, -1.000000000000000000, -0.000000000000000000 ) ) ;
#106811 = CARTESIAN_POINT ( 'NONE',  ( 0.6499999999999543920, 12.50000000000000000, 6.148780366869520897 ) ) ;
#106812 = DIRECTION ( 'NONE',  ( 0.000000000000000000, 1.000000000000000000, 0.000000000000000000 ) ) ;
#106813 = DIRECTION ( 'NONE',  ( 0.000000000000000000, 1.000000000000000000, 0.000000000000000000 ) ) ;
#106814 = ORIENTED_EDGE ( 'NONE', *, *, #5055, .F. ) ;
#106815 = DIRECTION ( 'NONE',  ( 0.000000000000000000, 1.000000000000000000, 0.000000000000000000 ) ) ;
#106816 = DIRECTION ( 'NONE',  ( 0.000000000000000000, -0.9999939076577903929, 0.003490651415223739937 ) ) ;
#106817 = DIRECTION ( 'NONE',  ( -0.000000000000000000, 1.000000000000000000, -0.000000000000000000 ) ) ;
#106818 = CARTESIAN_POINT ( 'NONE',  ( 11.89999999999990798, 12.50000000000000000, 4.048810130592458201 ) ) ;
#106819 = CARTESIAN_POINT ( 'NONE',  ( 12.89999999999990266, 12.50000000000000000, -3.572213422710612374 ) ) ;
#106820 = ORIENTED_EDGE ( 'NONE', *, *, #80456, .F. ) ;
#106821 = CIRCLE ( 'NONE', #31630, 0.1000000000000002554 ) ;
#106822 = ADVANCED_FACE ( 'NONE', ( #6088 ), #4608, .T. ) ;
#106823 = ORIENTED_EDGE ( 'NONE', *, *, #43422, .F. ) ;
#106824 = DIRECTION ( 'NONE',  ( 0.000000000000000000, 0.000000000000000000, -1.000000000000000000 ) ) ;
#106825 = ORIENTED_EDGE ( 'NONE', *, *, #75285, .F. ) ;
#106826 = CARTESIAN_POINT ( 'NONE',  ( 4.799999999999935874, 2.500000000000000000, 3.983716857408420964 ) ) ;
#106827 = CIRCLE ( 'NONE', #50399, 0.06509327318403745899 ) ;
#106828 = CARTESIAN_POINT ( 'NONE',  ( -11.05000000000000071, 2.500000000000000000, -2.511473670974873951 ) ) ;
#106829 = AXIS2_PLACEMENT_3D ( 'NONE', #28570, #108406, #58677 ) ;
#106830 = VERTEX_POINT ( 'NONE', #81299 ) ;
#106831 = CARTESIAN_POINT ( 'NONE',  ( 186.8333333333333144, 6.668395609140177704, -3.849999999999998312 ) ) ;
#106832 = PLANE ( 'NONE',  #32766 ) ;
#106833 = DIRECTION ( 'NONE',  ( 0.000000000000000000, 1.000000000000000000, 0.000000000000000000 ) ) ;
#106834 = EDGE_CURVE ( 'NONE', #50498, #112645, #23418, .T. ) ;
#106835 = FACE_OUTER_BOUND ( 'NONE', #62620, .T. ) ;
#106836 = CARTESIAN_POINT ( 'NONE',  ( -9.550000000000002487, 12.50000000000000000, 6.495190528383297135 ) ) ;
#106837 = EDGE_LOOP ( 'NONE', ( #15032, #78831, #18042, #99382 ) ) ;
#106838 = VECTOR ( 'NONE', #52555, 1000.000000000000000 ) ;
#106839 = CONICAL_SURFACE ( 'NONE', #85909, 0.1000000000000000472, 0.003490658503988666988 ) ;
#106840 = CARTESIAN_POINT ( 'NONE',  ( 3.749999999999940492, 2.500000000000000000, 5.802370205355744659 ) ) ;
#106841 = LINE ( 'NONE', #107505, #12155 ) ;
#106842 = EDGE_LOOP ( 'NONE', ( #96083, #16361, #42087, #92142 ) ) ;
#106843 = CARTESIAN_POINT ( 'NONE',  ( 13.34999999999990017, 2.500000000000000000, 2.165063509461097713 ) ) ;
#106844 = FACE_OUTER_BOUND ( 'NONE', #64477, .T. ) ;
#106845 = CARTESIAN_POINT ( 'NONE',  ( -5.450000000000019718, 12.50000000000000000, 2.165063509461097713 ) ) ;
#106846 = CIRCLE ( 'NONE', #100594, 0.1000000000000002554 ) ;
#106847 = CIRCLE ( 'NONE', #35859, 0.1000000000000002554 ) ;
#106848 = EDGE_LOOP ( 'NONE', ( #123699, #50285 ) ) ;
#106849 = DIRECTION ( 'NONE',  ( 0.000000000000000000, 1.000000000000000000, 0.000000000000000000 ) ) ;
#106850 = VERTEX_POINT ( 'NONE', #121212 ) ;
#106851 = DIRECTION ( 'NONE',  ( -0.000000000000000000, -1.000000000000000000, -0.000000000000000000 ) ) ;
#106852 = FACE_OUTER_BOUND ( 'NONE', #120645, .T. ) ;
#106853 = AXIS2_PLACEMENT_3D ( 'NONE', #64535, #23981, #105760 ) ;
#106854 = CARTESIAN_POINT ( 'NONE',  ( -0.4500000000000397571, 2.500000000000000000, -6.395190528383301931 ) ) ;
#106855 = EDGE_LOOP ( 'NONE', ( #43138, #23161, #66148, #85310 ) ) ;
#106856 = DIRECTION ( 'NONE',  ( 0.000000000000000000, 0.000000000000000000, 1.000000000000000000 ) ) ;
#106857 = ADVANCED_FACE ( 'NONE', ( #100919 ), #63225, .T. ) ;
#106858 = CARTESIAN_POINT ( 'NONE',  ( -3.950000000000026379, 2.500000000000000000, -1.918653347947326004 ) ) ;
#106859 = CONICAL_SURFACE ( 'NONE', #67048, 0.1000000000000000472, 0.003490658503988666988 ) ;
#106860 = CONICAL_SURFACE ( 'NONE', #92199, 0.09999999999999982514, 0.003490658503988666988 ) ;
#106861 = ORIENTED_EDGE ( 'NONE', *, *, #64482, .T. ) ;
#106862 = FACE_OUTER_BOUND ( 'NONE', #79293, .T. ) ;
#106863 = VERTEX_POINT ( 'NONE', #89182 ) ;
#106864 = DIRECTION ( 'NONE',  ( 0.000000000000000000, -0.000000000000000000, 1.000000000000000000 ) ) ;
#106865 = EDGE_CURVE ( 'NONE', #84166, #99722, #2563, .T. ) ;
#106866 = ORIENTED_EDGE ( 'NONE', *, *, #102342, .T. ) ;
#106867 = CARTESIAN_POINT ( 'NONE',  ( 3.549999999999942979, 2.500000000000000000, 1.818653347947321475 ) ) ;
#106868 = DIRECTION ( 'NONE',  ( 0.000000000000000000, -0.9999939076577903929, 0.003490651415223739937 ) ) ;
#106869 = EDGE_CURVE ( 'NONE', #47559, #104184, #30921, .T. ) ;
#106870 = ORIENTED_EDGE ( 'NONE', *, *, #97547, .T. ) ;
#106871 = ADVANCED_FACE ( 'NONE', ( #112048 ), #88244, .T. ) ;
#106872 = VERTEX_POINT ( 'NONE', #99000 ) ;
#106873 = EDGE_CURVE ( 'NONE', #64820, #15926, #71541, .T. ) ;
#106874 = EDGE_CURVE ( 'NONE', #57584, #76809, #54808, .T. ) ;
#106875 = CARTESIAN_POINT ( 'NONE',  ( 0.1999999999999576006, 2.500000000000000000, -4.776537180435978414 ) ) ;
#106876 = CARTESIAN_POINT ( 'NONE',  ( 8.949999999999919353, 2.500000000000000000, 2.411473670974873862 ) ) ;
#106877 = VERTEX_POINT ( 'NONE', #99652 ) ;
#106878 = CARTESIAN_POINT ( 'NONE',  ( -13.34999999999999076, 12.50000000000000000, -2.792790559304614284 ) ) ;
#106879 = CARTESIAN_POINT ( 'NONE',  ( 8.349999999999919709, 12.50000000000000000, -2.099970236277064473 ) ) ;
#106880 = ADVANCED_FACE ( 'NONE', ( #9976 ), #59032, .T. ) ;
#106881 = DIRECTION ( 'NONE',  ( -0.000000000000000000, -1.000000000000000000, -0.000000000000000000 ) ) ;
#106882 = DIRECTION ( 'NONE',  ( -0.000000000000000000, -1.000000000000000000, -0.000000000000000000 ) ) ;
#106883 = CIRCLE ( 'NONE', #16971, 0.09999999999999982514 ) ;
#106884 = AXIS2_PLACEMENT_3D ( 'NONE', #49359, #129215, #39549 ) ;
#106885 = EDGE_CURVE ( 'NONE', #126604, #96497, #41388, .T. ) ;
#106886 = DIRECTION ( 'NONE',  ( -4.274815082592931898E-19, -0.9999939076577903929, -0.003490651415223739937 ) ) ;
#106887 = CARTESIAN_POINT ( 'NONE',  ( -5.850000000000018296, 12.50000000000000000, 2.922977105672686982 ) ) ;
#106888 = EDGE_CURVE ( 'NONE', #16778, #67980, #8830, .T. ) ;
#106889 = EDGE_CURVE ( 'NONE', #62695, #108184, #104972, .T. ) ;
#106890 = EDGE_CURVE ( 'NONE', #90081, #121723, #15071, .T. ) ;
#106891 = ORIENTED_EDGE ( 'NONE', *, *, #67033, .T. ) ;
#106893 = ORIENTED_EDGE ( 'NONE', *, *, #76024, .F. ) ;
#106892 = AXIS2_PLACEMENT_3D ( 'NONE', #65226, #114336, #123506 ) ;
#106894 = ORIENTED_EDGE ( 'NONE', *, *, #47482, .T. ) ;
#106895 = VERTEX_POINT ( 'NONE', #60389 ) ;
#106896 = FACE_OUTER_BOUND ( 'NONE', #59489, .T. ) ;
#106897 = DIRECTION ( 'NONE',  ( 0.000000000000000000, 0.000000000000000000, 1.000000000000000000 ) ) ;
#106898 = AXIS2_PLACEMENT_3D ( 'NONE', #127253, #99725, #77489 ) ;
#106899 = DIRECTION ( 'NONE',  ( -4.274815082592931898E-19, -0.9999939076577903929, -0.003490651415223739937 ) ) ;
#106900 = ORIENTED_EDGE ( 'NONE', *, *, #19506, .F. ) ;
#106901 = FACE_BOUND ( 'NONE', #3099, .T. ) ;
#106902 = EDGE_CURVE ( 'NONE', #107807, #28723, #84055, .T. ) ;
#106903 = CARTESIAN_POINT ( 'NONE',  ( -8.950000000000009948, 2.500000000000000000, 2.511473670974873507 ) ) ;
#106904 = CARTESIAN_POINT ( 'NONE',  ( -12.69999999999999218, 12.50000000000000000, -0.3464101615137741286 ) ) ;
#106905 = CARTESIAN_POINT ( 'NONE',  ( 3.349999999999943689, 2.500000000000000000, 2.165063509461097713 ) ) ;
#106906 = CARTESIAN_POINT ( 'NONE',  ( -7.100000000000013856, 2.500000000000000000, 5.022947341949748790 ) ) ;
#106907 = LINE ( 'NONE', #97739, #114073 ) ;
#106908 = DIRECTION ( 'NONE',  ( 0.000000000000000000, 0.000000000000000000, -1.000000000000000000 ) ) ;
#106909 = CARTESIAN_POINT ( 'NONE',  ( -1.900000000000034550, 2.500000000000000000, 4.576537180435972019 ) ) ;
#106910 = LINE ( 'NONE', #76182, #44991 ) ;
#106911 = DIRECTION ( 'NONE',  ( 0.000000000000000000, 0.000000000000000000, 1.000000000000000000 ) ) ;
#106912 = CARTESIAN_POINT ( 'NONE',  ( 9.199999999999915801, 2.500000000000000000, -4.330127018922201643 ) ) ;
#106913 = EDGE_LOOP ( 'NONE', ( #17649, #14823, #103484, #18543 ) ) ;
#106914 = ORIENTED_EDGE ( 'NONE', *, *, #87417, .T. ) ;
#106915 = EDGE_LOOP ( 'NONE', ( #79111, #128626 ) ) ;
#106916 = ORIENTED_EDGE ( 'NONE', *, *, #81783, .T. ) ;
#106917 = DIRECTION ( 'NONE',  ( 0.000000000000000000, 0.000000000000000000, 1.000000000000000000 ) ) ;
#106918 = CARTESIAN_POINT ( 'NONE',  ( 2.099999999999947686, 12.50000000000000000, 5.022947341949748790 ) ) ;
#106920 = ORIENTED_EDGE ( 'NONE', *, *, #62297, .F. ) ;
#106919 = ORIENTED_EDGE ( 'NONE', *, *, #97394, .T. ) ;
#106921 = ORIENTED_EDGE ( 'NONE', *, *, #22673, .T. ) ;
#106922 = CARTESIAN_POINT ( 'NONE',  ( -3.749999999999991562, 2.500000000000000000, 6.595190528383296780 ) ) ;
#106923 = AXIS2_PLACEMENT_3D ( 'NONE', #18123, #86867, #96047 ) ;
#106924 = AXIS2_PLACEMENT_3D ( 'NONE', #78822, #29075, #68975 ) ;
#106925 = DIRECTION ( 'NONE',  ( 0.000000000000000000, 0.000000000000000000, 1.000000000000000000 ) ) ;
#106926 = DIRECTION ( 'NONE',  ( -0.000000000000000000, 1.000000000000000000, -0.000000000000000000 ) ) ;
#106927 = FACE_OUTER_BOUND ( 'NONE', #43218, .T. ) ;
#106928 = DIRECTION ( 'NONE',  ( 0.000000000000000000, 0.000000000000000000, -1.000000000000000000 ) ) ;
#106929 = ORIENTED_EDGE ( 'NONE', *, *, #44545, .F. ) ;
#106930 = CIRCLE ( 'NONE', #37987, 0.1000000000000000472 ) ;
#106931 = CIRCLE ( 'NONE', #29581, 0.06509327318403745899 ) ;
#106932 = ORIENTED_EDGE ( 'NONE', *, *, #120504, .F. ) ;
#106933 = EDGE_CURVE ( 'NONE', #50878, #15438, #92472, .T. ) ;
#106934 = ORIENTED_EDGE ( 'NONE', *, *, #111544, .T. ) ;
#106935 = AXIS2_PLACEMENT_3D ( 'NONE', #31821, #61287, #101209 ) ;
#106936 = ORIENTED_EDGE ( 'NONE', *, *, #37558, .F. ) ;
#106937 = EDGE_CURVE ( 'NONE', #110796, #59346, #38103, .T. ) ;
#106938 = LINE ( 'NONE', #17250, #111089 ) ;
#106939 = EDGE_LOOP ( 'NONE', ( #68425, #93868, #75333, #123329 ) ) ;
#106940 = EDGE_LOOP ( 'NONE', ( #106644, #88014 ) ) ;
#106941 = AXIS2_PLACEMENT_3D ( 'NONE', #84801, #124729, #35082 ) ;
#106942 = CARTESIAN_POINT ( 'NONE',  ( -11.25000000000000000, 12.50000000000000000, 2.792790559304612064 ) ) ;
#106943 = EDGE_CURVE ( 'NONE', #82416, #102898, #79857, .T. ) ;
#106944 = AXIS2_PLACEMENT_3D ( 'NONE', #17182, #116696, #66940 ) ;
#106945 = DIRECTION ( 'NONE',  ( 0.000000000000000000, 1.000000000000000000, 0.000000000000000000 ) ) ;
#106946 = DIRECTION ( 'NONE',  ( 0.000000000000000000, -0.9999939076577903929, 0.003490651415223739937 ) ) ;
#106947 = DIRECTION ( 'NONE',  ( 0.000000000000000000, 0.000000000000000000, 1.000000000000000000 ) ) ;
#106948 = CIRCLE ( 'NONE', #19103, 0.1000000000000002554 ) ;
#106949 = DIRECTION ( 'NONE',  ( 0.000000000000000000, 0.000000000000000000, 1.000000000000000000 ) ) ;
#106950 = AXIS2_PLACEMENT_3D ( 'NONE', #110263, #120095, #112202 ) ;
#106951 = ORIENTED_EDGE ( 'NONE', *, *, #52107, .F. ) ;
#106952 = DIRECTION ( 'NONE',  ( -0.000000000000000000, 1.000000000000000000, -0.000000000000000000 ) ) ;
#106953 = VERTEX_POINT ( 'NONE', #90449 ) ;
#106954 = CARTESIAN_POINT ( 'NONE',  ( 0.5999999999999555689, 2.500000000000000000, 4.676537180435972552 ) ) ;
#106955 = ORIENTED_EDGE ( 'NONE', *, *, #109535, .F. ) ;
#106956 = CARTESIAN_POINT ( 'NONE',  ( 4.149999999999938183, 12.50000000000000000, 5.802370205355744659 ) ) ;
#106957 = AXIS2_PLACEMENT_3D ( 'NONE', #118648, #39481, #8675 ) ;
#106958 = AXIS2_PLACEMENT_3D ( 'NONE', #20688, #119515, #29859 ) ;
#106959 = FACE_OUTER_BOUND ( 'NONE', #113766, .T. ) ;
#106960 = ORIENTED_EDGE ( 'NONE', *, *, #87841, .T. ) ;
#106961 = CARTESIAN_POINT ( 'NONE',  ( 13.09999999999990195, 2.500000000000000000, 4.776537180435972196 ) ) ;
#106962 = CARTESIAN_POINT ( 'NONE',  ( 183.9609375001707008, 0.000000000000000000, 7.632341765625000107 ) ) ;
#106963 = ORIENTED_EDGE ( 'NONE', *, *, #120614, .F. ) ;
#106964 = DIRECTION ( 'NONE',  ( -4.274815082592931898E-19, -0.9999939076577903929, -0.003490651415223739937 ) ) ;
#106965 = ORIENTED_EDGE ( 'NONE', *, *, #5565, .T. ) ;
#106966 = ORIENTED_EDGE ( 'NONE', *, *, #13977, .T. ) ;
#106967 = DIRECTION ( 'NONE',  ( -0.000000000000000000, -1.000000000000000000, -0.000000000000000000 ) ) ;
#106968 = DIRECTION ( 'NONE',  ( 0.000000000000000000, 0.000000000000000000, 1.000000000000000000 ) ) ;
#106969 = CARTESIAN_POINT ( 'NONE',  ( 183.8593750003413732, 0.000000000000000000, 7.564683531250000925 ) ) ;
#106970 = CARTESIAN_POINT ( 'NONE',  ( -4.150000000000025224, 12.50000000000000000, 6.430097255199259010 ) ) ;
#106971 = EDGE_CURVE ( 'NONE', #43111, #12708, #61667, .T. ) ;
#106972 = DIRECTION ( 'NONE',  ( -0.000000000000000000, -1.000000000000000000, -0.000000000000000000 ) ) ;
#106973 = LINE ( 'NONE', #17290, #61219 ) ;
#106974 = VECTOR ( 'NONE', #27484, 1000.000000000000000 ) ;
#106975 = AXIS2_PLACEMENT_3D ( 'NONE', #48893, #88798, #50817 ) ;
#106976 = AXIS2_PLACEMENT_3D ( 'NONE', #102937, #25031, #65592 ) ;
#106977 = ORIENTED_EDGE ( 'NONE', *, *, #64937, .F. ) ;
#106978 = DIRECTION ( 'NONE',  ( 0.000000000000000000, 0.000000000000000000, -1.000000000000000000 ) ) ;
#106979 = CONICAL_SURFACE ( 'NONE', #86049, 0.1000000000000002554, 0.003490658503988666988 ) ;
#106980 = CIRCLE ( 'NONE', #29633, 0.06509327318403745899 ) ;
#106981 = EDGE_LOOP ( 'NONE', ( #83191, #91049 ) ) ;
#106983 = EDGE_CURVE ( 'NONE', #69489, #87658, #65271, .T. ) ;
#106982 = CIRCLE ( 'NONE', #12889, 0.1000000000000002554 ) ;
#106984 = CONICAL_SURFACE ( 'NONE', #113260, 0.1000000000000002554, 0.003490658503988666988 ) ;
#106985 = DIRECTION ( 'NONE',  ( 0.000000000000000000, 1.000000000000000000, 0.000000000000000000 ) ) ;
#106986 = LINE ( 'NONE', #127935, #94937 ) ;
#106987 = LINE ( 'NONE', #8148, #50681 ) ;
#106988 = EDGE_CURVE ( 'NONE', #13612, #55568, #22393, .T. ) ;
#106989 = DIRECTION ( 'NONE',  ( -0.000000000000000000, 1.000000000000000000, -0.000000000000000000 ) ) ;
#106990 = CARTESIAN_POINT ( 'NONE',  ( -5.000000000000026645, 2.500000000000000000, -3.637306695894650055 ) ) ;
#106991 = EDGE_LOOP ( 'NONE', ( #39085, #60934, #103883, #44145 ) ) ;
#106992 = AXIS2_PLACEMENT_3D ( 'NONE', #4980, #44932, #88038 ) ;
#106993 = CARTESIAN_POINT ( 'NONE',  ( 12.09999999999990550, 12.50000000000000000, 5.022947341949748790 ) ) ;
#106994 = DIRECTION ( 'NONE',  ( 0.000000000000000000, 1.000000000000000000, 0.000000000000000000 ) ) ;
#106995 = ADVANCED_FACE ( 'NONE', ( #93692 ), #96564, .T. ) ;
#106996 = ORIENTED_EDGE ( 'NONE', *, *, #113838, .F. ) ;
#106997 = CARTESIAN_POINT ( 'NONE',  ( -8.350000000000008527, 12.50000000000000000, 5.737276932171707422 ) ) ;
#106998 = VERTEX_POINT ( 'NONE', #44594 ) ;
#106999 = VERTEX_POINT ( 'NONE', #4008 ) ;
#107000 = DIRECTION ( 'NONE',  ( 0.000000000000000000, 0.000000000000000000, 1.000000000000000000 ) ) ;
#107001 = ORIENTED_EDGE ( 'NONE', *, *, #90672, .F. ) ;
#107002 = CARTESIAN_POINT ( 'NONE',  ( 5.599999999999933031, 2.500000000000000000, -0.4464101615137783252 ) ) ;
#107003 = DIRECTION ( 'NONE',  ( -0.000000000000000000, -1.000000000000000000, -0.000000000000000000 ) ) ;
#107004 = DIRECTION ( 'NONE',  ( 0.000000000000000000, 1.000000000000000000, 0.000000000000000000 ) ) ;
#107005 = AXIS2_PLACEMENT_3D ( 'NONE', #40370, #121475, #119542 ) ;
#107006 = ORIENTED_EDGE ( 'NONE', *, *, #60626, .F. ) ;
#107007 = CIRCLE ( 'NONE', #33864, 0.06509327318403745899 ) ;
#107008 = FACE_BOUND ( 'NONE', #85943, .T. ) ;
#107010 = VERTEX_POINT ( 'NONE', #84516 ) ;
#107009 = CARTESIAN_POINT ( 'NONE',  ( 4.349999999999940137, 2.500000000000000000, -6.841600689897078702 ) ) ;
#107011 = CARTESIAN_POINT ( 'NONE',  ( 8.749999999999921840, 2.500000000000000000, -5.802370205355749988 ) ) ;
#107012 = DIRECTION ( 'NONE',  ( 0.000000000000000000, 0.000000000000000000, 1.000000000000000000 ) ) ;
#107013 = AXIS2_PLACEMENT_3D ( 'NONE', #33946, #100731, #11057 ) ;
#107014 = ORIENTED_EDGE ( 'NONE', *, *, #121051, .F. ) ;
#107015 = AXIS2_PLACEMENT_3D ( 'NONE', #75551, #114204, #35023 ) ;
#107016 = EDGE_CURVE ( 'NONE', #121453, #65156, #82007, .T. ) ;
#107017 = AXIS2_PLACEMENT_3D ( 'NONE', #68355, #75589, #17966 ) ;
#107018 = ORIENTED_EDGE ( 'NONE', *, *, #4546, .T. ) ;
#107019 = VERTEX_POINT ( 'NONE', #12539 ) ;
#107020 = DIRECTION ( 'NONE',  ( 0.000000000000000000, 0.000000000000000000, -1.000000000000000000 ) ) ;
#107021 = DIRECTION ( 'NONE',  ( 0.000000000000000000, 0.000000000000000000, 1.000000000000000000 ) ) ;
#107022 = FACE_OUTER_BOUND ( 'NONE', #10587, .T. ) ;
#107023 = EDGE_CURVE ( 'NONE', #3943, #70330, #2721, .T. ) ;
#107024 = FACE_BOUND ( 'NONE', #121807, .T. ) ;
#107025 = ORIENTED_EDGE ( 'NONE', *, *, #109734, .T. ) ;
#107026 = ADVANCED_FACE ( 'NONE', ( #23023 ), #83239, .T. ) ;
#107027 = DIRECTION ( 'NONE',  ( 0.000000000000000000, 0.000000000000000000, 1.000000000000000000 ) ) ;
#107028 = DIRECTION ( 'NONE',  ( 0.000000000000000000, 1.000000000000000000, 0.000000000000000000 ) ) ;
#107029 = AXIS2_PLACEMENT_3D ( 'NONE', #94298, #116521, #46489 ) ;
#107030 = ORIENTED_EDGE ( 'NONE', *, *, #80811, .T. ) ;
#107031 = AXIS2_PLACEMENT_3D ( 'NONE', #34790, #125084, #63593 ) ;
#107032 = CARTESIAN_POINT ( 'NONE',  ( -11.64999999999999858, 12.50000000000000000, -5.867463478539783672 ) ) ;
#107033 = AXIS2_PLACEMENT_3D ( 'NONE', #108808, #129140, #39471 ) ;
#107034 = AXIS2_PLACEMENT_3D ( 'NONE', #74129, #53834, #95701 ) ;
#107035 = AXIS2_PLACEMENT_3D ( 'NONE', #73433, #31595, #53176 ) ;
#107036 = EDGE_CURVE ( 'NONE', #46960, #37231, #46491, .T. ) ;
#107037 = CARTESIAN_POINT ( 'NONE',  ( -12.89999999999999147, 2.500000000000000000, -0.6928203230275500335 ) ) ;
#107038 = EDGE_CURVE ( 'NONE', #94894, #69453, #98717, .T. ) ;
#107039 = CARTESIAN_POINT ( 'NONE',  ( 186.5312500006828031, 9.429780353434619030E-16, -7.700000000000000178 ) ) ;
#107040 = ADVANCED_FACE ( 'NONE', ( #42687 ), #55058, .T. ) ;
#107041 = PLANE ( 'NONE',  #114036 ) ;
#107042 = AXIS2_PLACEMENT_3D ( 'NONE', #93215, #28173, #34301 ) ;
#107043 = CARTESIAN_POINT ( 'NONE',  ( -3.350000000000028955, 2.500000000000000000, -2.165063509461101710 ) ) ;
#107044 = ADVANCED_FACE ( 'NONE', ( #122512 ), #73587, .T. ) ;
#107045 = ORIENTED_EDGE ( 'NONE', *, *, #55522, .T. ) ;
#107046 = CONICAL_SURFACE ( 'NONE', #38011, 0.09999999999999982514, 0.003490658503988666988 ) ;
#107047 = VERTEX_POINT ( 'NONE', #5295 ) ;
#107048 = ORIENTED_EDGE ( 'NONE', *, *, #12470, .T. ) ;
#107049 = EDGE_LOOP ( 'NONE', ( #110260, #69840 ) ) ;
#107050 = EDGE_LOOP ( 'NONE', ( #84513, #108932 ) ) ;
#107051 = FACE_OUTER_BOUND ( 'NONE', #525, .T. ) ;
#107052 = DIRECTION ( 'NONE',  ( 0.000000000000000000, 1.000000000000000000, 0.000000000000000000 ) ) ;
#107053 = VERTEX_POINT ( 'NONE', #124443 ) ;
#107054 = FACE_BOUND ( 'NONE', #30517, .T. ) ;
#107055 = EDGE_CURVE ( 'NONE', #53009, #31935, #417, .T. ) ;
#107056 = DIRECTION ( 'NONE',  ( 0.000000000000000000, 0.000000000000000000, 1.000000000000000000 ) ) ;
#107057 = CARTESIAN_POINT ( 'NONE',  ( 1.049999999999954525, 2.500000000000000000, -2.411473670974877859 ) ) ;
#107058 = DIRECTION ( 'NONE',  ( 0.000000000000000000, 1.000000000000000000, 0.000000000000000000 ) ) ;
#107059 = CARTESIAN_POINT ( 'NONE',  ( -6.650000000000014566, 12.50000000000000000, 2.099970236277060032 ) ) ;
#107060 = DIRECTION ( 'NONE',  ( -4.274815082592931898E-19, -0.9999939076577903929, -0.003490651415223739937 ) ) ;
#107061 = VERTEX_POINT ( 'NONE', #74698 ) ;
#107062 = DIRECTION ( 'NONE',  ( 0.000000000000000000, 1.000000000000000000, 0.000000000000000000 ) ) ;
#107063 = ORIENTED_EDGE ( 'NONE', *, *, #60921, .T. ) ;
#107064 = ORIENTED_EDGE ( 'NONE', *, *, #67993, .T. ) ;
#107065 = CIRCLE ( 'NONE', #127922, 0.1000000000000002554 ) ;
#107066 = EDGE_LOOP ( 'NONE', ( #66856, #49917 ) ) ;
#107067 = VECTOR ( 'NONE', #105580, 1000.000000000000000 ) ;
#107068 = DIRECTION ( 'NONE',  ( 0.000000000000000000, 1.000000000000000000, 0.000000000000000000 ) ) ;
#107069 = CONICAL_SURFACE ( 'NONE', #81937, 0.1000000000000002554, 0.003490658503988666988 ) ;
#107070 = DIRECTION ( 'NONE',  ( -0.000000000000000000, -1.000000000000000000, -0.000000000000000000 ) ) ;
#107071 = CARTESIAN_POINT ( 'NONE',  ( 0.5999999999999560130, 2.500000000000000000, -3.983716857408426293 ) ) ;
#107072 = ORIENTED_EDGE ( 'NONE', *, *, #77491, .F. ) ;
#107073 = CARTESIAN_POINT ( 'NONE',  ( 10.87377556642454657, 1.500000000000127676, -8.986829606636716150 ) ) ;
#107074 = CARTESIAN_POINT ( 'NONE',  ( -7.900000000000014566, 2.500000000000000000, 0.7928203230275495672 ) ) ;
#107075 = CONICAL_SURFACE ( 'NONE', #86135, 0.09999999999999982514, 0.003490658503988666988 ) ;
#107076 = CIRCLE ( 'NONE', #121660, 0.06509327318403745899 ) ;
#107077 = CARTESIAN_POINT ( 'NONE',  ( 10.84999999999991260, 2.500000000000000000, 5.702370205355745014 ) ) ;
#107078 = CARTESIAN_POINT ( 'NONE',  ( 184.4062500006828316, -8.891194145520236347, -1.633285867636356693E-15 ) ) ;
#107079 = DIRECTION ( 'NONE',  ( 0.000000000000000000, 0.000000000000000000, 1.000000000000000000 ) ) ;
#107080 = DIRECTION ( 'NONE',  ( -0.000000000000000000, 1.000000000000000000, -0.000000000000000000 ) ) ;
#107081 = CIRCLE ( 'NONE', #8786, 0.09999999999999982514 ) ;
#107082 = CIRCLE ( 'NONE', #109229, 0.1000000000000002554 ) ;
#107083 = DIRECTION ( 'NONE',  ( 0.000000000000000000, 0.000000000000000000, 1.000000000000000000 ) ) ;
#107084 = EDGE_LOOP ( 'NONE', ( #93251, #57845, #84783, #32701 ) ) ;
#107085 = DIRECTION ( 'NONE',  ( 0.000000000000000000, 0.000000000000000000, -1.000000000000000000 ) ) ;
#107086 = CIRCLE ( 'NONE', #104928, 0.06509327318403745899 ) ;
#107087 = EDGE_LOOP ( 'NONE', ( #19059, #33662, #61744, #16657 ) ) ;
#107088 = EDGE_CURVE ( 'NONE', #74853, #63445, #31839, .T. ) ;
#107089 = EDGE_LOOP ( 'NONE', ( #103725, #18379, #51209, #15134 ) ) ;
#107090 = CARTESIAN_POINT ( 'NONE',  ( 129.5000000000000000, 1.375000000000000222, 6.000000000000000000 ) ) ;
#107091 = CARTESIAN_POINT ( 'NONE',  ( 4.149999999999939959, 2.500000000000000000, -6.395190528383301931 ) ) ;
#107092 = DIRECTION ( 'NONE',  ( -0.000000000000000000, -1.000000000000000000, -0.000000000000000000 ) ) ;
#107093 = ORIENTED_EDGE ( 'NONE', *, *, #47124, .T. ) ;
#107094 = ORIENTED_EDGE ( 'NONE', *, *, #116966, .T. ) ;
#107096 = ADVANCED_FACE ( 'NONE', ( #24950 ), #25552, .T. ) ;
#107095 = AXIS2_PLACEMENT_3D ( 'NONE', #82887, #25223, #65139 ) ;
#107097 = CARTESIAN_POINT ( 'NONE',  ( 21.23528140090950700, -2.699413673072311948, -2.293764360948876480 ) ) ;
#107098 = CARTESIAN_POINT ( 'NONE',  ( 15.39999999999989200, 2.500000000000000000, 0.6928203230275494784 ) ) ;
#107099 = DIRECTION ( 'NONE',  ( 0.000000000000000000, 0.000000000000000000, -1.000000000000000000 ) ) ;
#107100 = EDGE_LOOP ( 'NONE', ( #98882, #68873 ) ) ;
#107101 = ORIENTED_EDGE ( 'NONE', *, *, #97769, .F. ) ;
#107102 = DIRECTION ( 'NONE',  ( 0.000000000000000000, -0.9999939076577903929, 0.003490651415223739937 ) ) ;
#107104 = VERTEX_POINT ( 'NONE', #64229 ) ;
#107103 = AXIS2_PLACEMENT_3D ( 'NONE', #117434, #127936, #16026 ) ;
#107105 = CARTESIAN_POINT ( 'NONE',  ( 1.649999999999948841, 2.500000000000000000, 6.495190528383297135 ) ) ;
#107106 = CIRCLE ( 'NONE', #73658, 0.09999999999999982514 ) ;
#107107 = FACE_OUTER_BOUND ( 'NONE', #77528, .T. ) ;
#107108 = VERTEX_POINT ( 'NONE', #104776 ) ;
#107109 = FACE_OUTER_BOUND ( 'NONE', #54341, .T. ) ;
#107110 = DIRECTION ( 'NONE',  ( 0.000000000000000000, 0.000000000000000000, -1.000000000000000000 ) ) ;
#107111 = CARTESIAN_POINT ( 'NONE',  ( -10.60000000000000320, 12.50000000000000000, -4.611443907251935315 ) ) ;
#107113 = AXIS2_PLACEMENT_3D ( 'NONE', #80957, #52773, #120870 ) ;
#107112 = DIRECTION ( 'NONE',  ( 0.000000000000000000, 0.000000000000000000, -1.000000000000000000 ) ) ;
#107114 = ORIENTED_EDGE ( 'NONE', *, *, #100743, .F. ) ;
#107115 = AXIS2_PLACEMENT_3D ( 'NONE', #100960, #832, #10625 ) ;
#107116 = DIRECTION ( 'NONE',  ( -0.000000000000000000, -1.000000000000000000, -0.000000000000000000 ) ) ;
#107117 = AXIS2_PLACEMENT_3D ( 'NONE', #127294, #118099, #116161 ) ;
#107118 = CARTESIAN_POINT ( 'NONE',  ( 1.649999999999951505, 2.500000000000000000, 2.757883832488649656 ) ) ;
#107119 = ORIENTED_EDGE ( 'NONE', *, *, #126582, .T. ) ;
#107120 = SHAPE_REPRESENTATION ( 'Magnetic Levitation Sonic Motor Unit', ( #108296 ), #1678 ) ;
#107121 = ORIENTED_EDGE ( 'NONE', *, *, #123015, .F. ) ;
#107122 = CARTESIAN_POINT ( 'NONE',  ( 185.1718750003414016, 9.264065473108010111E-16, -7.564683531250000925 ) ) ;
#107123 = DIRECTION ( 'NONE',  ( 0.000000000000000000, 0.000000000000000000, 1.000000000000000000 ) ) ;
#107124 = CARTESIAN_POINT ( 'NONE',  ( 0.3999999999999563904, 2.500000000000000000, 5.022947341949748790 ) ) ;
#107125 = FACE_OUTER_BOUND ( 'NONE', #104200, .T. ) ;
#107126 = AXIS2_PLACEMENT_3D ( 'NONE', #109946, #20909, #11070 ) ;
#107127 = LINE ( 'NONE', #36494, #76142 ) ;
#107128 = FACE_OUTER_BOUND ( 'NONE', #7667, .T. ) ;
#107129 = CONICAL_SURFACE ( 'NONE', #13123, 0.1000000000000002554, 0.003490658503988666988 ) ;
#107130 = EDGE_CURVE ( 'NONE', #17899, #84933, #21365, .T. ) ;
#107131 = DIRECTION ( 'NONE',  ( 0.000000000000000000, 1.000000000000000000, 0.000000000000000000 ) ) ;
#107132 = CIRCLE ( 'NONE', #50707, 0.06509327318403745899 ) ;
#107133 = CARTESIAN_POINT ( 'NONE',  ( -2.500000000000032419, 2.500000000000000000, -3.637306695894650055 ) ) ;
#107134 = VECTOR ( 'NONE', #32129, 1000.000000000000000 ) ;
#107135 = CIRCLE ( 'NONE', #63322, 0.06509327318403745899 ) ;
#107136 = CARTESIAN_POINT ( 'NONE',  ( 6.849999999999929479, 12.50000000000000000, -1.818653347947326138 ) ) ;
#107137 = AXIS2_PLACEMENT_3D ( 'NONE', #35277, #54887, #64710 ) ;
#107138 = CARTESIAN_POINT ( 'NONE',  ( -6.850000000000017408, 12.50000000000000000, -1.818653347947325916 ) ) ;
#107139 = EDGE_CURVE ( 'NONE', #10760, #83674, #64862, .T. ) ;
#107140 = AXIS2_PLACEMENT_3D ( 'NONE', #110609, #42542, #62175 ) ;
#107141 = VERTEX_POINT ( 'NONE', #62313 ) ;
#107142 = DIRECTION ( 'NONE',  ( 0.000000000000000000, 0.000000000000000000, 1.000000000000000000 ) ) ;
#107143 = EDGE_CURVE ( 'NONE', #55337, #66379, #113402, .T. ) ;
#107144 = CARTESIAN_POINT ( 'NONE',  ( 1.449999999999951772, 12.50000000000000000, -6.148780366869526226 ) ) ;
#107145 = ADVANCED_FACE ( 'NONE', ( #56969 ), #119750, .T. ) ;
#107146 = CARTESIAN_POINT ( 'NONE',  ( 14.19999999999989626, 2.500000000000000000, 0.09999999999999772959 ) ) ;
#107147 = CARTESIAN_POINT ( 'NONE',  ( -10.60000000000000320, 2.500000000000000000, -3.983716857408421852 ) ) ;
#107148 = EDGE_LOOP ( 'NONE', ( #10782, #81691, #87825, #30075 ) ) ;
#107149 = CARTESIAN_POINT ( 'NONE',  ( -10.20000000000000462, 12.50000000000000000, -4.676537180435973440 ) ) ;
#107150 = EDGE_CURVE ( 'NONE', #98294, #106877, #77904, .T. ) ;
#107151 = CARTESIAN_POINT ( 'NONE',  ( 185.4166666666666856, 6.668395609140176816, 3.850000000000000977 ) ) ;
#107153 = ORIENTED_EDGE ( 'NONE', *, *, #103650, .F. ) ;
#107152 = DIRECTION ( 'NONE',  ( 0.000000000000000000, 0.000000000000000000, 1.000000000000000000 ) ) ;
#107154 = CIRCLE ( 'NONE', #19324, 0.1000000000000000056 ) ;
#107155 = EDGE_CURVE ( 'NONE', #118854, #93025, #42403, .T. ) ;
#107156 = ORIENTED_EDGE ( 'NONE', *, *, #28, .F. ) ;
#107157 = VERTEX_POINT ( 'NONE', #96250 ) ;
#107158 = EDGE_LOOP ( 'NONE', ( #81229, #55994, #111199, #41842 ) ) ;
#107159 = AXIS2_PLACEMENT_3D ( 'NONE', #57963, #27843, #97870 ) ;
#107160 = ORIENTED_EDGE ( 'NONE', *, *, #60831, .T. ) ;
#107161 = DIRECTION ( 'NONE',  ( -0.000000000000000000, -1.000000000000000000, -0.000000000000000000 ) ) ;
#107162 = CIRCLE ( 'NONE', #11017, 0.09999999999999999167 ) ;
#107163 = CIRCLE ( 'NONE', #67427, 0.1000000000000002554 ) ;
#107164 = DIRECTION ( 'NONE',  ( 0.000000000000000000, 1.000000000000000000, 0.000000000000000000 ) ) ;
#107165 = CARTESIAN_POINT ( 'NONE',  ( -10.00000000000000533, 2.500000000000000000, -4.922947341949749145 ) ) ;
#107166 = DIRECTION ( 'NONE',  ( 0.000000000000000000, 0.000000000000000000, 1.000000000000000000 ) ) ;
#107168 = ORIENTED_EDGE ( 'NONE', *, *, #97858, .F. ) ;
#107167 = CONICAL_SURFACE ( 'NONE', #82040, 0.1000000000000002554, 0.003490658503988666988 ) ;
#107169 = CIRCLE ( 'NONE', #34027, 0.09999999999999982514 ) ;
#107170 = AXIS2_PLACEMENT_3D ( 'NONE', #93957, #23262, #82862 ) ;
#107171 = CARTESIAN_POINT ( 'NONE',  ( 7.299999999999926104, 12.50000000000000000, -3.983716857408426293 ) ) ;
#107173 = ORIENTED_EDGE ( 'NONE', *, *, #77024, .F. ) ;
#107172 = AXIS2_PLACEMENT_3D ( 'NONE', #126909, #67299, #62988 ) ;
#107174 = CARTESIAN_POINT ( 'NONE',  ( 76.45227062060567391, -3.905198618290971257, -5.870121734780581413 ) ) ;
#107175 = FACE_OUTER_BOUND ( 'NONE', #99109, .T. ) ;
#107176 = CONICAL_SURFACE ( 'NONE', #88383, 0.09999999999999982514, 0.003490658503988666988 ) ;
#107178 = CIRCLE ( 'NONE', #11027, 0.09999999999999982514 ) ;
#107177 = DIRECTION ( 'NONE',  ( -0.000000000000000000, -1.000000000000000000, -0.000000000000000000 ) ) ;
#107179 = FACE_OUTER_BOUND ( 'NONE', #73489, .T. ) ;
#107180 = CARTESIAN_POINT ( 'NONE',  ( -11.04999999999999893, 12.50000000000000000, 6.148780366869520009 ) ) ;
#107181 = CONICAL_SURFACE ( 'NONE', #50766, 0.09999999999999982514, 0.003490658503988666988 ) ;
#107182 = ORIENTED_EDGE ( 'NONE', *, *, #82734, .F. ) ;
#107183 = ADVANCED_FACE ( 'NONE', ( #106718 ), #103019, .T. ) ;
#107184 = ORIENTED_EDGE ( 'NONE', *, *, #64751, .T. ) ;
#107185 = ORIENTED_EDGE ( 'NONE', *, *, #16553, .T. ) ;
#107186 = ORIENTED_EDGE ( 'NONE', *, *, #125920, .F. ) ;
#107187 = CARTESIAN_POINT ( 'NONE',  ( -3.642919299551294898E-14, 12.50000000000000000, 0.6928203230275518099 ) ) ;
#107188 = DIRECTION ( 'NONE',  ( 0.000000000000000000, 0.000000000000000000, 1.000000000000000000 ) ) ;
#107189 = CARTESIAN_POINT ( 'NONE',  ( -12.09999999999999609, 2.500000000000000000, -4.330127018922198978 ) ) ;
#107190 = ADVANCED_FACE ( 'NONE', ( #97551 ), #23608, .T. ) ;
#107191 = FACE_BOUND ( 'NONE', #123021, .T. ) ;
#107192 = CARTESIAN_POINT ( 'NONE',  ( -14.34999999999998543, 2.500000000000000000, 2.411473670974877415 ) ) ;
#107193 = CARTESIAN_POINT ( 'NONE',  ( -12.04999999999999538, 12.50000000000000000, 2.099970236277060032 ) ) ;
#107194 = ADVANCED_FACE ( 'NONE', ( #15759 ), #27711, .T. ) ;
#107195 = DIRECTION ( 'NONE',  ( -0.000000000000000000, 1.000000000000000000, -0.000000000000000000 ) ) ;
#107196 = CARTESIAN_POINT ( 'NONE',  ( -2.700000000000030820, 12.50000000000000000, 0.3464101615137735735 ) ) ;
#107197 = CIRCLE ( 'NONE', #84205, 0.06509327318403743123 ) ;
#107198 = EDGE_CURVE ( 'NONE', #92191, #60850, #31937, .T. ) ;
#107199 = CARTESIAN_POINT ( 'NONE',  ( 184.4635416670080588, -4.367472073101520635, 7.564683531249999149 ) ) ;
#107200 = DIRECTION ( 'NONE',  ( 1.000000000000000000, -0.000000000000000000, -0.000000000000000000 ) ) ;
#107201 = EDGE_CURVE ( 'NONE', #39846, #44247, #106092, .T. ) ;
#107202 = DIRECTION ( 'NONE',  ( 0.000000000000000000, -0.9999939076577903929, 0.003490651415223739937 ) ) ;
#107203 = ADVANCED_FACE ( 'NONE', ( #86438 ), #36064, .T. ) ;
#107204 = AXIS2_PLACEMENT_3D ( 'NONE', #74817, #55178, #6055 ) ;
#107205 = AXIS2_PLACEMENT_3D ( 'NONE', #29159, #67770, #18672 ) ;
#107206 = CIRCLE ( 'NONE', #123926, 0.1000000000000000472 ) ;
#107207 = CARTESIAN_POINT ( 'NONE',  ( -10.40000000000000213, 2.500000000000000000, -4.430127018922197735 ) ) ;
#107208 = EDGE_CURVE ( 'NONE', #35207, #78590, #117822, .T. ) ;
#107209 = ORIENTED_EDGE ( 'NONE', *, *, #69574, .T. ) ;
#107210 = VERTEX_POINT ( 'NONE', #105452 ) ;
#107211 = ORIENTED_EDGE ( 'NONE', *, *, #487, .T. ) ;
#107212 = ORIENTED_EDGE ( 'NONE', *, *, #108359, .T. ) ;
#107213 = CARTESIAN_POINT ( 'NONE',  ( 13.09999999999990195, 12.50000000000000000, 4.676537180435972552 ) ) ;
#107214 = FACE_BOUND ( 'NONE', #85486, .T. ) ;
#107215 = VECTOR ( 'NONE', #77888, 1000.000000000000000 ) ;
#107216 = DIRECTION ( 'NONE',  ( 0.000000000000000000, 1.000000000000000000, 0.000000000000000000 ) ) ;
#107217 = CIRCLE ( 'NONE', #128159, 0.09999999999999982514 ) ;
#107218 = EDGE_CURVE ( 'NONE', #117937, #10213, #88335, .T. ) ;
#107219 = LINE ( 'NONE', #86930, #41454 ) ;
#107220 = CIRCLE ( 'NONE', #75916, 0.06509327318403745899 ) ;
#107221 = ADVANCED_FACE ( 'NONE', ( #27503 ), #67417, .T. ) ;
#107222 = ORIENTED_EDGE ( 'NONE', *, *, #3600, .T. ) ;
#107223 = DIRECTION ( 'NONE',  ( 0.000000000000000000, 1.000000000000000000, 0.000000000000000000 ) ) ;
#107224 = CARTESIAN_POINT ( 'NONE',  ( -5.000000000000024869, 2.500000000000000000, -5.122947341949753763 ) ) ;
#107225 = FACE_OUTER_BOUND ( 'NONE', #75304, .T. ) ;
#107226 = VERTEX_POINT ( 'NONE', #36720 ) ;
#107227 = LINE ( 'NONE', #98052, #53369 ) ;
#107228 = DIRECTION ( 'NONE',  ( 0.000000000000000000, 1.000000000000000000, 0.000000000000000000 ) ) ;
#107229 = CIRCLE ( 'NONE', #48560, 0.1000000000000002554 ) ;
#107230 = CIRCLE ( 'NONE', #94710, 0.06509327318403745899 ) ;
#107231 = AXIS2_PLACEMENT_3D ( 'NONE', #98107, #18262, #7136 ) ;
#107232 = CIRCLE ( 'NONE', #65460, 0.06509327318403745899 ) ;
#107233 = ORIENTED_EDGE ( 'NONE', *, *, #79081, .T. ) ;
#107234 = CARTESIAN_POINT ( 'NONE',  ( -6.050000000000022027, 12.50000000000000000, -1.883746621131363597 ) ) ;
#107235 = DIRECTION ( 'NONE',  ( 0.000000000000000000, 0.000000000000000000, -1.000000000000000000 ) ) ;
#107236 = VECTOR ( 'NONE', #61349, 1000.000000000000000 ) ;
#107237 = ORIENTED_EDGE ( 'NONE', *, *, #56687, .F. ) ;
#107238 = DIRECTION ( 'NONE',  ( 0.000000000000000000, -0.000000000000000000, 1.000000000000000000 ) ) ;
#107239 = AXIS2_PLACEMENT_3D ( 'NONE', #486, #11610, #51557 ) ;
#107240 = CARTESIAN_POINT ( 'NONE',  ( 8.749999999999953815, 12.50000000000000000, 6.430097255199259010 ) ) ;
#107241 = CARTESIAN_POINT ( 'NONE',  ( 7.499999999999925393, 2.500000000000000000, -3.637306695894650055 ) ) ;
#107242 = EDGE_LOOP ( 'NONE', ( #23086, #85488 ) ) ;
#107243 = EDGE_LOOP ( 'NONE', ( #101472, #11045 ) ) ;
#107244 = ADVANCED_FACE ( 'NONE', ( #108015 ), #33987, .T. ) ;
#107245 = CARTESIAN_POINT ( 'NONE',  ( -3.950000000000026379, 12.50000000000000000, -1.818653347947326138 ) ) ;
#107246 = ORIENTED_EDGE ( 'NONE', *, *, #101408, .F. ) ;
#107247 = DIRECTION ( 'NONE',  ( -0.000000000000000000, -1.000000000000000000, -0.000000000000000000 ) ) ;
#107248 = FACE_BOUND ( 'NONE', #31885, .T. ) ;
#107249 = ORIENTED_EDGE ( 'NONE', *, *, #20665, .T. ) ;
#107250 = EDGE_CURVE ( 'NONE', #38503, #68589, #28180, .T. ) ;
#107251 = CARTESIAN_POINT ( 'NONE',  ( 129.5000000000000000, 0.000000000000000000, 0.000000000000000000 ) ) ;
#107252 = VERTEX_POINT ( 'NONE', #95629 ) ;
#107253 = DIRECTION ( 'NONE',  ( 0.000000000000000000, -0.9999939076577903929, 0.003490651415223739937 ) ) ;
#107254 = FACE_OUTER_BOUND ( 'NONE', #84770, .T. ) ;
#107255 = AXIS2_PLACEMENT_3D ( 'NONE', #2621, #22934, #123678 ) ;
#107256 = CARTESIAN_POINT ( 'NONE',  ( 7.499999999999927169, 2.500000000000000000, 3.737306695894644371 ) ) ;
#107257 = DIRECTION ( 'NONE',  ( -0.000000000000000000, 1.000000000000000000, -0.000000000000000000 ) ) ;
#107258 = CARTESIAN_POINT ( 'NONE',  ( 179.5000000000000000, -1.375000000000002442, -6.000000000000000000 ) ) ;
#107259 = ORIENTED_EDGE ( 'NONE', *, *, #120914, .F. ) ;
#107260 = ADVANCED_FACE ( 'NONE', ( #76635 ), #107129, .T. ) ;
#107261 = ORIENTED_EDGE ( 'NONE', *, *, #108968, .T. ) ;
#107262 = CARTESIAN_POINT ( 'NONE',  ( 10.39999999999991509, 2.500000000000000000, -0.5928203230275542746 ) ) ;
#107263 = AXIS2_PLACEMENT_3D ( 'NONE', #85441, #33762, #84798 ) ;
#107264 = CARTESIAN_POINT ( 'NONE',  ( -13.34999999999999076, 2.500000000000000000, -2.757883832488651876 ) ) ;
#107266 = CARTESIAN_POINT ( 'NONE',  ( -6.050000000000022027, 2.500000000000000000, -1.818653347947326138 ) ) ;
#107265 = CIRCLE ( 'NONE', #128210, 0.06509327318403741736 ) ;
#107268 = ORIENTED_EDGE ( 'NONE', *, *, #33484, .T. ) ;
#107267 = VERTEX_POINT ( 'NONE', #25576 ) ;
#107269 = ORIENTED_EDGE ( 'NONE', *, *, #83289, .T. ) ;
#107270 = CARTESIAN_POINT ( 'NONE',  ( -1.450000000000035927, 12.50000000000000000, -6.083687093685488989 ) ) ;
#107271 = CARTESIAN_POINT ( 'NONE',  ( -11.24999999999999822, 12.50000000000000000, 5.802370205355744659 ) ) ;
#107272 = VECTOR ( 'NONE', #108586, 1000.000000000000000 ) ;
#107274 = DIRECTION ( 'NONE',  ( 0.000000000000000000, 0.000000000000000000, 1.000000000000000000 ) ) ;
#107273 = VECTOR ( 'NONE', #116965, 1000.000000000000000 ) ;
#107275 = AXIS2_PLACEMENT_3D ( 'NONE', #99120, #19916, #9446 ) ;
#107276 = DIRECTION ( 'NONE',  ( 0.000000000000000000, 1.000000000000000000, 0.000000000000000000 ) ) ;
#107277 = FACE_OUTER_BOUND ( 'NONE', #109668, .T. ) ;
#107278 = FACE_OUTER_BOUND ( 'NONE', #4774, .T. ) ;
#107279 = DIRECTION ( 'NONE',  ( -0.000000000000000000, 1.000000000000000000, -0.000000000000000000 ) ) ;
#107280 = LINE ( 'NONE', #96805, #124070 ) ;
#107281 = FACE_OUTER_BOUND ( 'NONE', #54884, .T. ) ;
#107282 = AXIS2_PLACEMENT_3D ( 'NONE', #96345, #66248, #65609 ) ;
#107283 = ORIENTED_EDGE ( 'NONE', *, *, #63595, .T. ) ;
#107284 = VERTEX_POINT ( 'NONE', #45888 ) ;
#107285 = CARTESIAN_POINT ( 'NONE',  ( 0.8499999999999527933, 2.500000000000000000, 7.088010851410848190 ) ) ;
#107286 = EDGE_LOOP ( 'NONE', ( #67965, #96684 ) ) ;
#107287 = ORIENTED_EDGE ( 'NONE', *, *, #24430, .T. ) ;
#107288 = DIRECTION ( 'NONE',  ( 0.000000000000000000, -0.000000000000000000, 1.000000000000000000 ) ) ;
#107289 = DIRECTION ( 'NONE',  ( -0.000000000000000000, 1.000000000000000000, -0.000000000000000000 ) ) ;
#107290 = LINE ( 'NONE', #116459, #109223 ) ;
#107291 = AXIS2_PLACEMENT_3D ( 'NONE', #106232, #37503, #76773 ) ;
#107292 = DIRECTION ( 'NONE',  ( 0.000000000000000000, 1.000000000000000000, 0.000000000000000000 ) ) ;
#107293 = CARTESIAN_POINT ( 'NONE',  ( -11.64999999999999680, 2.500000000000000000, 1.372243186433545370 ) ) ;
#107294 = CARTESIAN_POINT ( 'NONE',  ( -12.49999999999999289, 12.50000000000000000, 3.637306695894644726 ) ) ;
#107295 = DIRECTION ( 'NONE',  ( -4.274815082592931898E-19, -0.9999939076577903929, -0.003490651415223739937 ) ) ;
#107296 = EDGE_LOOP ( 'NONE', ( #88813, #57181 ) ) ;
#107297 = CARTESIAN_POINT ( 'NONE',  ( -1.450000000000035927, 12.50000000000000000, -6.148780366869526226 ) ) ;
#107298 = CIRCLE ( 'NONE', #67574, 0.06509327318403745899 ) ;
#107300 = CIRCLE ( 'NONE', #21631, 0.06509327318403745899 ) ;
#107299 = CARTESIAN_POINT ( 'NONE',  ( -6.505213034913026604E-15, 12.50000000000000000, 4.330127018922196314 ) ) ;
#107301 = ADVANCED_FACE ( 'NONE', ( #85793 ), #125705, .T. ) ;
#107302 = CONICAL_SURFACE ( 'NONE', #11151, 0.1000000000000002554, 0.003490658503988666988 ) ;
#107303 = EDGE_LOOP ( 'NONE', ( #18930, #55124, #62331, #127204 ) ) ;
#107304 = VERTEX_POINT ( 'NONE', #51056 ) ;
#107305 = ADVANCED_FACE ( 'NONE', ( #81153, #41238 ), #50388, .T. ) ;
#107306 = VERTEX_POINT ( 'NONE', #78587 ) ;
#107307 = EDGE_LOOP ( 'NONE', ( #4033, #25203 ) ) ;
#107308 = EDGE_CURVE ( 'NONE', #109714, #127460, #98817, .T. ) ;
#107309 = PLANE ( 'NONE',  #8620 ) ;
#107310 = DIRECTION ( 'NONE',  ( 0.000000000000000000, -0.9999939076577903929, 0.003490651415223739937 ) ) ;
#107311 = CONICAL_SURFACE ( 'NONE', #71818, 0.1000000000000002554, 0.003490658503988666988 ) ;
#107312 = AXIS2_PLACEMENT_3D ( 'NONE', #114332, #62195, #5013 ) ;
#107313 = ORIENTED_EDGE ( 'NONE', *, *, #86080, .F. ) ;
#107314 = CARTESIAN_POINT ( 'NONE',  ( -14.59999999999998366, 2.500000000000000000, -0.7928203230275520097 ) ) ;
#107315 = CIRCLE ( 'NONE', #50889, 0.1000000000000000472 ) ;
#107316 = CARTESIAN_POINT ( 'NONE',  ( 9.349999999999916156, 2.500000000000000000, -2.411473670974877859 ) ) ;
#107317 = ADVANCED_FACE ( 'NONE', ( #11092 ), #50704, .T. ) ;
#107318 = DIRECTION ( 'NONE',  ( 0.000000000000000000, 0.000000000000000000, 1.000000000000000000 ) ) ;
#107320 = ORIENTED_EDGE ( 'NONE', *, *, #49406, .F. ) ;
#107319 = EDGE_CURVE ( 'NONE', #99172, #21324, #1287, .T. ) ;
#107321 = ADVANCED_FACE ( 'NONE', ( #118477 ), #40251, .T. ) ;
#107322 = CARTESIAN_POINT ( 'NONE',  ( -3.950000000000026379, 12.50000000000000000, 6.841600689897072485 ) ) ;
#107323 = VECTOR ( 'NONE', #49147, 1000.000000000000000 ) ;
#107324 = FACE_OUTER_BOUND ( 'NONE', #108220, .T. ) ;
#107325 = ORIENTED_EDGE ( 'NONE', *, *, #17486, .F. ) ;
#107326 = CIRCLE ( 'NONE', #59231, 0.06509327318403745899 ) ;
#107327 = VECTOR ( 'NONE', #96619, 1000.000000000000000 ) ;
#107328 = ORIENTED_EDGE ( 'NONE', *, *, #30641, .F. ) ;
#107329 = ORIENTED_EDGE ( 'NONE', *, *, #122704, .F. ) ;
#107330 = FACE_OUTER_BOUND ( 'NONE', #13687, .T. ) ;
#107331 = AXIS2_PLACEMENT_3D ( 'NONE', #73568, #91292, #113505 ) ;
#107332 = DIRECTION ( 'NONE',  ( 0.000000000000000000, 1.000000000000000000, 0.000000000000000000 ) ) ;
#107333 = ORIENTED_EDGE ( 'NONE', *, *, #102393, .T. ) ;
#107334 = DIRECTION ( 'NONE',  ( 0.000000000000000000, 0.000000000000000000, 1.000000000000000000 ) ) ;
#107335 = DIRECTION ( 'NONE',  ( -0.000000000000000000, 1.000000000000000000, -0.000000000000000000 ) ) ;
#107336 = DIRECTION ( 'NONE',  ( 0.000000000000000000, 0.000000000000000000, 1.000000000000000000 ) ) ;
#107337 = DIRECTION ( 'NONE',  ( -0.000000000000000000, 1.000000000000000000, -0.000000000000000000 ) ) ;
#107338 = ORIENTED_EDGE ( 'NONE', *, *, #119874, .F. ) ;
#107339 = DIRECTION ( 'NONE',  ( 0.000000000000000000, 0.000000000000000000, -1.000000000000000000 ) ) ;
#107340 = ORIENTED_EDGE ( 'NONE', *, *, #72377, .F. ) ;
#107341 = ORIENTED_EDGE ( 'NONE', *, *, #31751, .F. ) ;
#107343 = CIRCLE ( 'NONE', #119872, 0.1000000000000002554 ) ;
#107342 = CARTESIAN_POINT ( 'NONE',  ( 0.5999999999999551248, 12.50000000000000000, -4.676537180435978769 ) ) ;
#107344 = CIRCLE ( 'NONE', #30003, 0.1000000000000000472 ) ;
#107345 = CARTESIAN_POINT ( 'NONE',  ( -7.900000000000014566, 2.500000000000000000, -2.276824562219559311E-15 ) ) ;
#107346 = FACE_BOUND ( 'NONE', #86659, .T. ) ;
#107347 = CARTESIAN_POINT ( 'NONE',  ( 186.2395833340161175, 4.445597072760147483, 7.699999999999948663 ) ) ;
#107348 = DIRECTION ( 'NONE',  ( 0.000000000000000000, -0.9999939076577903929, 0.003490651415223739937 ) ) ;
#107349 = DIRECTION ( 'NONE',  ( 0.000000000000000000, 0.000000000000000000, -1.000000000000000000 ) ) ;
#107350 = AXIS2_PLACEMENT_3D ( 'NONE', #83987, #102992, #55198 ) ;
#107351 = AXIS2_PLACEMENT_3D ( 'NONE', #66562, #77672, #78348 ) ;
#107352 = AXIS2_PLACEMENT_3D ( 'NONE', #37726, #68457, #27901 ) ;
#107354 = ADVANCED_FACE ( 'NONE', ( #90295 ), #2659, .T. ) ;
#107353 = AXIS2_PLACEMENT_3D ( 'NONE', #40185, #127913, #89914 ) ;
#107355 = ORIENTED_EDGE ( 'NONE', *, *, #13929, .T. ) ;
#107356 = EDGE_CURVE ( 'NONE', #32515, #89688, #86284, .T. ) ;
#107357 = DIRECTION ( 'NONE',  ( 0.000000000000000000, 1.000000000000000000, 0.000000000000000000 ) ) ;
#107358 = LINE ( 'NONE', #27485, #82456 ) ;
#107359 = CARTESIAN_POINT ( 'NONE',  ( 9.149999999999915090, 2.500000000000000000, -2.065063509461102065 ) ) ;
#107360 = ADVANCED_FACE ( 'NONE', ( #49123 ), #67395, .T. ) ;
#107361 = FACE_OUTER_BOUND ( 'NONE', #19511, .T. ) ;
#107362 = EDGE_LOOP ( 'NONE', ( #111213, #8012, #56768, #83350 ) ) ;
#107363 = FACE_OUTER_BOUND ( 'NONE', #105086, .T. ) ;
#107364 = VECTOR ( 'NONE', #13233, 1000.000000000000000 ) ;
#107365 = AXIS2_PLACEMENT_3D ( 'NONE', #51373, #41553, #91277 ) ;
#107366 = CARTESIAN_POINT ( 'NONE',  ( 6.649999999999930189, 2.500000000000000000, -1.472243186433550122 ) ) ;
#107367 = EDGE_CURVE ( 'NONE', #65580, #16616, #23509, .T. ) ;
#107368 = EDGE_CURVE ( 'NONE', #2989, #54526, #96658, .T. ) ;
#107369 = ORIENTED_EDGE ( 'NONE', *, *, #104165, .F. ) ;
#107370 = AXIS2_PLACEMENT_3D ( 'NONE', #14391, #105371, #15678 ) ;
#107371 = DIRECTION ( 'NONE',  ( 0.000000000000000000, 0.000000000000000000, 1.000000000000000000 ) ) ;
#107372 = DIRECTION ( 'NONE',  ( -4.274815082592931898E-19, -0.9999939076577903929, -0.003490651415223739937 ) ) ;
#107373 = FACE_BOUND ( 'NONE', #81154, .T. ) ;
#107374 = CARTESIAN_POINT ( 'NONE',  ( 8.328334240990686865, -2.500000000000000000, -8.539519492767929876 ) ) ;
#107375 = EDGE_CURVE ( 'NONE', #8229, #112688, #69378, .T. ) ;
#107376 = EDGE_CURVE ( 'NONE', #125682, #44204, #4710, .T. ) ;
#107377 = ORIENTED_EDGE ( 'NONE', *, *, #19684, .F. ) ;
#107378 = DIRECTION ( 'NONE',  ( -0.000000000000000000, -1.000000000000000000, -0.000000000000000000 ) ) ;
#107379 = EDGE_LOOP ( 'NONE', ( #37846, #114184 ) ) ;
#107380 = ORIENTED_EDGE ( 'NONE', *, *, #35577, .T. ) ;
#107381 = CARTESIAN_POINT ( 'NONE',  ( 20.37757664703743998, 0.6627606010239225354, -4.188167776336756631 ) ) ;
#107382 = CARTESIAN_POINT ( 'NONE',  ( 185.9166666666666856, 6.668395609140176816, 3.850000000000000977 ) ) ;
#107383 = ADVANCED_FACE ( 'NONE', ( #30129 ), #21461, .T. ) ;
#107385 = ORIENTED_EDGE ( 'NONE', *, *, #50647, .T. ) ;
#107384 = AXIS2_PLACEMENT_3D ( 'NONE', #74037, #44579, #51828 ) ;
#107386 = DIRECTION ( 'NONE',  ( 0.000000000000000000, -0.9999939076577903929, 0.003490651415223739937 ) ) ;
#107387 = DIRECTION ( 'NONE',  ( 0.000000000000000000, 1.000000000000000000, 0.000000000000000000 ) ) ;
#107388 = CARTESIAN_POINT ( 'NONE',  ( 4.349999999999936584, 12.50000000000000000, 6.148780366869520009 ) ) ;
#107389 = AXIS2_PLACEMENT_3D ( 'NONE', #66602, #27973, #68534 ) ;
#107390 = CIRCLE ( 'NONE', #98988, 0.06509327318403745899 ) ;
#107391 = CIRCLE ( 'NONE', #117747, 0.1000000000000002554 ) ;
#107392 = ORIENTED_EDGE ( 'NONE', *, *, #20915, .T. ) ;
#107393 = DIRECTION ( 'NONE',  ( 0.000000000000000000, 0.000000000000000000, 1.000000000000000000 ) ) ;
#107394 = CARTESIAN_POINT ( 'NONE',  ( -8.350000000000010303, 12.50000000000000000, 6.495190528383297135 ) ) ;
#107395 = CARTESIAN_POINT ( 'NONE',  ( -11.44999999999999929, 2.500000000000000000, -1.818653347947322141 ) ) ;
#107396 = DIRECTION ( 'NONE',  ( -0.000000000000000000, 1.000000000000000000, -0.000000000000000000 ) ) ;
#107397 = ORIENTED_EDGE ( 'NONE', *, *, #14507, .F. ) ;
#107398 = DIRECTION ( 'NONE',  ( 0.000000000000000000, 1.000000000000000000, 0.000000000000000000 ) ) ;
#107399 = ORIENTED_EDGE ( 'NONE', *, *, #80923, .F. ) ;
#107400 = AXIS2_PLACEMENT_3D ( 'NONE', #79056, #9654, #109120 ) ;
#107401 = DIRECTION ( 'NONE',  ( -4.274815082592931898E-19, -0.9999939076577903929, -0.003490651415223739937 ) ) ;
#107402 = AXIS2_PLACEMENT_3D ( 'NONE', #24552, #75576, #103765 ) ;
#107403 = ORIENTED_EDGE ( 'NONE', *, *, #22655, .T. ) ;
#107405 = FACE_OUTER_BOUND ( 'NONE', #27822, .T. ) ;
#107404 = CONICAL_SURFACE ( 'NONE', #82718, 0.09999999999999982514, 0.003490658503988666988 ) ;
#107406 = LINE ( 'NONE', #25611, #45281 ) ;
#107407 = VECTOR ( 'NONE', #121484, 1000.000000000000000 ) ;
#107408 = DIRECTION ( 'NONE',  ( -0.000000000000000000, 1.000000000000000000, -0.000000000000000000 ) ) ;
#107409 = CARTESIAN_POINT ( 'NONE',  ( 10.59999999999991260, 12.50000000000000000, -0.4115034346978157509 ) ) ;
#107410 = ORIENTED_EDGE ( 'NONE', *, *, #91362, .F. ) ;
#107411 = DIRECTION ( 'NONE',  ( -0.000000000000000000, -1.000000000000000000, -0.000000000000000000 ) ) ;
#107412 = DIRECTION ( 'NONE',  ( 0.000000000000000000, 0.000000000000000000, 1.000000000000000000 ) ) ;
#107413 = FACE_OUTER_BOUND ( 'NONE', #127661, .T. ) ;
#107414 = DIRECTION ( 'NONE',  ( 0.000000000000000000, 0.000000000000000000, 1.000000000000000000 ) ) ;
#107415 = CARTESIAN_POINT ( 'NONE',  ( 14.14999999999989555, 12.50000000000000000, 2.165063509461097713 ) ) ;
#107416 = ORIENTED_EDGE ( 'NONE', *, *, #36335, .T. ) ;
#107417 = ADVANCED_FACE ( 'NONE', ( #110597 ), #71634, .T. ) ;
#107418 = ORIENTED_EDGE ( 'NONE', *, *, #102843, .F. ) ;
#107419 = DIRECTION ( 'NONE',  ( 0.000000000000000000, 0.000000000000000000, 1.000000000000000000 ) ) ;
#107421 = ORIENTED_EDGE ( 'NONE', *, *, #92829, .F. ) ;
#107420 = AXIS2_PLACEMENT_3D ( 'NONE', #76779, #74200, #34934 ) ;
#107422 = CONICAL_SURFACE ( 'NONE', #92762, 0.1000000000000002554, 0.003490658503988666988 ) ;
#107423 = DIRECTION ( 'NONE',  ( -0.000000000000000000, 1.000000000000000000, -0.000000000000000000 ) ) ;
#107425 = ORIENTED_EDGE ( 'NONE', *, *, #47822, .F. ) ;
#107424 = VERTEX_POINT ( 'NONE', #86207 ) ;
#107426 = ORIENTED_EDGE ( 'NONE', *, *, #94284, .T. ) ;
#107427 = CIRCLE ( 'NONE', #103225, 0.09999999999999982514 ) ;
#107428 = CARTESIAN_POINT ( 'NONE',  ( -1.250000000000001110, 2.500000000000000000, -6.495190528383302464 ) ) ;
#107429 = AXIS2_PLACEMENT_3D ( 'NONE', #34304, #114137, #24467 ) ;
#107430 = CARTESIAN_POINT ( 'NONE',  ( 12.29999999999990301, 2.500000000000000000, -0.3464101615137782364 ) ) ;
#107431 = CARTESIAN_POINT ( 'NONE',  ( -9.600000000000008527, 2.500000000000000000, -5.122947341949750211 ) ) ;
#107432 = SURFACE_STYLE_USAGE ( .BOTH. , #119188 ) ;
#107433 = FACE_OUTER_BOUND ( 'NONE', #78005, .T. ) ;
#107434 = CARTESIAN_POINT ( 'NONE',  ( 4.599999999999940137, 2.500000000000000000, -4.330127018922201643 ) ) ;
#107435 = DIRECTION ( 'NONE',  ( 0.000000000000000000, -0.000000000000000000, 1.000000000000000000 ) ) ;
#107436 = LINE ( 'NONE', #5508, #101204 ) ;
#107437 = EDGE_LOOP ( 'NONE', ( #68304, #109401, #60286, #52404 ) ) ;
#107438 = DIRECTION ( 'NONE',  ( 0.000000000000000000, 1.000000000000000000, 0.000000000000000000 ) ) ;
#107439 = EDGE_LOOP ( 'NONE', ( #54471, #110282 ) ) ;
#107440 = ORIENTED_EDGE ( 'NONE', *, *, #90789, .T. ) ;
#107441 = ORIENTED_EDGE ( 'NONE', *, *, #103710, .T. ) ;
#107442 = EDGE_LOOP ( 'NONE', ( #93949, #87647, #67190, #85153 ) ) ;
#107443 = DIRECTION ( 'NONE',  ( 0.000000000000000000, 0.000000000000000000, 1.000000000000000000 ) ) ;
#107444 = AXIS2_PLACEMENT_3D ( 'NONE', #94724, #75723, #16785 ) ;
#107445 = AXIS2_PLACEMENT_3D ( 'NONE', #16258, #126241, #84380 ) ;
#107446 = ORIENTED_EDGE ( 'NONE', *, *, #20746, .T. ) ;
#107447 = EDGE_LOOP ( 'NONE', ( #82685, #18027 ) ) ;
#107449 = CARTESIAN_POINT ( 'NONE',  ( -0.8500000000000395017, 2.500000000000000000, 6.495190528383297135 ) ) ;
#107448 = AXIS2_PLACEMENT_3D ( 'NONE', #86575, #96386, #6692 ) ;
#107450 = CARTESIAN_POINT ( 'NONE',  ( 3.349999999999941913, 12.50000000000000000, 5.802370205355744659 ) ) ;
#107452 = FACE_OUTER_BOUND ( 'NONE', #93358, .T. ) ;
#107451 = CIRCLE ( 'NONE', #42634, 0.06509327318403741736 ) ;
#107453 = CARTESIAN_POINT ( 'NONE',  ( 1.899999999999951283, 12.50000000000000000, -4.676537180435977881 ) ) ;
#107454 = AXIS2_PLACEMENT_3D ( 'NONE', #39685, #88756, #79585 ) ;
#107455 = DIRECTION ( 'NONE',  ( 0.000000000000000000, 0.000000000000000000, 1.000000000000000000 ) ) ;
#107456 = ORIENTED_EDGE ( 'NONE', *, *, #123010, .T. ) ;
#107457 = CARTESIAN_POINT ( 'NONE',  ( 2.099999999999948574, 2.500000000000000000, 4.230127018922196669 ) ) ;
#107458 = CIRCLE ( 'NONE', #86524, 0.06509327318403745899 ) ;
#107460 = ORIENTED_EDGE ( 'NONE', *, *, #42162, .F. ) ;
#107459 = AXIS2_PLACEMENT_3D ( 'NONE', #55116, #25637, #7283 ) ;
#107461 = FACE_OUTER_BOUND ( 'NONE', #42989, .T. ) ;
#107463 = ADVANCED_FACE ( 'NONE', ( #28606 ), #46300, .T. ) ;
#107462 = AXIS2_PLACEMENT_3D ( 'NONE', #64236, #44601, #15102 ) ;
#107464 = ORIENTED_EDGE ( 'NONE', *, *, #99814, .F. ) ;
#107465 = DIRECTION ( 'NONE',  ( 0.000000000000000000, 0.000000000000000000, 1.000000000000000000 ) ) ;
#107466 = ORIENTED_EDGE ( 'NONE', *, *, #93320, .T. ) ;
#107467 = ADVANCED_FACE ( 'NONE', ( #7651 ), #8728, .T. ) ;
#107468 = VERTEX_POINT ( 'NONE', #97333 ) ;
#107469 = EDGE_CURVE ( 'NONE', #106056, #123660, #123652, .T. ) ;
#107470 = DIRECTION ( 'NONE',  ( 0.000000000000000000, 0.000000000000000000, 1.000000000000000000 ) ) ;
#107471 = LINE ( 'NONE', #55156, #75624 ) ;
#107472 = CARTESIAN_POINT ( 'NONE',  ( 186.1250000000000000, -8.891194145520236347, -1.633285867636356299E-15 ) ) ;
#107473 = PLANE ( 'NONE',  #2597 ) ;
#107474 = AXIS2_PLACEMENT_3D ( 'NONE', #87928, #118048, #98400 ) ;
#107475 = EDGE_CURVE ( 'NONE', #108499, #59648, #68511, .T. ) ;
#107476 = FACE_OUTER_BOUND ( 'NONE', #56036, .T. ) ;
#107478 = ORIENTED_EDGE ( 'NONE', *, *, #70900, .F. ) ;
#107477 = EDGE_CURVE ( 'NONE', #15129, #57241, #17319, .T. ) ;
#107479 = LINE ( 'NONE', #28277, #122968 ) ;
#107480 = LINE ( 'NONE', #117932, #112135 ) ;
#107481 = ADVANCED_FACE ( 'NONE', ( #16172 ), #38439, .T. ) ;
#107482 = DIRECTION ( 'NONE',  ( 0.000000000000000000, 0.000000000000000000, 1.000000000000000000 ) ) ;
#107483 = ADVANCED_FACE ( 'NONE', ( #108434 ), #94416, .T. ) ;
#107484 = EDGE_CURVE ( 'NONE', #113061, #51178, #79006, .T. ) ;
#107485 = DIRECTION ( 'NONE',  ( 0.000000000000000000, -0.9999939076577903929, 0.003490651415223739937 ) ) ;
#107486 = CIRCLE ( 'NONE', #46853, 0.06509327318403745899 ) ;
#107487 = DIRECTION ( 'NONE',  ( -0.000000000000000000, -1.000000000000000000, -0.000000000000000000 ) ) ;
#107488 = ORIENTED_EDGE ( 'NONE', *, *, #102019, .T. ) ;
#107489 = ORIENTED_EDGE ( 'NONE', *, *, #32835, .F. ) ;
#107490 = CARTESIAN_POINT ( 'NONE',  ( -12.29999999999999716, 2.500000000000000000, 0.4464101615137776591 ) ) ;
#107491 = ADVANCED_FACE ( 'NONE', ( #6999 ), #118258, .T. ) ;
#107492 = ORIENTED_EDGE ( 'NONE', *, *, #121126, .F. ) ;
#107493 = AXIS2_PLACEMENT_3D ( 'NONE', #69221, #477, #29973 ) ;
#107494 = FACE_OUTER_BOUND ( 'NONE', #29704, .T. ) ;
#107495 = CARTESIAN_POINT ( 'NONE',  ( 12.49999999999990408, 2.500000000000000000, -3.737306695894649700 ) ) ;
#107496 = AXIS2_PLACEMENT_3D ( 'NONE', #98181, #49107, #68076 ) ;
#107497 = EDGE_LOOP ( 'NONE', ( #103412, #94091, #116278, #28427 ) ) ;
#107498 = CARTESIAN_POINT ( 'NONE',  ( 185.5833333333333144, -6.668395609140180369, 3.849999999999994760 ) ) ;
#107499 = FACE_OUTER_BOUND ( 'NONE', #21792, .T. ) ;
#107500 = CARTESIAN_POINT ( 'NONE',  ( -12.49999999999999289, 12.50000000000000000, -0.7579135962115874925 ) ) ;
#107501 = DIRECTION ( 'NONE',  ( 0.000000000000000000, 0.000000000000000000, 1.000000000000000000 ) ) ;
#107502 = ORIENTED_EDGE ( 'NONE', *, *, #76362, .T. ) ;
#107503 = VECTOR ( 'NONE', #91247, 1000.000000000000000 ) ;
#107504 = DIRECTION ( 'NONE',  ( -0.000000000000000000, -1.000000000000000000, -0.000000000000000000 ) ) ;
#107505 = CARTESIAN_POINT ( 'NONE',  ( -14.79999999999998295, 2.500000000000000000, -0.2464101615137760659 ) ) ;
#107506 = ORIENTED_EDGE ( 'NONE', *, *, #8037, .T. ) ;
#107507 = CARTESIAN_POINT ( 'NONE',  ( 4.549999999999935874, 12.50000000000000000, 6.495190528383297135 ) ) ;
#107508 = CARTESIAN_POINT ( 'NONE',  ( 10.59999999999990905, 2.500000000000000000, 4.676537180435972552 ) ) ;
#107509 = LINE ( 'NONE', #77406, #86747 ) ;
#107510 = EDGE_LOOP ( 'NONE', ( #78774, #23587, #71509, #35901 ) ) ;
#107511 = AXIS2_PLACEMENT_3D ( 'NONE', #40740, #11239, #51832 ) ;
#107512 = AXIS2_PLACEMENT_3D ( 'NONE', #50527, #10588, #122508 ) ;
#107513 = DIRECTION ( 'NONE',  ( 0.000000000000000000, -0.9999939076577903929, 0.003490651415223739937 ) ) ;
#107515 = EDGE_LOOP ( 'NONE', ( #5821, #121741, #35863, #127401 ) ) ;
#107514 = AXIS2_PLACEMENT_3D ( 'NONE', #20473, #82622, #30309 ) ;
#107516 = EDGE_CURVE ( 'NONE', #89903, #110245, #6558, .T. ) ;
#107517 = DIRECTION ( 'NONE',  ( 0.000000000000000000, 0.000000000000000000, 1.000000000000000000 ) ) ;
#107518 = CARTESIAN_POINT ( 'NONE',  ( -7.950000000000012612, 2.500000000000000000, 2.165063509461097713 ) ) ;
#107519 = CARTESIAN_POINT ( 'NONE',  ( 9.149999999999916866, 2.500000000000000000, 5.802370205355744659 ) ) ;
#107520 = ADVANCED_FACE ( 'NONE', ( #46961 ), #67199, .T. ) ;
#107521 = ORIENTED_EDGE ( 'NONE', *, *, #94762, .T. ) ;
#107522 = DIRECTION ( 'NONE',  ( 0.000000000000000000, 1.000000000000000000, 0.000000000000000000 ) ) ;
#107523 = EDGE_CURVE ( 'NONE', #2500, #120531, #315, .T. ) ;
#107524 = FACE_OUTER_BOUND ( 'NONE', #45420, .T. ) ;
#107525 = ORIENTED_EDGE ( 'NONE', *, *, #128901, .T. ) ;
#107526 = CARTESIAN_POINT ( 'NONE',  ( -0.4000000000000339950, 12.50000000000000000, 0.6928203230275518099 ) ) ;
#107527 = EDGE_CURVE ( 'NONE', #74144, #65189, #44240, .T. ) ;
#107528 = VERTEX_POINT ( 'NONE', #96044 ) ;
#107529 = LINE ( 'NONE', #85934, #70402 ) ;
#107530 = EDGE_CURVE ( 'NONE', #269, #84610, #81888, .T. ) ;
#107531 = EDGE_CURVE ( 'NONE', #31429, #116085, #11071, .T. ) ;
#107532 = CONICAL_SURFACE ( 'NONE', #72041, 0.1000000000000002554, 0.003490658503988666988 ) ;
#107533 = ORIENTED_EDGE ( 'NONE', *, *, #111878, .F. ) ;
#107534 = CARTESIAN_POINT ( 'NONE',  ( -12.09999999999999609, 12.50000000000000000, -3.702399969078684627 ) ) ;
#107535 = CARTESIAN_POINT ( 'NONE',  ( -9.600000000000006750, 2.500000000000000000, 3.537306695894645081 ) ) ;
#107536 = VECTOR ( 'NONE', #92000, 1000.000000000000000 ) ;
#107537 = EDGE_LOOP ( 'NONE', ( #84960, #78523, #124772, #15750 ) ) ;
#107538 = EDGE_LOOP ( 'NONE', ( #47974, #16717 ) ) ;
#107539 = CARTESIAN_POINT ( 'NONE',  ( 0.1999999999999567124, 12.50000000000000000, -3.983716857408426293 ) ) ;
#107540 = CARTESIAN_POINT ( 'NONE',  ( 8.549999999999920774, 12.50000000000000000, -2.576566944158915184 ) ) ;
#107541 = EDGE_LOOP ( 'NONE', ( #71969, #69789, #69208, #94987 ) ) ;
#107542 = ADVANCED_FACE ( 'NONE', ( #126152 ), #60974, .T. ) ;
#107543 = DIRECTION ( 'NONE',  ( 0.000000000000000000, 0.000000000000000000, 1.000000000000000000 ) ) ;
#107544 = DIRECTION ( 'NONE',  ( 0.000000000000000000, 1.000000000000000000, 0.000000000000000000 ) ) ;
#107545 = VECTOR ( 'NONE', #55601, 1000.000000000000000 ) ;
#107546 = AXIS2_PLACEMENT_3D ( 'NONE', #30800, #119803, #668 ) ;
#107547 = VECTOR ( 'NONE', #24541, 1000.000000000000000 ) ;
#107548 = DIRECTION ( 'NONE',  ( 0.000000000000000000, 1.000000000000000000, 0.000000000000000000 ) ) ;
#107549 = DIRECTION ( 'NONE',  ( 0.000000000000000000, 0.000000000000000000, 1.000000000000000000 ) ) ;
#107550 = LINE ( 'NONE', #17866, #95434 ) ;
#107551 = DIRECTION ( 'NONE',  ( 0.000000000000000000, 1.000000000000000000, 0.000000000000000000 ) ) ;
#107552 = CIRCLE ( 'NONE', #109617, 0.06509327318403741736 ) ;
#107553 = VECTOR ( 'NONE', #121076, 1000.000000000000000 ) ;
#107554 = EDGE_LOOP ( 'NONE', ( #45757, #63004, #29886, #103860 ) ) ;
#107555 = ORIENTED_EDGE ( 'NONE', *, *, #61987, .F. ) ;
#107556 = ORIENTED_EDGE ( 'NONE', *, *, #29993, .T. ) ;
#107557 = VERTEX_POINT ( 'NONE', #37141 ) ;
#107558 = CARTESIAN_POINT ( 'NONE',  ( -10.84999999999999964, 2.500000000000000000, 7.188010851410848723 ) ) ;
#107559 = DIRECTION ( 'NONE',  ( 0.000000000000000000, 0.000000000000000000, -1.000000000000000000 ) ) ;
#107560 = CIRCLE ( 'NONE', #67844, 0.1000000000000000472 ) ;
#107561 = DIRECTION ( 'NONE',  ( 0.000000000000000000, 0.000000000000000000, 1.000000000000000000 ) ) ;
#107562 = EDGE_LOOP ( 'NONE', ( #17390, #26389, #109512, #97797 ) ) ;
#107563 = FACE_BOUND ( 'NONE', #18366, .T. ) ;
#107564 = EDGE_LOOP ( 'NONE', ( #58324, #118942 ) ) ;
#107565 = ADVANCED_FACE ( 'NONE', ( #116958 ), #73487, .T. ) ;
#107566 = CARTESIAN_POINT ( 'NONE',  ( 4.149999999999941735, 12.50000000000000000, -7.188010851410854052 ) ) ;
#107567 = DIRECTION ( 'NONE',  ( 0.000000000000000000, -0.9999939076577903929, 0.003490651415223739937 ) ) ;
#107568 = DIRECTION ( 'NONE',  ( 1.000000000000000000, 0.000000000000000000, 0.000000000000000000 ) ) ;
#107569 = CARTESIAN_POINT ( 'NONE',  ( -2.500000000000032419, 2.500000000000000000, -3.637306695894650055 ) ) ;
#107570 = DIRECTION ( 'NONE',  ( 0.000000000000000000, 0.000000000000000000, -1.000000000000000000 ) ) ;
#107571 = CARTESIAN_POINT ( 'NONE',  ( -0.2000000000000408673, 12.50000000000000000, -3.983716857408426293 ) ) ;
#107572 = CARTESIAN_POINT ( 'NONE',  ( 2.049999999999950084, 12.50000000000000000, -6.495190528383302464 ) ) ;
#107573 = DIRECTION ( 'NONE',  ( 0.000000000000000000, 1.000000000000000000, 0.000000000000000000 ) ) ;
#107574 = CARTESIAN_POINT ( 'NONE',  ( 11.24999999999994493, 2.500000000000000000, 6.495190528383297135 ) ) ;
#107575 = AXIS2_PLACEMENT_3D ( 'NONE', #84612, #124541, #34888 ) ;
#107576 = DIRECTION ( 'NONE',  ( -0.000000000000000000, -1.000000000000000000, -0.000000000000000000 ) ) ;
#107577 = ORIENTED_EDGE ( 'NONE', *, *, #9950, .F. ) ;
#107578 = ORIENTED_EDGE ( 'NONE', *, *, #103081, .T. ) ;
#107579 = ADVANCED_FACE ( 'NONE', ( #82212 ), #19404, .T. ) ;
#107580 = VERTEX_POINT ( 'NONE', #89448 ) ;
#107581 = ORIENTED_EDGE ( 'NONE', *, *, #31675, .F. ) ;
#107582 = CARTESIAN_POINT ( 'NONE',  ( 17.50000000000001066, -2.481874158964551658, -3.264437049507144195 ) ) ;
#107583 = CARTESIAN_POINT ( 'NONE',  ( 13.14999999999989733, 2.500000000000000000, -1.818653347947325916 ) ) ;
#107585 = ORIENTED_EDGE ( 'NONE', *, *, #70690, .T. ) ;
#107584 = EDGE_LOOP ( 'NONE', ( #108704, #83153, #642, #41920 ) ) ;
#107586 = VERTEX_POINT ( 'NONE', #52113 ) ;
#107587 = DIRECTION ( 'NONE',  ( -4.274815082592931898E-19, -0.9999939076577903929, -0.003490651415223739937 ) ) ;
#107588 = CIRCLE ( 'NONE', #15619, 0.1000000000000000472 ) ;
#107589 = AXIS2_PLACEMENT_3D ( 'NONE', #77111, #85633, #35895 ) ;
#107590 = DIRECTION ( 'NONE',  ( -0.000000000000000000, 1.000000000000000000, -0.000000000000000000 ) ) ;
#107591 = CARTESIAN_POINT ( 'NONE',  ( -7.100000000000014744, 2.500000000000000000, 4.230127018922196669 ) ) ;
#107592 = LINE ( 'NONE', #27728, #109564 ) ;
#107593 = CARTESIAN_POINT ( 'NONE',  ( 187.1979166673494603, 6.668395609140176816, 3.850000000000000977 ) ) ;
#107594 = FACE_OUTER_BOUND ( 'NONE', #84058, .T. ) ;
#107595 = EDGE_CURVE ( 'NONE', #104575, #99398, #40356, .T. ) ;
#107596 = ORIENTED_EDGE ( 'NONE', *, *, #20196, .T. ) ;
#107597 = DIRECTION ( 'NONE',  ( 0.000000000000000000, 0.000000000000000000, 1.000000000000000000 ) ) ;
#107598 = ORIENTED_EDGE ( 'NONE', *, *, #20125, .T. ) ;
#107599 = ORIENTED_EDGE ( 'NONE', *, *, #49877, .T. ) ;
#107600 = ORIENTED_EDGE ( 'NONE', *, *, #9682, .T. ) ;
#107601 = VECTOR ( 'NONE', #79856, 1000.000000000000000 ) ;
#107602 = DIRECTION ( 'NONE',  ( 0.000000000000000000, 0.000000000000000000, 1.000000000000000000 ) ) ;
#107603 = ORIENTED_EDGE ( 'NONE', *, *, #45918, .T. ) ;
#107604 = VERTEX_POINT ( 'NONE', #80930 ) ;
#107605 = DIRECTION ( 'NONE',  ( -0.000000000000000000, 1.000000000000000000, -0.000000000000000000 ) ) ;
#107607 = CIRCLE ( 'NONE', #57433, 0.1000000000000002554 ) ;
#107606 = DIRECTION ( 'NONE',  ( -0.000000000000000000, 1.000000000000000000, -0.000000000000000000 ) ) ;
#107608 = DIRECTION ( 'NONE',  ( 0.000000000000000000, 1.000000000000000000, 0.000000000000000000 ) ) ;
#107609 = AXIS2_PLACEMENT_3D ( 'NONE', #114314, #105786, #46215 ) ;
#107610 = DIRECTION ( 'NONE',  ( -0.000000000000000000, -1.000000000000000000, -0.000000000000000000 ) ) ;
#107612 = AXIS2_PLACEMENT_3D ( 'NONE', #6580, #47200, #97572 ) ;
#107611 = CARTESIAN_POINT ( 'NONE',  ( 2.899999999999946620, 12.50000000000000000, -5.022947341949754119 ) ) ;
#107613 = VERTEX_POINT ( 'NONE', #129407 ) ;
#107614 = VECTOR ( 'NONE', #124104, 1000.000000000000000 ) ;
#107615 = PLANE ( 'NONE',  #107643 ) ;
#107616 = ORIENTED_EDGE ( 'NONE', *, *, #911, .F. ) ;
#107617 = CARTESIAN_POINT ( 'NONE',  ( -3.950000000000026379, 2.500000000000000000, 6.841600689897072485 ) ) ;
#107618 = ADVANCED_FACE ( 'NONE', ( #110997 ), #121608, .T. ) ;
#107619 = ORIENTED_EDGE ( 'NONE', *, *, #105422, .T. ) ;
#107620 = DIRECTION ( 'NONE',  ( -0.000000000000000000, -1.000000000000000000, -0.000000000000000000 ) ) ;
#107621 = CARTESIAN_POINT ( 'NONE',  ( -4.800000000000026468, 2.500000000000000000, -4.776537180435978414 ) ) ;
#107622 = ORIENTED_EDGE ( 'NONE', *, *, #38031, .F. ) ;
#107623 = DIRECTION ( 'NONE',  ( -0.000000000000000000, -1.000000000000000000, -0.000000000000000000 ) ) ;
#107624 = LINE ( 'NONE', #106962, #52204 ) ;
#107625 = ORIENTED_EDGE ( 'NONE', *, *, #32757, .F. ) ;
#107626 = AXIS2_PLACEMENT_3D ( 'NONE', #107294, #117740, #88275 ) ;
#107628 = DIRECTION ( 'NONE',  ( 0.000000000000000000, 1.000000000000000000, 0.000000000000000000 ) ) ;
#107627 = VECTOR ( 'NONE', #12152, 1000.000000000000000 ) ;
#107629 = VERTEX_POINT ( 'NONE', #41664 ) ;
#107630 = CIRCLE ( 'NONE', #103429, 0.06509327318403745899 ) ;
#107631 = EDGE_CURVE ( 'NONE', #91861, #107707, #109741, .T. ) ;
#107632 = AXIS2_PLACEMENT_3D ( 'NONE', #109006, #126740, #99217 ) ;
#107634 = EDGE_LOOP ( 'NONE', ( #32667, #42260 ) ) ;
#107633 = EDGE_CURVE ( 'NONE', #50900, #116451, #79627, .T. ) ;
#107635 = CARTESIAN_POINT ( 'NONE',  ( -5.200000000000020606, 2.500000000000000000, 3.983716857408420964 ) ) ;
#107636 = PLANE ( 'NONE',  #57656 ) ;
#107637 = EDGE_CURVE ( 'NONE', #55845, #124238, #21262, .T. ) ;
#107638 = CARTESIAN_POINT ( 'NONE',  ( 185.6302083336747444, -4.367472073101514418, -7.564683531250002702 ) ) ;
#107639 = EDGE_CURVE ( 'NONE', #44639, #117877, #92025, .T. ) ;
#107640 = FACE_OUTER_BOUND ( 'NONE', #79475, .T. ) ;
#107641 = CARTESIAN_POINT ( 'NONE',  ( 13.94999999999989448, 2.500000000000000000, -2.511473670974877948 ) ) ;
#107642 = CIRCLE ( 'NONE', #11491, 0.06509327318403743123 ) ;
#107643 = AXIS2_PLACEMENT_3D ( 'NONE', #97791, #8114, #108882 ) ;
#107644 = ADVANCED_FACE ( 'NONE', ( #29887 ), #39734, .T. ) ;
#107645 = CARTESIAN_POINT ( 'NONE',  ( -9.400000000000009237, 12.50000000000000000, -4.741630453620011565 ) ) ;
#107646 = AXIS2_PLACEMENT_3D ( 'NONE', #18129, #7009, #127456 ) ;
#107647 = ADVANCED_FACE ( 'NONE', ( #71097 ), #100675, .T. ) ;
#107648 = ORIENTED_EDGE ( 'NONE', *, *, #97448, .F. ) ;
#107649 = EDGE_CURVE ( 'NONE', #48724, #54992, #31741, .T. ) ;
#107650 = AXIS2_PLACEMENT_3D ( 'NONE', #115657, #16152, #83006 ) ;
#107651 = DIRECTION ( 'NONE',  ( 0.000000000000000000, 0.000000000000000000, 1.000000000000000000 ) ) ;
#107653 = CIRCLE ( 'NONE', #76351, 0.06509327318403741736 ) ;
#107652 = DIRECTION ( 'NONE',  ( 0.000000000000000000, -0.9999939076577903929, 0.003490651415223739937 ) ) ;
#107654 = ADVANCED_FACE ( 'NONE', ( #61934 ), #49540, .T. ) ;
#107655 = ORIENTED_EDGE ( 'NONE', *, *, #98833, .F. ) ;
#107656 = CONICAL_SURFACE ( 'NONE', #114007, 0.1000000000000002554, 0.003490658503988666988 ) ;
#107657 = CARTESIAN_POINT ( 'NONE',  ( 8.349999999999923261, 2.500000000000000000, -5.802370205355749988 ) ) ;
#107658 = CARTESIAN_POINT ( 'NONE',  ( 9.999999999999911182, 2.500000000000000000, 5.022947341949748790 ) ) ;
#107659 = CARTESIAN_POINT ( 'NONE',  ( -6.071532165918824830E-15, 12.50000000000000000, -4.330127018922201643 ) ) ;
#107660 = CARTESIAN_POINT ( 'NONE',  ( 14.99999999999989164, 12.50000000000000000, 0.6928203230275494784 ) ) ;
#107661 = EDGE_CURVE ( 'NONE', #110789, #71913, #71424, .T. ) ;
#107662 = CARTESIAN_POINT ( 'NONE',  ( 15.39999999999989022, 12.50000000000000000, -2.385244779468109755E-15 ) ) ;
#107663 = EDGE_LOOP ( 'NONE', ( #1, #3026, #11251, #6970 ) ) ;
#107664 = DIRECTION ( 'NONE',  ( -0.000000000000000000, -1.000000000000000000, -0.000000000000000000 ) ) ;
#107665 = DIRECTION ( 'NONE',  ( 0.000000000000000000, 0.000000000000000000, 1.000000000000000000 ) ) ;
#107666 = AXIS2_PLACEMENT_3D ( 'NONE', #80685, #30307, #29639 ) ;
#107667 = VERTEX_POINT ( 'NONE', #90075 ) ;
#107668 = PLANE ( 'NONE',  #28087 ) ;
#107669 = VERTEX_POINT ( 'NONE', #71751 ) ;
#107670 = EDGE_LOOP ( 'NONE', ( #113901, #125382, #76094, #94321 ) ) ;
#107671 = DIRECTION ( 'NONE',  ( 0.000000000000000000, -0.9999939076577903929, 0.003490651415223739937 ) ) ;
#107672 = ORIENTED_EDGE ( 'NONE', *, *, #2136, .F. ) ;
#107673 = FACE_OUTER_BOUND ( 'NONE', #112889, .T. ) ;
#107674 = DIRECTION ( 'NONE',  ( 1.000000000000000000, -0.000000000000000000, -0.000000000000000000 ) ) ;
#107675 = CIRCLE ( 'NONE', #88893, 0.1000000000000000472 ) ;
#107676 = DIRECTION ( 'NONE',  ( 0.000000000000000000, 0.000000000000000000, 1.000000000000000000 ) ) ;
#107677 = AXIS2_PLACEMENT_3D ( 'NONE', #23991, #41074, #42345 ) ;
#107678 = VERTEX_POINT ( 'NONE', #60016 ) ;
#107679 = CARTESIAN_POINT ( 'NONE',  ( -4.150000000000024336, 2.500000000000000000, 1.572243186433545548 ) ) ;
#107681 = ORIENTED_EDGE ( 'NONE', *, *, #13016, .T. ) ;
#107680 = DIRECTION ( 'NONE',  ( -0.000000000000000000, 1.000000000000000000, -0.000000000000000000 ) ) ;
#107682 = PLANE ( 'NONE',  #4696 ) ;
#107683 = CARTESIAN_POINT ( 'NONE',  ( 10.44999999999991047, 12.50000000000000000, 2.099970236277060032 ) ) ;
#107684 = ORIENTED_EDGE ( 'NONE', *, *, #88118, .T. ) ;
#107685 = CIRCLE ( 'NONE', #74238, 0.06509327318403745899 ) ;
#107686 = ADVANCED_FACE ( 'NONE', ( #111675 ), #40057, .T. ) ;
#107687 = ORIENTED_EDGE ( 'NONE', *, *, #47864, .T. ) ;
#107689 = ADVANCED_FACE ( 'NONE', ( #40366 ), #48457, .T. ) ;
#107688 = CONICAL_SURFACE ( 'NONE', #34556, 0.1000000000000002554, 0.003490658503988666988 ) ;
#107690 = ORIENTED_EDGE ( 'NONE', *, *, #52723, .T. ) ;
#107691 = CARTESIAN_POINT ( 'NONE',  ( 11.69999999999990870, 12.50000000000000000, -4.330127018922201643 ) ) ;
#107692 = DIRECTION ( 'NONE',  ( 0.000000000000000000, -0.000000000000000000, 1.000000000000000000 ) ) ;
#107693 = CARTESIAN_POINT ( 'NONE',  ( -12.49999999999999289, 12.50000000000000000, 3.637306695894644726 ) ) ;
#107694 = FACE_BOUND ( 'NONE', #9056, .T. ) ;
#107695 = ORIENTED_EDGE ( 'NONE', *, *, #15056, .F. ) ;
#107696 = DIRECTION ( 'NONE',  ( 0.000000000000000000, 0.000000000000000000, 1.000000000000000000 ) ) ;
#107697 = DIRECTION ( 'NONE',  ( 0.000000000000000000, 1.000000000000000000, 0.000000000000000000 ) ) ;
#107698 = ORIENTED_EDGE ( 'NONE', *, *, #85232, .F. ) ;
#107699 = EDGE_CURVE ( 'NONE', #104854, #113368, #107229, .T. ) ;
#107701 = CARTESIAN_POINT ( 'NONE',  ( 185.0000000000000000, 0.000000000000000000, 7.700000000000000178 ) ) ;
#107700 = AXIS2_PLACEMENT_3D ( 'NONE', #105767, #46854, #37678 ) ;
#107702 = AXIS2_PLACEMENT_3D ( 'NONE', #24495, #126567, #123970 ) ;
#107703 = CARTESIAN_POINT ( 'NONE',  ( -6.250000000000017764, 12.50000000000000000, 7.188010851410848723 ) ) ;
#107704 = CARTESIAN_POINT ( 'NONE',  ( 12.09999999999990550, 12.50000000000000000, -4.330127018922201643 ) ) ;
#107705 = CARTESIAN_POINT ( 'NONE',  ( -1.650000000000035660, 2.500000000000000000, 7.188010851410848723 ) ) ;
#107706 = CARTESIAN_POINT ( 'NONE',  ( 4.149999999999939959, 2.500000000000000000, -6.495190528383302464 ) ) ;
#107707 = VERTEX_POINT ( 'NONE', #66903 ) ;
#107708 = ORIENTED_EDGE ( 'NONE', *, *, #72304, .F. ) ;
#107709 = ORIENTED_EDGE ( 'NONE', *, *, #19775, .T. ) ;
#107710 = VERTEX_POINT ( 'NONE', #96357 ) ;
#107711 = ORIENTED_EDGE ( 'NONE', *, *, #64064, .T. ) ;
#107712 = CARTESIAN_POINT ( 'NONE',  ( 2.699999999999946443, 12.50000000000000000, -3.918623584224389056 ) ) ;
#107713 = DIRECTION ( 'NONE',  ( 0.000000000000000000, -0.9999939076577903929, 0.003490651415223739937 ) ) ;
#107714 = ORIENTED_EDGE ( 'NONE', *, *, #24902, .F. ) ;
#107715 = FACE_BOUND ( 'NONE', #23068, .T. ) ;
#107716 = AXIS2_PLACEMENT_3D ( 'NONE', #64130, #85701, #24857 ) ;
#107717 = CARTESIAN_POINT ( 'NONE',  ( 6.899999999999928413, 2.500000000000000000, -4.676537180435977881 ) ) ;
#107718 = AXIS2_PLACEMENT_3D ( 'NONE', #44351, #12945, #101998 ) ;
#107719 = CARTESIAN_POINT ( 'NONE',  ( -13.14999999999999147, 12.50000000000000000, 1.818653347947325472 ) ) ;
#107720 = DIRECTION ( 'NONE',  ( -0.000000000000000000, -1.000000000000000000, -0.000000000000000000 ) ) ;
#107721 = CARTESIAN_POINT ( 'NONE',  ( 4.349999999999941025, 2.500000000000000000, -1.818653347947326138 ) ) ;
#107722 = DIRECTION ( 'NONE',  ( 0.000000000000000000, 0.000000000000000000, 1.000000000000000000 ) ) ;
#107723 = VERTEX_POINT ( 'NONE', #42963 ) ;
#107724 = DIRECTION ( 'NONE',  ( 0.000000000000000000, 1.000000000000000000, 0.000000000000000000 ) ) ;
#107725 = CIRCLE ( 'NONE', #13711, 0.09999999999999982514 ) ;
#107726 = EDGE_LOOP ( 'NONE', ( #109487, #70237, #19942, #114762 ) ) ;
#107727 = CIRCLE ( 'NONE', #5305, 0.06509327318403745899 ) ;
#107728 = AXIS2_PLACEMENT_3D ( 'NONE', #123864, #53853, #65597 ) ;
#107729 = EDGE_LOOP ( 'NONE', ( #87667, #93831 ) ) ;
#107730 = ORIENTED_EDGE ( 'NONE', *, *, #93601, .F. ) ;
#107731 = LINE ( 'NONE', #88734, #104891 ) ;
#107732 = CARTESIAN_POINT ( 'NONE',  ( -8.550000000000013145, 12.50000000000000000, 2.511473670974873507 ) ) ;
#107733 = CARTESIAN_POINT ( 'NONE',  ( 15.39999999999989022, 12.50000000000000000, -0.06509327318403980434 ) ) ;
#107734 = ORIENTED_EDGE ( 'NONE', *, *, #87974, .T. ) ;
#107735 = DIRECTION ( 'NONE',  ( 0.000000000000000000, 0.000000000000000000, 1.000000000000000000 ) ) ;
#107736 = AXIS2_PLACEMENT_3D ( 'NONE', #5553, #34407, #55318 ) ;
#107737 = CARTESIAN_POINT ( 'NONE',  ( 11.64999999999990621, 12.50000000000000000, 6.495190528383297135 ) ) ;
#107738 = CARTESIAN_POINT ( 'NONE',  ( -11.64999999999999680, 2.500000000000000000, 5.902370205355745192 ) ) ;
#107739 = DIRECTION ( 'NONE',  ( 0.000000000000000000, 0.000000000000000000, -1.000000000000000000 ) ) ;
#107740 = CARTESIAN_POINT ( 'NONE',  ( 1.249999999999952482, 2.500000000000000000, -5.802370205355749988 ) ) ;
#107742 = AXIS2_PLACEMENT_3D ( 'NONE', #61612, #89764, #22333 ) ;
#107741 = LINE ( 'NONE', #39037, #88521 ) ;
#107743 = ADVANCED_FACE ( 'NONE', ( #7338 ), #21358, .T. ) ;
#107744 = CARTESIAN_POINT ( 'NONE',  ( -6.050000000000017586, 12.50000000000000000, 6.148780366869520009 ) ) ;
#107745 = ADVANCED_FACE ( 'NONE', ( #14095 ), #116012, .T. ) ;
#107746 = VERTEX_POINT ( 'NONE', #62581 ) ;
#107747 = CARTESIAN_POINT ( 'NONE',  ( -7.500000000000001776, -2.500000000000000000, 9.000000000000003553 ) ) ;
#107748 = ORIENTED_EDGE ( 'NONE', *, *, #13602, .F. ) ;
#107749 = ORIENTED_EDGE ( 'NONE', *, *, #11419, .T. ) ;
#107750 = DIRECTION ( 'NONE',  ( 0.000000000000000000, 1.000000000000000000, 0.000000000000000000 ) ) ;
#107751 = DIRECTION ( 'NONE',  ( 0.000000000000000000, 0.000000000000000000, 1.000000000000000000 ) ) ;
#107753 = EDGE_CURVE ( 'NONE', #64553, #83521, #69377, .T. ) ;
#107752 = DIRECTION ( 'NONE',  ( -0.000000000000000000, 1.000000000000000000, -0.000000000000000000 ) ) ;
#107754 = AXIS2_PLACEMENT_3D ( 'NONE', #14483, #23684, #73418 ) ;
#107755 = ORIENTED_EDGE ( 'NONE', *, *, #117977, .T. ) ;
#107756 = EDGE_LOOP ( 'NONE', ( #437, #43521, #84619, #81792 ) ) ;
#107757 = DIRECTION ( 'NONE',  ( 0.000000000000000000, 0.000000000000000000, -1.000000000000000000 ) ) ;
#107758 = FACE_OUTER_BOUND ( 'NONE', #43673, .T. ) ;
#107759 = DIRECTION ( 'NONE',  ( -0.000000000000000000, 1.000000000000000000, -0.000000000000000000 ) ) ;
#107760 = ORIENTED_EDGE ( 'NONE', *, *, #111780, .F. ) ;
#107761 = ORIENTED_EDGE ( 'NONE', *, *, #61385, .T. ) ;
#107762 = CARTESIAN_POINT ( 'NONE',  ( -4.350000000000023626, 2.500000000000000000, -1.918653347947325782 ) ) ;
#107763 = AXIS2_PLACEMENT_3D ( 'NONE', #53161, #121889, #80691 ) ;
#107764 = ORIENTED_EDGE ( 'NONE', *, *, #107368, .F. ) ;
#107766 = CIRCLE ( 'NONE', #105624, 0.1000000000000000472 ) ;
#107765 = CARTESIAN_POINT ( 'NONE',  ( -3.550000000000030909, 2.500000000000000000, -6.841600689897078702 ) ) ;
#107767 = FACE_OUTER_BOUND ( 'NONE', #106202, .T. ) ;
#107768 = ORIENTED_EDGE ( 'NONE', *, *, #13621, .T. ) ;
#107769 = DIRECTION ( 'NONE',  ( 0.000000000000000000, 1.000000000000000000, 0.000000000000000000 ) ) ;
#107770 = EDGE_CURVE ( 'NONE', #61867, #30241, #44341, .T. ) ;
#107771 = DIRECTION ( 'NONE',  ( 0.000000000000000000, 1.000000000000000000, 0.000000000000000000 ) ) ;
#107772 = LINE ( 'NONE', #10833, #57363 ) ;
#107773 = DIRECTION ( 'NONE',  ( 0.000000000000000000, -0.000000000000000000, 1.000000000000000000 ) ) ;
#107774 = VERTEX_POINT ( 'NONE', #17132 ) ;
#107775 = CIRCLE ( 'NONE', #97316, 0.1000000000000000056 ) ;
#107776 = EDGE_CURVE ( 'NONE', #97390, #65136, #96553, .T. ) ;
#107777 = CARTESIAN_POINT ( 'NONE',  ( -10.85000000000000142, 12.50000000000000000, 2.165063509461097713 ) ) ;
#107778 = AXIS2_PLACEMENT_3D ( 'NONE', #94673, #15460, #86122 ) ;
#107779 = ORIENTED_EDGE ( 'NONE', *, *, #35261, .T. ) ;
#107780 = VERTEX_POINT ( 'NONE', #6672 ) ;
#107781 = ADVANCED_FACE ( 'NONE', ( #57090 ), #97019, .T. ) ;
#107782 = EDGE_CURVE ( 'NONE', #124302, #59948, #19193, .T. ) ;
#107783 = DIRECTION ( 'NONE',  ( 0.000000000000000000, 0.000000000000000000, -1.000000000000000000 ) ) ;
#107784 = DIRECTION ( 'NONE',  ( -0.000000000000000000, 1.000000000000000000, -0.000000000000000000 ) ) ;
#107785 = LINE ( 'NONE', #116941, #13383 ) ;
#107786 = ADVANCED_FACE ( 'NONE', ( #46000 ), #12798, .T. ) ;
#107787 = DIRECTION ( 'NONE',  ( -0.000000000000000000, -1.000000000000000000, -0.000000000000000000 ) ) ;
#107788 = EDGE_CURVE ( 'NONE', #24991, #75374, #25543, .T. ) ;
#107789 = CARTESIAN_POINT ( 'NONE',  ( -3.350000000000028511, 12.50000000000000000, 1.407149913249508000 ) ) ;
#107790 = DIRECTION ( 'NONE',  ( 0.000000000000000000, 1.000000000000000000, 0.000000000000000000 ) ) ;
#107791 = AXIS2_PLACEMENT_3D ( 'NONE', #76799, #104942, #114773 ) ;
#107792 = LINE ( 'NONE', #117579, #75954 ) ;
#107793 = DIRECTION ( 'NONE',  ( 0.000000000000000000, 1.000000000000000000, 0.000000000000000000 ) ) ;
#107794 = CARTESIAN_POINT ( 'NONE',  ( 127.5000000000000000, -2.000000000000000000, 5.000000000000001776 ) ) ;
#107795 = EDGE_CURVE ( 'NONE', #97087, #41669, #72400, .T. ) ;
#107796 = EDGE_CURVE ( 'NONE', #5168, #100174, #93322, .T. ) ;
#107797 = DIRECTION ( 'NONE',  ( 0.000000000000000000, 0.000000000000000000, 1.000000000000000000 ) ) ;
#107798 = ADVANCED_FACE ( 'NONE', ( #36826 ), #126491, .T. ) ;
#107799 = EDGE_CURVE ( 'NONE', #96322, #54140, #98706, .T. ) ;
#107800 = VERTEX_POINT ( 'NONE', #53401 ) ;
#107801 = DIRECTION ( 'NONE',  ( 0.000000000000000000, 0.000000000000000000, -1.000000000000000000 ) ) ;
#107802 = DIRECTION ( 'NONE',  ( -0.000000000000000000, -1.000000000000000000, -0.000000000000000000 ) ) ;
#107803 = LINE ( 'NONE', #88804, #57937 ) ;
#107804 = CARTESIAN_POINT ( 'NONE',  ( 13.09999999999990195, 12.50000000000000000, 3.983716857408420076 ) ) ;
#107805 = CARTESIAN_POINT ( 'NONE',  ( -1.900000000000035438, 12.50000000000000000, 3.983716857408420076 ) ) ;
#107806 = EDGE_CURVE ( 'NONE', #44808, #81692, #100760, .T. ) ;
#107807 = VERTEX_POINT ( 'NONE', #63859 ) ;
#107808 = DIRECTION ( 'NONE',  ( 0.000000000000000000, 0.000000000000000000, -1.000000000000000000 ) ) ;
#107809 = VECTOR ( 'NONE', #25131, 1000.000000000000000 ) ;
#107810 = VECTOR ( 'NONE', #51949, 1000.000000000000000 ) ;
#107811 = DIRECTION ( 'NONE',  ( 0.000000000000000000, 1.000000000000000000, 0.000000000000000000 ) ) ;
#107813 = ORIENTED_EDGE ( 'NONE', *, *, #95206, .F. ) ;
#107812 = CARTESIAN_POINT ( 'NONE',  ( 3.949999999999938005, 12.50000000000000000, 6.841600689897072485 ) ) ;
#107814 = ORIENTED_EDGE ( 'NONE', *, *, #56087, .T. ) ;
#107815 = VERTEX_POINT ( 'NONE', #103783 ) ;
#107816 = ORIENTED_EDGE ( 'NONE', *, *, #102582, .F. ) ;
#107817 = VERTEX_POINT ( 'NONE', #76096 ) ;
#107818 = CARTESIAN_POINT ( 'NONE',  ( -5.400000000000023448, 2.500000000000000000, -4.230127018922201998 ) ) ;
#107819 = CONICAL_SURFACE ( 'NONE', #51416, 0.09999999999999982514, 0.003490658503988666988 ) ;
#107820 = EDGE_CURVE ( 'NONE', #60288, #9509, #106204, .T. ) ;
#107821 = DIRECTION ( 'NONE',  ( -4.274815082592931898E-19, -0.9999939076577903929, -0.003490651415223739937 ) ) ;
#107822 = DIRECTION ( 'NONE',  ( -0.000000000000000000, -1.000000000000000000, -0.000000000000000000 ) ) ;
#107823 = AXIS2_PLACEMENT_3D ( 'NONE', #57905, #28437, #57243 ) ;
#107824 = DIRECTION ( 'NONE',  ( 0.000000000000000000, 1.000000000000000000, 0.000000000000000000 ) ) ;
#107825 = AXIS2_PLACEMENT_3D ( 'NONE', #58325, #68115, #120450 ) ;
#107826 = ORIENTED_EDGE ( 'NONE', *, *, #94034, .F. ) ;
#107827 = CIRCLE ( 'NONE', #11682, 0.06509327318403743123 ) ;
#107829 = AXIS2_PLACEMENT_3D ( 'NONE', #79791, #99450, #121007 ) ;
#107828 = CARTESIAN_POINT ( 'NONE',  ( -9.350000000000004974, 12.50000000000000000, 6.776507416713035248 ) ) ;
#107830 = EDGE_LOOP ( 'NONE', ( #74040, #23107, #44163, #60709 ) ) ;
#107831 = FACE_OUTER_BOUND ( 'NONE', #30776, .T. ) ;
#107832 = DIRECTION ( 'NONE',  ( -0.000000000000000000, -1.000000000000000000, -0.000000000000000000 ) ) ;
#107833 = FACE_OUTER_BOUND ( 'NONE', #112474, .T. ) ;
#107834 = DIRECTION ( 'NONE',  ( 0.000000000000000000, 0.000000000000000000, 1.000000000000000000 ) ) ;
#107835 = ORIENTED_EDGE ( 'NONE', *, *, #121124, .F. ) ;
#107836 = ADVANCED_FACE ( 'NONE', ( #123406 ), #14091, .T. ) ;
#107837 = VERTEX_POINT ( 'NONE', #12795 ) ;
#107838 = EDGE_LOOP ( 'NONE', ( #81874, #60415, #100421, #32812 ) ) ;
#107839 = ADVANCED_FACE ( 'NONE', ( #54035 ), #93959, .T. ) ;
#107840 = VERTEX_POINT ( 'NONE', #55330 ) ;
#107841 = CARTESIAN_POINT ( 'NONE',  ( 11.84999999999990372, 12.50000000000000000, -6.083687093685488989 ) ) ;
#107842 = FACE_OUTER_BOUND ( 'NONE', #88051, .T. ) ;
#107843 = CARTESIAN_POINT ( 'NONE',  ( -3.150000000000030553, 2.500000000000000000, 6.148780366869520009 ) ) ;
#107844 = FACE_BOUND ( 'NONE', #102424, .T. ) ;
#107845 = CARTESIAN_POINT ( 'NONE',  ( -9.550000000000006040, 12.50000000000000000, 2.165063509461097713 ) ) ;
#107846 = AXIS2_PLACEMENT_3D ( 'NONE', #68755, #14, #18999 ) ;
#107847 = CARTESIAN_POINT ( 'NONE',  ( 187.2395833340161460, 4.445597072760117285, 7.699999999999999289 ) ) ;
#107848 = DIRECTION ( 'NONE',  ( 0.000000000000000000, 0.000000000000000000, -1.000000000000000000 ) ) ;
#107849 = DIRECTION ( 'NONE',  ( -4.274815082592931898E-19, -0.9999939076577903929, -0.003490651415223739937 ) ) ;
#107850 = CARTESIAN_POINT ( 'NONE',  ( 184.0052083336747160, -6.551208109652278289, 3.782341765624995134 ) ) ;
#107851 = AXIS2_PLACEMENT_3D ( 'NONE', #37389, #78611, #67447 ) ;
#107852 = DIRECTION ( 'NONE',  ( 0.000000000000000000, 1.000000000000000000, 0.000000000000000000 ) ) ;
#107853 = DIRECTION ( 'NONE',  ( 0.000000000000000000, 0.000000000000000000, -1.000000000000000000 ) ) ;
#107854 = CIRCLE ( 'NONE', #57695, 0.09999999999999982514 ) ;
#107855 = CIRCLE ( 'NONE', #120387, 0.06509327318403745899 ) ;
#107856 = DIRECTION ( 'NONE',  ( 0.000000000000000000, 1.000000000000000000, 0.000000000000000000 ) ) ;
#107857 = ORIENTED_EDGE ( 'NONE', *, *, #97021, .F. ) ;
#107858 = EDGE_LOOP ( 'NONE', ( #93495, #61488 ) ) ;
#107859 = VERTEX_POINT ( 'NONE', #102491 ) ;
#107860 = ORIENTED_EDGE ( 'NONE', *, *, #5049, .F. ) ;
#107861 = FACE_OUTER_BOUND ( 'NONE', #124583, .T. ) ;
#107862 = FACE_BOUND ( 'NONE', #8500, .T. ) ;
#107864 = CARTESIAN_POINT ( 'NONE',  ( -6.050000000000020250, 2.500000000000000000, -6.841600689897078702 ) ) ;
#107863 = AXIS2_PLACEMENT_3D ( 'NONE', #96091, #46339, #116366 ) ;
#107866 = CIRCLE ( 'NONE', #112084, 0.1000000000000002554 ) ;
#107865 = VECTOR ( 'NONE', #16286, 1000.000000000000000 ) ;
#107867 = EDGE_LOOP ( 'NONE', ( #15555, #55151 ) ) ;
#107868 = LINE ( 'NONE', #27356, #2808 ) ;
#107869 = DIRECTION ( 'NONE',  ( 0.000000000000000000, 0.000000000000000000, 1.000000000000000000 ) ) ;
#107870 = LINE ( 'NONE', #53144, #87098 ) ;
#107871 = ORIENTED_EDGE ( 'NONE', *, *, #66857, .T. ) ;
#107872 = CARTESIAN_POINT ( 'NONE',  ( 16.55763163376620284, -0.1615157349257290431, 6.093150851882368713 ) ) ;
#107873 = CARTESIAN_POINT ( 'NONE',  ( 21.23528140090977345, 2.699413673072321718, -2.293764360948945757 ) ) ;
#107874 = EDGE_CURVE ( 'NONE', #105467, #58293, #27601, .T. ) ;
#107875 = VERTEX_POINT ( 'NONE', #105048 ) ;
#107876 = EDGE_LOOP ( 'NONE', ( #41269, #9424 ) ) ;
#107877 = DIRECTION ( 'NONE',  ( -0.000000000000000000, 1.000000000000000000, -0.000000000000000000 ) ) ;
#107878 = CARTESIAN_POINT ( 'NONE',  ( -2.100000000000034284, 12.50000000000000000, -2.385244779468109755E-15 ) ) ;
#107879 = CARTESIAN_POINT ( 'NONE',  ( 4.349999999999937472, 12.50000000000000000, 6.841600689897072485 ) ) ;
#107880 = DIRECTION ( 'NONE',  ( 0.000000000000000000, 1.000000000000000000, 0.000000000000000000 ) ) ;
#107881 = EDGE_LOOP ( 'NONE', ( #100468, #52974 ) ) ;
#107882 = DIRECTION ( 'NONE',  ( 0.000000000000000000, 0.000000000000000000, -1.000000000000000000 ) ) ;
#107883 = EDGE_LOOP ( 'NONE', ( #74297, #30018 ) ) ;
#107884 = ADVANCED_FACE ( 'NONE', ( #3007 ), #56838, .T. ) ;
#107885 = EDGE_LOOP ( 'NONE', ( #87957, #3640, #68729, #62643 ) ) ;
#107886 = EDGE_CURVE ( 'NONE', #7603, #112348, #2555, .T. ) ;
#107887 = DIRECTION ( 'NONE',  ( 0.000000000000000000, 0.000000000000000000, -1.000000000000000000 ) ) ;
#107888 = B_SPLINE_CURVE_WITH_KNOTS ( 'NONE', 3,
 ( #52774, #70484, #92709, #3677, #43623, #30585, #50854, #20744, #60684, #100577 ),
 .UNSPECIFIED., .F., .F.,
 ( 4, 2, 2, 2, 4 ),
 ( 4.358438792651350852E-18, 0.0006221151217586977583, 0.001244230243517391180, 0.001866345365276084710, 0.002488460487034778023 ),
 .UNSPECIFIED. ) ;
#107889 = ORIENTED_EDGE ( 'NONE', *, *, #19097, .F. ) ;
#107890 = CARTESIAN_POINT ( 'NONE',  ( 186.6979166673494603, 6.668395609140176816, 3.850000000000000977 ) ) ;
#107891 = FACE_BOUND ( 'NONE', #42611, .T. ) ;
#107892 = AXIS2_PLACEMENT_3D ( 'NONE', #15143, #53177, #55101 ) ;
#107893 = VERTEX_POINT ( 'NONE', #62578 ) ;
#107894 = CIRCLE ( 'NONE', #72407, 0.09999999999999982514 ) ;
#107895 = CARTESIAN_POINT ( 'NONE',  ( 112.3213495094165921, 7.276123333567264595, 2.535987402356341125 ) ) ;
#107896 = VERTEX_POINT ( 'NONE', #84124 ) ;
#107897 = CARTESIAN_POINT ( 'NONE',  ( -6.450000000000016165, 2.500000000000000000, 6.941600689897073018 ) ) ;
#107898 = DIRECTION ( 'NONE',  ( 0.000000000000000000, 0.000000000000000000, 1.000000000000000000 ) ) ;
#107899 =( BOUNDED_CURVE ( )  B_SPLINE_CURVE ( 2, ( #69321, #77228, #119720 ),
 .UNSPECIFIED., .F., .F. ) 
 B_SPLINE_CURVE_WITH_KNOTS ( ( 3, 3 ),
 ( -5.999999999966287552E-08, 0.01488647113978520606 ),
 .UNSPECIFIED. ) 
 CURVE ( )  GEOMETRIC_REPRESENTATION_ITEM ( )  RATIONAL_B_SPLINE_CURVE ( ( 1.000000000000000000, 0.7762344340431585055, 0.8943752373141855561 ) ) 
 REPRESENTATION_ITEM ( '' )  );
#107900 = CARTESIAN_POINT ( 'NONE',  ( 5.649999999999934630, 2.500000000000000000, -2.511473670974877948 ) ) ;
#107902 = EDGE_CURVE ( 'NONE', #101722, #53584, #52737, .T. ) ;
#107901 = PLANE ( 'NONE',  #15219 ) ;
#107903 = FACE_OUTER_BOUND ( 'NONE', #98913, .T. ) ;
#107904 = ORIENTED_EDGE ( 'NONE', *, *, #20081, .T. ) ;
#107907 = VERTEX_POINT ( 'NONE', #95257 ) ;
#107906 = AXIS2_PLACEMENT_3D ( 'NONE', #6398, #128149, #78425 ) ;
#107905 = AXIS2_PLACEMENT_3D ( 'NONE', #121328, #62432, #39585 ) ;
#107908 = EDGE_LOOP ( 'NONE', ( #91069, #7497, #103721, #11424 ) ) ;
#107909 = CARTESIAN_POINT ( 'NONE',  ( -6.650000000000015454, 12.50000000000000000, 2.922977105672686982 ) ) ;
#107910 = DIRECTION ( 'NONE',  ( -0.000000000000000000, 1.000000000000000000, -0.000000000000000000 ) ) ;
#107911 = LINE ( 'NONE', #109189, #20858 ) ;
#107913 = ORIENTED_EDGE ( 'NONE', *, *, #23284, .F. ) ;
#107912 = EDGE_LOOP ( 'NONE', ( #19522, #36621, #118276, #112246 ) ) ;
#107914 = VERTEX_POINT ( 'NONE', #84782 ) ;
#107915 = DIRECTION ( 'NONE',  ( 0.000000000000000000, 1.000000000000000000, 0.000000000000000000 ) ) ;
#107916 = CIRCLE ( 'NONE', #66144, 0.1000000000000000056 ) ;
#107917 = DIRECTION ( 'NONE',  ( -0.000000000000000000, -1.000000000000000000, -0.000000000000000000 ) ) ;
#107918 = CONICAL_SURFACE ( 'NONE', #118288, 0.1000000000000000472, 0.003490658503988666988 ) ;
#107919 = PRODUCT_CONTEXT ( 'NONE', #56335, 'mechanical' ) ;
#107920 = CARTESIAN_POINT ( 'NONE',  ( 7.699999999999923794, 12.50000000000000000, -3.983716857408426293 ) ) ;
#107921 = DIRECTION ( 'NONE',  ( 0.000000000000000000, 1.000000000000000000, 0.000000000000000000 ) ) ;
#107922 = DIRECTION ( 'NONE',  ( 0.000000000000000000, 0.000000000000000000, -1.000000000000000000 ) ) ;
#107923 = CARTESIAN_POINT ( 'NONE',  ( -9.150000000000005684, 2.500000000000000000, 6.495190528383297135 ) ) ;
#107924 = DIRECTION ( 'NONE',  ( 0.000000000000000000, 0.000000000000000000, -1.000000000000000000 ) ) ;
#107925 = DIRECTION ( 'NONE',  ( -0.000000000000000000, -1.000000000000000000, -0.000000000000000000 ) ) ;
#107926 = ORIENTED_EDGE ( 'NONE', *, *, #84105, .T. ) ;
#107927 = VERTEX_POINT ( 'NONE', #83507 ) ;
#107928 = ADVANCED_FACE ( 'NONE', ( #114241 ), #104418, .T. ) ;
#107929 = PLANE ( 'NONE',  #71718 ) ;
#107930 = CARTESIAN_POINT ( 'NONE',  ( 4.599999999999937472, 12.50000000000000000, 0.6928203230275494784 ) ) ;
#107931 = ORIENTED_EDGE ( 'NONE', *, *, #34204, .F. ) ;
#107932 = ORIENTED_EDGE ( 'NONE', *, *, #101700, .T. ) ;
#107933 = EDGE_CURVE ( 'NONE', #81561, #29893, #61073, .T. ) ;
#107934 = CARTESIAN_POINT ( 'NONE',  ( 186.3177083336747160, 4.367472073101515306, 7.564683531250000925 ) ) ;
#107935 = DIRECTION ( 'NONE',  ( 0.000000000000000000, 1.000000000000000000, 0.000000000000000000 ) ) ;
#107936 = AXIS2_PLACEMENT_3D ( 'NONE', #90827, #11619, #62672 ) ;
#107937 = DIRECTION ( 'NONE',  ( -0.000000000000000000, 1.000000000000000000, -0.000000000000000000 ) ) ;
#107938 = ADVANCED_FACE ( 'NONE', ( #24571 ), #92359, .T. ) ;
#107939 = CARTESIAN_POINT ( 'NONE',  ( -7.500000000000016875, 2.500000000000000000, -3.637306695894650055 ) ) ;
#107940 = CARTESIAN_POINT ( 'NONE',  ( -7.100000000000017408, 2.500000000000000000, 0.5928203230275495006 ) ) ;
#107941 = DIRECTION ( 'NONE',  ( -0.000000000000000000, 1.000000000000000000, -0.000000000000000000 ) ) ;
#107942 = CIRCLE ( 'NONE', #97563, 0.1000000000000000472 ) ;
#107943 = CIRCLE ( 'NONE', #80769, 0.1000000000000002554 ) ;
#107944 = CARTESIAN_POINT ( 'NONE',  ( 6.899999999999928413, 2.500000000000000000, 4.083716857408421497 ) ) ;
#107945 = EDGE_LOOP ( 'NONE', ( #22029, #97595 ) ) ;
#107946 = LINE ( 'NONE', #98757, #72803 ) ;
#107947 = EDGE_CURVE ( 'NONE', #32914, #86614, #411, .T. ) ;
#107948 = EDGE_CURVE ( 'NONE', #72026, #21011, #34417, .T. ) ;
#107949 = EDGE_CURVE ( 'NONE', #18418, #118169, #125804, .T. ) ;
#107950 = AXIS2_PLACEMENT_3D ( 'NONE', #31566, #71473, #32231 ) ;
#107951 = ADVANCED_FACE ( 'NONE', ( #53398 ), #4598, .T. ) ;
#107952 = CONICAL_SURFACE ( 'NONE', #72450, 0.09999999999999982514, 0.003490658503988666988 ) ;
#107953 = DIRECTION ( 'NONE',  ( 0.000000000000000000, 1.000000000000000000, 0.000000000000000000 ) ) ;
#107954 = EDGE_LOOP ( 'NONE', ( #62402, #98273 ) ) ;
#107955 = AXIS2_PLACEMENT_3D ( 'NONE', #57487, #26731, #106567 ) ;
#107956 = EDGE_CURVE ( 'NONE', #71603, #48770, #79846, .T. ) ;
#107957 = VERTEX_POINT ( 'NONE', #25202 ) ;
#107958 = ORIENTED_EDGE ( 'NONE', *, *, #126689, .F. ) ;
#107959 = EDGE_LOOP ( 'NONE', ( #48526, #79612 ) ) ;
#107960 = CARTESIAN_POINT ( 'NONE',  ( 4.399999999999939071, 12.50000000000000000, -0.4115034346978156399 ) ) ;
#107961 = DIRECTION ( 'NONE',  ( -4.274815082592931898E-19, -0.9999939076577903929, -0.003490651415223739937 ) ) ;
#107962 = ADVANCED_FACE ( 'NONE', ( #65120 ), #33879, .T. ) ;
#107963 = AXIS2_PLACEMENT_3D ( 'NONE', #108160, #127809, #37514 ) ;
#107964 = ORIENTED_EDGE ( 'NONE', *, *, #13520, .T. ) ;
#107965 = CARTESIAN_POINT ( 'NONE',  ( 1.449999999999952216, 12.50000000000000000, -2.576566944158915184 ) ) ;
#107966 = CARTESIAN_POINT ( 'NONE',  ( 17.50000000000000000, -0.9166666666666694052, -3.999999999999998224 ) ) ;
#107967 = AXIS2_PLACEMENT_3D ( 'NONE', #50287, #129520, #30012 ) ;
#107968 = LINE ( 'NONE', #58866, #76258 ) ;
#107970 = ORIENTED_EDGE ( 'NONE', *, *, #49592, .T. ) ;
#107969 = DIRECTION ( 'NONE',  ( 0.000000000000000000, 1.000000000000000000, 0.000000000000000000 ) ) ;
#107971 = LINE ( 'NONE', #18292, #30645 ) ;
#107972 = DIRECTION ( 'NONE',  ( -0.000000000000000000, -1.000000000000000000, -0.000000000000000000 ) ) ;
#107973 = ORIENTED_EDGE ( 'NONE', *, *, #22890, .F. ) ;
#107974 = EDGE_LOOP ( 'NONE', ( #121650, #52926, #115615, #15261 ) ) ;
#107975 = ORIENTED_EDGE ( 'NONE', *, *, #72991, .F. ) ;
#107976 = DIRECTION ( 'NONE',  ( -0.000000000000000000, -1.000000000000000000, -0.000000000000000000 ) ) ;
#107977 = DIRECTION ( 'NONE',  ( -0.000000000000000000, -1.000000000000000000, -0.000000000000000000 ) ) ;
#107978 = ORIENTED_EDGE ( 'NONE', *, *, #115420, .T. ) ;
#107979 = CARTESIAN_POINT ( 'NONE',  ( 12.29999999999990301, 2.500000000000000000, -0.4464101615137782142 ) ) ;
#107980 = DIRECTION ( 'NONE',  ( 0.000000000000000000, 0.000000000000000000, 1.000000000000000000 ) ) ;
#107981 = DIRECTION ( 'NONE',  ( 0.000000000000000000, 0.000000000000000000, 1.000000000000000000 ) ) ;
#107982 = DIRECTION ( 'NONE',  ( 0.000000000000000000, -0.9999939076577903929, 0.003490651415223739937 ) ) ;
#107983 = EDGE_LOOP ( 'NONE', ( #30378, #51915 ) ) ;
#107984 = DIRECTION ( 'NONE',  ( 0.000000000000000000, 0.000000000000000000, -1.000000000000000000 ) ) ;
#107985 = EDGE_CURVE ( 'NONE', #17292, #124192, #73577, .T. ) ;
#107986 = VECTOR ( 'NONE', #34081, 1000.000000000000000 ) ;
#107987 = ORIENTED_EDGE ( 'NONE', *, *, #89318, .T. ) ;
#107988 = ORIENTED_EDGE ( 'NONE', *, *, #38696, .F. ) ;
#107989 = CARTESIAN_POINT ( 'NONE',  ( 9.599999999999914380, 12.50000000000000000, -4.330127018922201643 ) ) ;
#107990 = CARTESIAN_POINT ( 'NONE',  ( -2.300000000000033573, 2.500000000000000000, 0.2464101615137735679 ) ) ;
#107991 = FACE_BOUND ( 'NONE', #127101, .T. ) ;
#107992 = DIRECTION ( 'NONE',  ( 0.000000000000000000, 1.000000000000000000, 0.000000000000000000 ) ) ;
#107993 = CARTESIAN_POINT ( 'NONE',  ( 14.39999999999989555, 2.500000000000000000, -0.3464101615137782364 ) ) ;
#107995 = AXIS2_PLACEMENT_3D ( 'NONE', #105114, #113659, #15435 ) ;
#107994 = AXIS2_PLACEMENT_3D ( 'NONE', #2675, #94286, #55008 ) ;
#107996 = FACE_OUTER_BOUND ( 'NONE', #96130, .T. ) ;
#107997 = EDGE_CURVE ( 'NONE', #24704, #109720, #95893, .T. ) ;
#107998 = ORIENTED_EDGE ( 'NONE', *, *, #10116, .T. ) ;
#107999 = DIRECTION ( 'NONE',  ( 0.000000000000000000, 0.000000000000000000, -1.000000000000000000 ) ) ;
#108000 = FACE_OUTER_BOUND ( 'NONE', #16968, .T. ) ;
#108001 = FACE_OUTER_BOUND ( 'NONE', #22392, .T. ) ;
#108002 = DIRECTION ( 'NONE',  ( 0.000000000000000000, 0.000000000000000000, 1.000000000000000000 ) ) ;
#108003 = ORIENTED_EDGE ( 'NONE', *, *, #544, .T. ) ;
#108004 = AXIS2_PLACEMENT_3D ( 'NONE', #117160, #58281, #118469 ) ;
#108005 = CARTESIAN_POINT ( 'NONE',  ( -3.642919299551294898E-14, 12.50000000000000000, 0.7579135962115892688 ) ) ;
#108006 = VECTOR ( 'NONE', #26785, 1000.000000000000000 ) ;
#108007 = DIRECTION ( 'NONE',  ( -0.000000000000000000, -1.000000000000000000, -0.000000000000000000 ) ) ;
#108008 = ORIENTED_EDGE ( 'NONE', *, *, #127276, .T. ) ;
#108009 = ORIENTED_EDGE ( 'NONE', *, *, #107902, .T. ) ;
#108010 = DIRECTION ( 'NONE',  ( -0.000000000000000000, -1.000000000000000000, -0.000000000000000000 ) ) ;
#108011 = FACE_OUTER_BOUND ( 'NONE', #29006, .T. ) ;
#108012 = FACE_BOUND ( 'NONE', #44465, .T. ) ;
#108013 = FACE_OUTER_BOUND ( 'NONE', #78228, .T. ) ;
#108014 = ORIENTED_EDGE ( 'NONE', *, *, #76917, .F. ) ;
#108015 = FACE_OUTER_BOUND ( 'NONE', #48932, .T. ) ;
#108016 = ORIENTED_EDGE ( 'NONE', *, *, #93006, .T. ) ;
#108017 = EDGE_LOOP ( 'NONE', ( #108364, #30610, #46275, #46061 ) ) ;
#108018 = DIRECTION ( 'NONE',  ( -0.000000000000000000, -1.000000000000000000, -0.000000000000000000 ) ) ;
#108019 = CARTESIAN_POINT ( 'NONE',  ( 184.2552083336747444, 6.551208109652275624, -3.782341765624998686 ) ) ;
#108020 = AXIS2_PLACEMENT_3D ( 'NONE', #88064, #39671, #128024 ) ;
#108021 = VECTOR ( 'NONE', #5972, 1000.000000000000000 ) ;
#108022 = VERTEX_POINT ( 'NONE', #105719 ) ;
#108023 = CARTESIAN_POINT ( 'NONE',  ( 3.099999999999943245, 2.500000000000000000, 4.083716857408420609 ) ) ;
#108024 = VECTOR ( 'NONE', #97744, 1000.000000000000000 ) ;
#108025 = LINE ( 'NONE', #78596, #23976 ) ;
#108026 = EDGE_CURVE ( 'NONE', #92529, #76531, #50603, .T. ) ;
#108027 = FACE_OUTER_BOUND ( 'NONE', #91645, .T. ) ;
#108028 = DIRECTION ( 'NONE',  ( 0.000000000000000000, -0.9999939076577903929, 0.003490651415223739937 ) ) ;
#108029 = AXIS2_PLACEMENT_3D ( 'NONE', #122215, #32561, #72469 ) ;
#108030 = AXIS2_PLACEMENT_3D ( 'NONE', #113995, #117022, #117662 ) ;
#108031 = EDGE_CURVE ( 'NONE', #37336, #6486, #35691, .T. ) ;
#108032 = ORIENTED_EDGE ( 'NONE', *, *, #116238, .T. ) ;
#108033 = DIRECTION ( 'NONE',  ( 0.000000000000000000, 0.000000000000000000, 1.000000000000000000 ) ) ;
#108034 = CARTESIAN_POINT ( 'NONE',  ( 13.09999999999989839, 2.500000000000000000, -0.3464101615137783474 ) ) ;
#108035 = ORIENTED_EDGE ( 'NONE', *, *, #55764, .T. ) ;
#108036 = EDGE_CURVE ( 'NONE', #116926, #107710, #123744, .T. ) ;
#108037 = DIRECTION ( 'NONE',  ( 0.000000000000000000, 0.000000000000000000, 1.000000000000000000 ) ) ;
#108038 = ORIENTED_EDGE ( 'NONE', *, *, #35271, .F. ) ;
#108039 = AXIS2_PLACEMENT_3D ( 'NONE', #19023, #81816, #52366 ) ;
#108040 = ADVANCED_FACE ( 'NONE', ( #27149 ), #56589, .T. ) ;
#108041 = PLANE ( 'NONE',  #88984 ) ;
#108042 = CONICAL_SURFACE ( 'NONE', #39129, 0.1000000000000002554, 0.003490658503988666988 ) ;
#108043 = VERTEX_POINT ( 'NONE', #18615 ) ;
#108044 = FACE_OUTER_BOUND ( 'NONE', #94800, .T. ) ;
#108045 = DIRECTION ( 'NONE',  ( 0.000000000000000000, 1.846105847067148761E-16, 1.000000000000000000 ) ) ;
#108046 = LINE ( 'NONE', #61380, #35069 ) ;
#108048 = VECTOR ( 'NONE', #13856, 1000.000000000000000 ) ;
#108047 = AXIS2_PLACEMENT_3D ( 'NONE', #89411, #39695, #10207 ) ;
#108049 = DIRECTION ( 'NONE',  ( 0.000000000000000000, 1.000000000000000000, 0.000000000000000000 ) ) ;
#108050 = ORIENTED_EDGE ( 'NONE', *, *, #48861, .T. ) ;
#108051 = ADVANCED_FACE ( 'NONE', ( #96507 ), #100860, .T. ) ;
#108052 = CARTESIAN_POINT ( 'NONE',  ( 0.8499999999999553468, 2.500000000000000000, -2.957883832488653830 ) ) ;
#108053 = DIRECTION ( 'NONE',  ( 0.000000000000000000, -0.000000000000000000, 1.000000000000000000 ) ) ;
#108054 = DIRECTION ( 'NONE',  ( 0.000000000000000000, -0.9999939076577903929, 0.003490651415223739937 ) ) ;
#108055 = DIRECTION ( 'NONE',  ( 0.000000000000000000, 0.000000000000000000, -1.000000000000000000 ) ) ;
#108056 = CARTESIAN_POINT ( 'NONE',  ( -6.083778633910298187E-15, 2.500000000000000000, -4.430127018922202176 ) ) ;
#108057 = EDGE_CURVE ( 'NONE', #82164, #13480, #57260, .T. ) ;
#108058 = DIRECTION ( 'NONE',  ( -0.000000000000000000, -1.000000000000000000, -0.000000000000000000 ) ) ;
#108059 = EDGE_LOOP ( 'NONE', ( #104629, #89230, #75259, #16077 ) ) ;
#108060 = ORIENTED_EDGE ( 'NONE', *, *, #90340, .F. ) ;
#108061 = CARTESIAN_POINT ( 'NONE',  ( -9.400000000000007461, 2.500000000000000000, 0.3464101615137735735 ) ) ;
#108062 = ORIENTED_EDGE ( 'NONE', *, *, #84585, .F. ) ;
#108063 = FACE_OUTER_BOUND ( 'NONE', #12170, .T. ) ;
#108065 = ORIENTED_EDGE ( 'NONE', *, *, #7231, .F. ) ;
#108064 = ORIENTED_EDGE ( 'NONE', *, *, #77187, .T. ) ;
#108066 = VERTEX_POINT ( 'NONE', #6833 ) ;
#108067 = CIRCLE ( 'NONE', #51652, 0.1000000000000000472 ) ;
#108068 = CARTESIAN_POINT ( 'NONE',  ( 17.50000000000000000, 2.500000000000000000, -3.999999999999996447 ) ) ;
#108069 = CARTESIAN_POINT ( 'NONE',  ( 6.849999999999929479, 12.50000000000000000, 6.841600689897072485 ) ) ;
#108070 = DIRECTION ( 'NONE',  ( 0.000000000000000000, 0.000000000000000000, 1.000000000000000000 ) ) ;
#108071 = DIRECTION ( 'NONE',  ( 1.000000000000000000, -0.000000000000000000, -0.000000000000000000 ) ) ;
#108072 = DIRECTION ( 'NONE',  ( 0.000000000000000000, -0.000000000000000000, 1.000000000000000000 ) ) ;
#108073 = CARTESIAN_POINT ( 'NONE',  ( -0.4000000000000331624, 12.50000000000000000, -0.6928203230275519209 ) ) ;
#108074 = DIRECTION ( 'NONE',  ( 0.000000000000000000, 1.000000000000000000, 0.000000000000000000 ) ) ;
#108075 = ORIENTED_EDGE ( 'NONE', *, *, #43107, .T. ) ;
#108076 = ORIENTED_EDGE ( 'NONE', *, *, #100518, .F. ) ;
#108077 = ORIENTED_EDGE ( 'NONE', *, *, #43595, .T. ) ;
#108078 = AXIS2_PLACEMENT_3D ( 'NONE', #67053, #83670, #33918 ) ;
#108079 = FACE_OUTER_BOUND ( 'NONE', #96733, .T. ) ;
#108080 = EDGE_LOOP ( 'NONE', ( #99339, #62607, #111496, #122584 ) ) ;
#108081 = VERTEX_POINT ( 'NONE', #46801 ) ;
#108084 = EDGE_CURVE ( 'NONE', #25178, #121192, #115518, .T. ) ;
#108083 = CIRCLE ( 'NONE', #101840, 0.1000000000000000056 ) ;
#108082 = CONICAL_SURFACE ( 'NONE', #101838, 0.1000000000000000472, 0.003490658503988666988 ) ;
#108085 = DIRECTION ( 'NONE',  ( 0.000000000000000000, 0.000000000000000000, 1.000000000000000000 ) ) ;
#108086 = CARTESIAN_POINT ( 'NONE',  ( -5.650000000000019895, 2.500000000000000000, 2.411473670974873862 ) ) ;
#108087 = CARTESIAN_POINT ( 'NONE',  ( 10.84999999999991260, 2.500000000000000000, 6.395190528383296602 ) ) ;
#108088 = FACE_OUTER_BOUND ( 'NONE', #112187, .T. ) ;
#108089 = EDGE_CURVE ( 'NONE', #5141, #22283, #46482, .T. ) ;
#108090 = CARTESIAN_POINT ( 'NONE',  ( -11.05000000000000071, 2.500000000000000000, 6.941600689897073018 ) ) ;
#108091 = ORIENTED_EDGE ( 'NONE', *, *, #6121, .T. ) ;
#108092 = EDGE_CURVE ( 'NONE', #76885, #45239, #30247, .T. ) ;
#108093 = ADVANCED_FACE ( 'NONE', ( #76896 ), #84132, .T. ) ;
#108094 = DIRECTION ( 'NONE',  ( -1.000000000000000000, -0.000000000000000000, -0.000000000000000000 ) ) ;
#108097 = EDGE_CURVE ( 'NONE', #37483, #129577, #16658, .T. ) ;
#108096 = AXIS2_PLACEMENT_3D ( 'NONE', #67928, #47020, #77732 ) ;
#108095 = AXIS2_PLACEMENT_3D ( 'NONE', #25521, #127451, #8940 ) ;
#108098 = ORIENTED_EDGE ( 'NONE', *, *, #82421, .T. ) ;
#108099 = DIRECTION ( 'NONE',  ( 0.000000000000000000, 0.000000000000000000, 1.000000000000000000 ) ) ;
#108100 = VECTOR ( 'NONE', #65026, 1000.000000000000000 ) ;
#108101 = ORIENTED_EDGE ( 'NONE', *, *, #89155, .T. ) ;
#108102 = CARTESIAN_POINT ( 'NONE',  ( 4.799999999999935874, 2.500000000000000000, 0.3464101615137735735 ) ) ;
#108103 = EDGE_CURVE ( 'NONE', #127931, #78711, #23501, .T. ) ;
#108104 = VERTEX_POINT ( 'NONE', #37628 ) ;
#108105 = ORIENTED_EDGE ( 'NONE', *, *, #46582, .F. ) ;
#108106 = LINE ( 'NONE', #116635, #98417 ) ;
#108107 = CARTESIAN_POINT ( 'NONE',  ( -11.89999999999999680, 2.500000000000000000, -3.983716857408423628 ) ) ;
#108108 = EDGE_CURVE ( 'NONE', #7764, #33696, #27702, .T. ) ;
#108109 = EDGE_CURVE ( 'NONE', #124470, #60953, #102925, .T. ) ;
#108110 = CARTESIAN_POINT ( 'NONE',  ( -9.200000000000009948, 12.50000000000000000, -4.395220292106235327 ) ) ;
#108111 = LINE ( 'NONE', #127757, #126234 ) ;
#108112 = DIRECTION ( 'NONE',  ( 0.000000000000000000, 0.000000000000000000, 1.000000000000000000 ) ) ;
#108113 = VERTEX_POINT ( 'NONE', #19920 ) ;
#108114 = CARTESIAN_POINT ( 'NONE',  ( -5.200000000000024158, 2.500000000000000000, -4.776537180435977525 ) ) ;
#108115 = DIRECTION ( 'NONE',  ( 0.000000000000000000, 0.000000000000000000, 1.000000000000000000 ) ) ;
#108116 = FACE_OUTER_BOUND ( 'NONE', #61843, .T. ) ;
#108117 = DIRECTION ( 'NONE',  ( -0.000000000000000000, -1.000000000000000000, -0.000000000000000000 ) ) ;
#108118 = CIRCLE ( 'NONE', #83009, 0.06509327318403745899 ) ;
#108119 = CONICAL_SURFACE ( 'NONE', #20300, 0.1000000000000000472, 0.003490658503988666988 ) ;
#108120 = CARTESIAN_POINT ( 'NONE',  ( 8.149999999999920419, 12.50000000000000000, -1.818653347947325916 ) ) ;
#108121 = ORIENTED_EDGE ( 'NONE', *, *, #66578, .F. ) ;
#108122 = AXIS2_PLACEMENT_3D ( 'NONE', #104303, #15906, #95768 ) ;
#108123 = VERTEX_POINT ( 'NONE', #50041 ) ;
#108124 = DIRECTION ( 'NONE',  ( 0.000000000000000000, -0.9999939076577903929, 0.003490651415223739937 ) ) ;
#108125 = ADVANCED_FACE ( 'NONE', ( #120689 ), #11373, .T. ) ;
#108126 = CIRCLE ( 'NONE', #83102, 0.06509327318403741736 ) ;
#108127 = ORIENTED_EDGE ( 'NONE', *, *, #2434, .F. ) ;
#108128 = CONICAL_SURFACE ( 'NONE', #51706, 0.1000000000000002554, 0.003490658503988666988 ) ;
#108129 = DIRECTION ( 'NONE',  ( 0.000000000000000000, 1.000000000000000000, 0.000000000000000000 ) ) ;
#108130 = DIRECTION ( 'NONE',  ( -1.000000000000000000, -0.000000000000000000, 1.445602896647339656E-16 ) ) ;
#108131 = CIRCLE ( 'NONE', #110281, 0.1000000000000002554 ) ;
#108132 = AXIS2_PLACEMENT_3D ( 'NONE', #68698, #36024, #107980 ) ;
#108133 = VERTEX_POINT ( 'NONE', #70305 ) ;
#108134 = CARTESIAN_POINT ( 'NONE',  ( 184.7083333333333144, -4.445597072760115509, -7.700000000000001954 ) ) ;
#108135 = CARTESIAN_POINT ( 'NONE',  ( -15.79999999999998117, 2.500000000000000000, 0.1000000000000000056 ) ) ;
#108136 = PLANE ( 'NONE',  #52432 ) ;
#108137 = DIRECTION ( 'NONE',  ( 0.000000000000000000, 0.000000000000000000, 1.000000000000000000 ) ) ;
#108138 = VERTEX_POINT ( 'NONE', #19242 ) ;
#108140 = AXIS2_PLACEMENT_3D ( 'NONE', #37387, #7246, #21433 ) ;
#108139 = CIRCLE ( 'NONE', #110210, 0.06509327318403745899 ) ;
#108141 = DIRECTION ( 'NONE',  ( 0.000000000000000000, 0.000000000000000000, -1.000000000000000000 ) ) ;
#108142 = VERTEX_POINT ( 'NONE', #68999 ) ;
#108143 = FACE_OUTER_BOUND ( 'NONE', #93679, .T. ) ;
#108144 = CARTESIAN_POINT ( 'NONE',  ( 0.1999999999999567124, 2.500000000000000000, -3.883716857408426648 ) ) ;
#108145 = CARTESIAN_POINT ( 'NONE',  ( 3.949999999999942446, 2.500000000000000000, -6.841600689897078702 ) ) ;
#108146 = ADVANCED_FACE ( 'NONE', ( #1548 ), #128071, .T. ) ;
#108147 = ORIENTED_EDGE ( 'NONE', *, *, #100125, .F. ) ;
#108148 = DIRECTION ( 'NONE',  ( -4.274815082592931898E-19, -0.9999939076577903929, -0.003490651415223739937 ) ) ;
#108149 = ORIENTED_EDGE ( 'NONE', *, *, #111527, .F. ) ;
#108150 = CARTESIAN_POINT ( 'NONE',  ( 5.849999999999935696, 2.500000000000000000, -7.288010851410854585 ) ) ;
#108151 = DIRECTION ( 'NONE',  ( -4.274815082592931898E-19, -0.9999939076577903929, -0.003490651415223739937 ) ) ;
#108152 = AXIS2_PLACEMENT_3D ( 'NONE', #106233, #125856, #18486 ) ;
#108153 = CARTESIAN_POINT ( 'NONE',  ( -14.14999999999998792, 2.500000000000000000, 2.757883832488653209 ) ) ;
#108154 = ORIENTED_EDGE ( 'NONE', *, *, #18822, .F. ) ;
#108155 = PLANE ( 'NONE',  #80242 ) ;
#108156 = LINE ( 'NONE', #7374, #24507 ) ;
#108157 = EDGE_LOOP ( 'NONE', ( #29485, #83402 ) ) ;
#108158 = CARTESIAN_POINT ( 'NONE',  ( 8.099999999999923261, 12.50000000000000000, -4.611443907251940644 ) ) ;
#108159 = ORIENTED_EDGE ( 'NONE', *, *, #38536, .T. ) ;
#108160 = CARTESIAN_POINT ( 'NONE',  ( 8.149999999999920419, 2.500000000000000000, 6.841600689897072485 ) ) ;
#108161 = CONICAL_SURFACE ( 'NONE', #72678, 0.1000000000000000056, 0.003490658503988666988 ) ;
#108162 = VECTOR ( 'NONE', #125208, 1000.000000000000000 ) ;
#108163 = ORIENTED_EDGE ( 'NONE', *, *, #60418, .F. ) ;
#108164 = CARTESIAN_POINT ( 'NONE',  ( 9.999999999999911182, 12.50000000000000000, 5.022947341949748790 ) ) ;
#108165 = FACE_OUTER_BOUND ( 'NONE', #63796, .T. ) ;
#108166 = VERTEX_POINT ( 'NONE', #252 ) ;
#108167 = ORIENTED_EDGE ( 'NONE', *, *, #121793, .T. ) ;
#108168 = DIRECTION ( 'NONE',  ( 0.000000000000000000, 0.000000000000000000, 1.000000000000000000 ) ) ;
#108169 = CARTESIAN_POINT ( 'NONE',  ( -3.950000000000026379, 12.50000000000000000, 2.511473670974873507 ) ) ;
#108170 = ORIENTED_EDGE ( 'NONE', *, *, #109584, .F. ) ;
#108171 = CIRCLE ( 'NONE', #20364, 0.09999999999999982514 ) ;
#108172 = DIRECTION ( 'NONE',  ( 0.000000000000000000, -1.846105847067148515E-16, -1.000000000000000000 ) ) ;
#108173 = CARTESIAN_POINT ( 'NONE',  ( 186.8593750003414016, 0.000000000000000000, 7.564683531250000925 ) ) ;
#108174 = AXIS2_PLACEMENT_3D ( 'NONE', #44657, #6618, #104211 ) ;
#108175 = CARTESIAN_POINT ( 'NONE',  ( 104.0348890100390946, 8.147879001971702451, 3.062904332527759621 ) ) ;
#108176 = CARTESIAN_POINT ( 'NONE',  ( -8.100000000000013856, 2.500000000000000000, -3.883716857408426648 ) ) ;
#108177 = DIRECTION ( 'NONE',  ( -4.274815082592931898E-19, -0.9999939076577903929, -0.003490651415223739937 ) ) ;
#108178 = DIRECTION ( 'NONE',  ( 0.000000000000000000, 0.000000000000000000, -1.000000000000000000 ) ) ;
#108179 = CIRCLE ( 'NONE', #7546, 0.1000000000000000056 ) ;
#108181 = EDGE_CURVE ( 'NONE', #65792, #86833, #96646, .T. ) ;
#108180 = CIRCLE ( 'NONE', #47570, 0.1000000000000002554 ) ;
#108182 = EDGE_LOOP ( 'NONE', ( #97236, #61100 ) ) ;
#108183 = ORIENTED_EDGE ( 'NONE', *, *, #128649, .F. ) ;
#108184 = VERTEX_POINT ( 'NONE', #10702 ) ;
#108185 = VERTEX_POINT ( 'NONE', #80779 ) ;
#108186 = DIRECTION ( 'NONE',  ( 0.000000000000000000, 0.000000000000000000, -1.000000000000000000 ) ) ;
#108187 = DIRECTION ( 'NONE',  ( -4.274815082592931898E-19, -0.9999939076577903929, -0.003490651415223739937 ) ) ;
#108188 = DIRECTION ( 'NONE',  ( 0.000000000000000000, 0.000000000000000000, 1.000000000000000000 ) ) ;
#108189 = VERTEX_POINT ( 'NONE', #99124 ) ;
#108190 = EDGE_CURVE ( 'NONE', #56111, #40454, #89292, .T. ) ;
#108191 = FACE_BOUND ( 'NONE', #48931, .T. ) ;
#108192 = EDGE_LOOP ( 'NONE', ( #22861, #4083 ) ) ;
#108193 = ADVANCED_FACE ( 'NONE', ( #41509 ), #67381, .T. ) ;
#108194 = DIRECTION ( 'NONE',  ( -0.000000000000000000, -1.000000000000000000, -0.000000000000000000 ) ) ;
#108195 = CARTESIAN_POINT ( 'NONE',  ( -8.750000000000010658, 12.50000000000000000, 2.857883832488649301 ) ) ;
#108196 = DIRECTION ( 'NONE',  ( 0.000000000000000000, 0.000000000000000000, 1.000000000000000000 ) ) ;
#108197 = CIRCLE ( 'NONE', #83088, 0.1000000000000002554 ) ;
#108198 = DIRECTION ( 'NONE',  ( 0.000000000000000000, 1.000000000000000000, 0.000000000000000000 ) ) ;
#108199 = DIRECTION ( 'NONE',  ( -0.000000000000000000, -1.000000000000000000, -0.000000000000000000 ) ) ;
#108200 = CONICAL_SURFACE ( 'NONE', #28799, 0.1000000000000000472, 0.003490658503988666988 ) ;
#108201 = EDGE_CURVE ( 'NONE', #51148, #121928, #50655, .T. ) ;
#108202 = CARTESIAN_POINT ( 'NONE',  ( -6.700000000000016165, 2.500000000000000000, 4.230127018922196669 ) ) ;
#108203 = EDGE_CURVE ( 'NONE', #22700, #52514, #117566, .T. ) ;
#108204 = DIRECTION ( 'NONE',  ( -0.000000000000000000, -1.000000000000000000, -0.000000000000000000 ) ) ;
#108205 = CARTESIAN_POINT ( 'NONE',  ( 14.99999999999989342, 2.500000000000000000, -0.5928203230275541635 ) ) ;
#108206 = ADVANCED_FACE ( 'NONE', ( #70941 ), #78852, .T. ) ;
#108207 = DIRECTION ( 'NONE',  ( 0.000000000000000000, 0.000000000000000000, -1.000000000000000000 ) ) ;
#108208 = ADVANCED_FACE ( 'NONE', ( #31664 ), #21192, .T. ) ;
#108209 = AXIS2_PLACEMENT_3D ( 'NONE', #55275, #95196, #70546 ) ;
#108210 = VECTOR ( 'NONE', #51091, 1000.000000000000000 ) ;
#108211 = CARTESIAN_POINT ( 'NONE',  ( -2.500000000000032419, 2.500000000000000000, 0.7928203230275495672 ) ) ;
#108212 = ORIENTED_EDGE ( 'NONE', *, *, #31810, .F. ) ;
#108214 = ORIENTED_EDGE ( 'NONE', *, *, #73862, .F. ) ;
#108213 = CIRCLE ( 'NONE', #14109, 0.1000000000000000472 ) ;
#108215 = EDGE_LOOP ( 'NONE', ( #7257, #16357 ) ) ;
#108216 = ORIENTED_EDGE ( 'NONE', *, *, #72482, .F. ) ;
#108217 = CARTESIAN_POINT ( 'NONE',  ( 17.50011901588668906, -2.224285231025419307, -4.071013062218297840 ) ) ;
#108218 = DIRECTION ( 'NONE',  ( -0.000000000000000000, 1.000000000000000000, -0.000000000000000000 ) ) ;
#108220 = EDGE_LOOP ( 'NONE', ( #103212, #24168, #104660, #101720 ) ) ;
#108219 = ORIENTED_EDGE ( 'NONE', *, *, #115899, .T. ) ;
#108221 = EDGE_CURVE ( 'NONE', #120555, #37733, #29765, .T. ) ;
#108223 = ORIENTED_EDGE ( 'NONE', *, *, #83031, .T. ) ;
#108222 = VECTOR ( 'NONE', #80042, 1000.000000000000000 ) ;
#108225 = AXIS2_PLACEMENT_3D ( 'NONE', #78282, #90657, #8222 ) ;
#108224 = DIRECTION ( 'NONE',  ( 0.000000000000000000, 1.000000000000000000, 0.000000000000000000 ) ) ;
#108226 = AXIS2_PLACEMENT_3D ( 'NONE', #66611, #67901, #96074 ) ;
#108227 = DIRECTION ( 'NONE',  ( 0.000000000000000000, -0.000000000000000000, 1.000000000000000000 ) ) ;
#108228 = CARTESIAN_POINT ( 'NONE',  ( 185.9583333333333144, 4.445597072760159030, 7.699999999999928235 ) ) ;
#108229 = FACE_OUTER_BOUND ( 'NONE', #80656, .T. ) ;
#108230 = DIRECTION ( 'NONE',  ( 0.000000000000000000, -0.9999939076577903929, 0.003490651415223739937 ) ) ;
#108231 = DIRECTION ( 'NONE',  ( 0.000000000000000000, 0.000000000000000000, 1.000000000000000000 ) ) ;
#108232 = DIRECTION ( 'NONE',  ( 0.000000000000000000, 1.000000000000000000, 0.000000000000000000 ) ) ;
#108233 = AXIS2_PLACEMENT_3D ( 'NONE', #127403, #126764, #37735 ) ;
#108234 = VERTEX_POINT ( 'NONE', #69650 ) ;
#108235 = DIRECTION ( 'NONE',  ( 0.000000000000000000, 1.000000000000000000, 0.000000000000000000 ) ) ;
#108236 = VERTEX_POINT ( 'NONE', #118747 ) ;
#108238 = CONICAL_SURFACE ( 'NONE', #122920, 0.1000000000000000056, 0.003490658503988666988 ) ;
#108237 = CIRCLE ( 'NONE', #68519, 0.09999999999999982514 ) ;
#108239 = VERTEX_POINT ( 'NONE', #71582 ) ;
#108240 = ORIENTED_EDGE ( 'NONE', *, *, #41875, .F. ) ;
#108241 = LINE ( 'NONE', #68962, #98483 ) ;
#108242 = ORIENTED_EDGE ( 'NONE', *, *, #16732, .T. ) ;
#108243 = ORIENTED_EDGE ( 'NONE', *, *, #91001, .F. ) ;
#108244 = CARTESIAN_POINT ( 'NONE',  ( 2.299999999999947864, 12.50000000000000000, 4.048810130592458201 ) ) ;
#108245 = CARTESIAN_POINT ( 'NONE',  ( 5.849999999999933920, 2.500000000000000000, -2.857883832488653741 ) ) ;
#108246 = DIRECTION ( 'NONE',  ( 0.000000000000000000, 1.000000000000000000, 0.000000000000000000 ) ) ;
#108247 = DIRECTION ( 'NONE',  ( -0.000000000000000000, -1.000000000000000000, -0.000000000000000000 ) ) ;
#108248 = CARTESIAN_POINT ( 'NONE',  ( -8.950000000000009948, 2.500000000000000000, 2.511473670974873507 ) ) ;
#108249 = ADVANCED_FACE ( 'NONE', ( #89927 ), #19286, .T. ) ;
#108250 = ORIENTED_EDGE ( 'NONE', *, *, #25982, .T. ) ;
#108251 = EDGE_CURVE ( 'NONE', #122621, #13831, #109170, .T. ) ;
#108252 = CARTESIAN_POINT ( 'NONE',  ( -10.85000000000000142, 2.500000000000000000, -6.495190528383298911 ) ) ;
#108253 = EDGE_LOOP ( 'NONE', ( #87764, #23984, #77855, #59515 ) ) ;
#108255 = EDGE_CURVE ( 'NONE', #125293, #61342, #54894, .T. ) ;
#108254 = CARTESIAN_POINT ( 'NONE',  ( 16.56034314470449686, 0.8287381876616523035, 6.090234461610898542 ) ) ;
#108256 = ORIENTED_EDGE ( 'NONE', *, *, #68032, .T. ) ;
#108257 = CARTESIAN_POINT ( 'NONE',  ( 112.3243458019354648, 8.328603270140316539, -2.530626142253337374 ) ) ;
#108258 = DIRECTION ( 'NONE',  ( 0.000000000000000000, 0.000000000000000000, -1.000000000000000000 ) ) ;
#108259 = ORIENTED_EDGE ( 'NONE', *, *, #119262, .T. ) ;
#108261 = AXIS2_PLACEMENT_3D ( 'NONE', #43042, #100625, #2416 ) ;
#108260 = LINE ( 'NONE', #78828, #71833 ) ;
#108262 = EDGE_CURVE ( 'NONE', #45293, #24007, #88649, .T. ) ;
#108263 = FACE_OUTER_BOUND ( 'NONE', #86277, .T. ) ;
#108264 = EDGE_LOOP ( 'NONE', ( #109394, #105336, #22720, #49685 ) ) ;
#108265 = ADVANCED_FACE ( 'NONE', ( #40200 ), #93175, .T. ) ;
#108267 = ADVANCED_FACE ( 'NONE', ( #74170 ), #12647, .T. ) ;
#108266 = AXIS2_PLACEMENT_3D ( 'NONE', #37427, #28241, #68803 ) ;
#108268 = CIRCLE ( 'NONE', #51842, 0.1000000000000002554 ) ;
#108269 = ADVANCED_FACE ( 'NONE', ( #94434 ), #94596, .T. ) ;
#108270 = CARTESIAN_POINT ( 'NONE',  ( 4.149999999999939959, 2.500000000000000000, -6.395190528383301931 ) ) ;
#108271 = EDGE_LOOP ( 'NONE', ( #117141, #77168 ) ) ;
#108272 = ORIENTED_EDGE ( 'NONE', *, *, #68196, .F. ) ;
#108273 = CARTESIAN_POINT ( 'NONE',  ( 11.44999999999990870, 2.500000000000000000, -1.818653347947326138 ) ) ;
#108274 = CARTESIAN_POINT ( 'NONE',  ( -13.14999999999999147, 12.50000000000000000, -1.818653347947323917 ) ) ;
#108275 = CARTESIAN_POINT ( 'NONE',  ( 186.3802083336747444, 4.367472073101515306, 7.564683531250000925 ) ) ;
#108276 = PLANE ( 'NONE',  #126505 ) ;
#108277 = ADVANCED_FACE ( 'NONE', ( #113440 ), #64342, .T. ) ;
#108278 = VECTOR ( 'NONE', #33419, 1000.000000000000000 ) ;
#108279 = DIRECTION ( 'NONE',  ( -4.274815082592931898E-19, -0.9999939076577903929, -0.003490651415223739937 ) ) ;
#108280 = CIRCLE ( 'NONE', #76979, 0.1000000000000002554 ) ;
#108281 = ORIENTED_EDGE ( 'NONE', *, *, #86781, .T. ) ;
#108282 = DIRECTION ( 'NONE',  ( -0.000000000000000000, 1.000000000000000000, -0.000000000000000000 ) ) ;
#108284 = AXIS2_PLACEMENT_3D ( 'NONE', #107394, #126396, #77931 ) ;
#108283 = CARTESIAN_POINT ( 'NONE',  ( 4.149999999999936406, 2.500000000000000000, 6.595190528383296780 ) ) ;
#108285 = EDGE_LOOP ( 'NONE', ( #25208, #119738 ) ) ;
#108286 = AXIS2_PLACEMENT_3D ( 'NONE', #17285, #87329, #109570 ) ;
#108287 = FACE_OUTER_BOUND ( 'NONE', #20712, .T. ) ;
#108288 = FACE_OUTER_BOUND ( 'NONE', #110137, .T. ) ;
#108289 = DIRECTION ( 'NONE',  ( 0.000000000000000000, -0.000000000000000000, 1.000000000000000000 ) ) ;
#108290 = PLANE ( 'NONE',  #16634 ) ;
#108291 = PLANE ( 'NONE',  #51668 ) ;
#108292 = ORIENTED_EDGE ( 'NONE', *, *, #89684, .T. ) ;
#108293 = AXIS2_PLACEMENT_3D ( 'NONE', #90119, #77724, #29301 ) ;
#108294 = CARTESIAN_POINT ( 'NONE',  ( 1.649999999999951505, 12.50000000000000000, 2.857883832488649301 ) ) ;
#108295 = DIRECTION ( 'NONE',  ( 0.000000000000000000, -0.9999939076577903929, 0.003490651415223739937 ) ) ;
#108296 = AXIS2_PLACEMENT_3D ( 'NONE', #10644, #90516, #80718 ) ;
#108297 = AXIS2_PLACEMENT_3D ( 'NONE', #11324, #40810, #68953 ) ;
#108298 = VERTEX_POINT ( 'NONE', #14579 ) ;
#108299 = LINE ( 'NONE', #86729, #94892 ) ;
#108300 = AXIS2_PLACEMENT_3D ( 'NONE', #68213, #57769, #38122 ) ;
#108301 = ADVANCED_FACE ( 'NONE', ( #43439 ), #119640, .T. ) ;
#108302 = EDGE_LOOP ( 'NONE', ( #111771, #119314, #21292, #43536 ) ) ;
#108303 = ORIENTED_EDGE ( 'NONE', *, *, #121527, .T. ) ;
#108304 = DIRECTION ( 'NONE',  ( 0.000000000000000000, 0.000000000000000000, 1.000000000000000000 ) ) ;
#108305 = CONICAL_SURFACE ( 'NONE', #95793, 0.1000000000000000472, 0.003490658503988666988 ) ;
#108306 = ORIENTED_EDGE ( 'NONE', *, *, #28324, .F. ) ;
#108307 = PLANE ( 'NONE',  #125973 ) ;
#108308 = PLANE ( 'NONE',  #102823 ) ;
#108309 = CARTESIAN_POINT ( 'NONE',  ( 4.399999999999940847, 2.500000000000000000, -3.983716857408426293 ) ) ;
#108310 = ORIENTED_EDGE ( 'NONE', *, *, #109888, .T. ) ;
#108311 = CARTESIAN_POINT ( 'NONE',  ( -11.89999999999999680, 2.500000000000000000, -4.676537180435976104 ) ) ;
#108313 = EDGE_LOOP ( 'NONE', ( #6488, #13697, #3515, #19024 ) ) ;
#108312 = DIRECTION ( 'NONE',  ( 0.000000000000000000, -0.9999939076577903929, 0.003490651415223739937 ) ) ;
#108314 = CARTESIAN_POINT ( 'NONE',  ( 12.09999999999990550, 12.50000000000000000, -5.022947341949754119 ) ) ;
#108315 = CIRCLE ( 'NONE', #129280, 0.1000000000000002554 ) ;
#108316 = ADVANCED_FACE ( 'NONE', ( #63708 ), #3491, .T. ) ;
#108317 = PLANE ( 'NONE',  #124113 ) ;
#108318 = ORIENTED_EDGE ( 'NONE', *, *, #75131, .F. ) ;
#108320 = AXIS2_PLACEMENT_3D ( 'NONE', #91087, #49894, #10573 ) ;
#108319 = AXIS2_PLACEMENT_3D ( 'NONE', #61434, #68162, #108085 ) ;
#108321 = ORIENTED_EDGE ( 'NONE', *, *, #12659, .T. ) ;
#108322 = ORIENTED_EDGE ( 'NONE', *, *, #10963, .F. ) ;
#108323 = DIRECTION ( 'NONE',  ( -0.000000000000000000, 1.000000000000000000, -0.000000000000000000 ) ) ;
#108324 = CARTESIAN_POINT ( 'NONE',  ( 10.39999999999991154, 2.500000000000000000, 5.022947341949748790 ) ) ;
#108325 = DIRECTION ( 'NONE',  ( 0.000000000000000000, 1.000000000000000000, 0.000000000000000000 ) ) ;
#108326 = FACE_BOUND ( 'NONE', #112763, .T. ) ;
#108327 = EDGE_LOOP ( 'NONE', ( #43386, #51734 ) ) ;
#108328 = DIRECTION ( 'NONE',  ( -0.000000000000000000, 1.000000000000000000, -0.000000000000000000 ) ) ;
#108329 = DIRECTION ( 'NONE',  ( 0.000000000000000000, 0.000000000000000000, 1.000000000000000000 ) ) ;
#108330 = VERTEX_POINT ( 'NONE', #92506 ) ;
#108331 = LINE ( 'NONE', #58606, #123902 ) ;
#108332 = DIRECTION ( 'NONE',  ( -4.274815082592931898E-19, -0.9999939076577903929, -0.003490651415223739937 ) ) ;
#108333 = DIRECTION ( 'NONE',  ( -4.274815082592931898E-19, -0.9999939076577903929, -0.003490651415223739937 ) ) ;
#108334 = DIRECTION ( 'NONE',  ( -0.000000000000000000, -1.000000000000000000, -0.000000000000000000 ) ) ;
#108335 = CONICAL_SURFACE ( 'NONE', #10147, 0.1000000000000002554, 0.003490658503988666988 ) ;
#108336 = CARTESIAN_POINT ( 'NONE',  ( -6.700000000000019718, 2.500000000000000000, -4.430127018922202176 ) ) ;
#108337 = CARTESIAN_POINT ( 'NONE',  ( -5.200000000000024158, 12.50000000000000000, -4.676537180435977881 ) ) ;
#108338 = DIRECTION ( 'NONE',  ( -4.274815082592931898E-19, -0.9999939076577903929, -0.003490651415223739937 ) ) ;
#108339 = CIRCLE ( 'NONE', #70785, 0.1000000000000000472 ) ;
#108340 = ADVANCED_FACE ( 'NONE', ( #22509 ), #102344, .T. ) ;
#108341 = ORIENTED_EDGE ( 'NONE', *, *, #8610, .T. ) ;
#108342 = ORIENTED_EDGE ( 'NONE', *, *, #51647, .F. ) ;
#108343 = ORIENTED_EDGE ( 'NONE', *, *, #119114, .F. ) ;
#108344 = CIRCLE ( 'NONE', #51934, 0.09999999999999982514 ) ;
#108345 = EDGE_LOOP ( 'NONE', ( #206, #77796, #116321, #127521 ) ) ;
#108346 = EDGE_LOOP ( 'NONE', ( #69632, #33488 ) ) ;
#108347 = CARTESIAN_POINT ( 'NONE',  ( 8.349999999999923261, 2.500000000000000000, 2.857883832488649301 ) ) ;
#108348 = DIRECTION ( 'NONE',  ( 0.000000000000000000, 0.000000000000000000, 1.000000000000000000 ) ) ;
#108349 = EDGE_LOOP ( 'NONE', ( #104045, #95755, #113700, #4072 ) ) ;
#108350 = FACE_BOUND ( 'NONE', #2871, .T. ) ;
#108351 = EDGE_CURVE ( 'NONE', #80116, #118274, #79940, .T. ) ;
#108352 = CARTESIAN_POINT ( 'NONE',  ( 5.399999999999936406, 2.500000000000000000, -3.737306695894649700 ) ) ;
#108353 = AXIS2_PLACEMENT_3D ( 'NONE', #81508, #44645, #1638 ) ;
#108354 = VECTOR ( 'NONE', #30187, 1000.000000000000000 ) ;
#108355 = CONICAL_SURFACE ( 'NONE', #87420, 0.09999999999999982514, 0.003490658503988666988 ) ;
#108356 = CARTESIAN_POINT ( 'NONE',  ( -0.8500000000000386136, 12.50000000000000000, 5.802370205355744659 ) ) ;
#108357 = EDGE_CURVE ( 'NONE', #115280, #60931, #31926, .T. ) ;
#108358 = FACE_OUTER_BOUND ( 'NONE', #102991, .T. ) ;
#108359 = EDGE_CURVE ( 'NONE', #40017, #71388, #124562, .T. ) ;
#108360 = LINE ( 'NONE', #118183, #17778 ) ;
#108361 = ADVANCED_FACE ( 'NONE', ( #121982 ), #13292, .T. ) ;
#108362 = CARTESIAN_POINT ( 'NONE',  ( -5.400000000000019895, 12.50000000000000000, 3.572213422710607489 ) ) ;
#108363 = EDGE_CURVE ( 'NONE', #62955, #112193, #56931, .T. ) ;
#108364 = ORIENTED_EDGE ( 'NONE', *, *, #95842, .F. ) ;
#108365 = ORIENTED_EDGE ( 'NONE', *, *, #42193, .F. ) ;
#108366 = AXIS2_PLACEMENT_3D ( 'NONE', #10398, #90232, #88296 ) ;
#108367 = VERTEX_POINT ( 'NONE', #62426 ) ;
#108368 = ORIENTED_EDGE ( 'NONE', *, *, #117101, .T. ) ;
#108369 = PLANE ( 'NONE',  #58944 ) ;
#108370 = CARTESIAN_POINT ( 'NONE',  ( 13.91976764350745555, 2.499999999999999556, 6.779443706236890854 ) ) ;
#108371 = CARTESIAN_POINT ( 'NONE',  ( -13.94999999999998863, 12.50000000000000000, 2.511473670974877503 ) ) ;
#108372 = ORIENTED_EDGE ( 'NONE', *, *, #115908, .F. ) ;
#108373 = EDGE_CURVE ( 'NONE', #104314, #43021, #54508, .T. ) ;
#108374 = LINE ( 'NONE', #97905, #120761 ) ;
#108375 = ADVANCED_FACE ( 'NONE', ( #114090 ), #101698, .T. ) ;
#108376 = CIRCLE ( 'NONE', #28973, 0.06509327318403745899 ) ;
#108377 = DIRECTION ( 'NONE',  ( 0.000000000000000000, 0.000000000000000000, 1.000000000000000000 ) ) ;
#108378 = ADVANCED_FACE ( 'NONE', ( #23127 ), #80039, .T. ) ;
#108379 = CARTESIAN_POINT ( 'NONE',  ( 8.349999999999923261, 12.50000000000000000, 2.165063509461097713 ) ) ;
#108380 = CARTESIAN_POINT ( 'NONE',  ( 185.3593750003413732, 0.000000000000000000, 7.564683531250000925 ) ) ;
#108381 = DIRECTION ( 'NONE',  ( -0.000000000000000000, 1.000000000000000000, -0.000000000000000000 ) ) ;
#108382 = CARTESIAN_POINT ( 'NONE',  ( -8.750000000000007105, 2.500000000000000000, 7.088010851410848190 ) ) ;
#108383 = AXIS2_PLACEMENT_3D ( 'NONE', #75426, #93800, #106197 ) ;
#108384 = CARTESIAN_POINT ( 'NONE',  ( -2.100000000000034728, 2.500000000000000000, 4.430127018922196847 ) ) ;
#108385 = ORIENTED_EDGE ( 'NONE', *, *, #95642, .F. ) ;
#108386 = DIRECTION ( 'NONE',  ( 0.000000000000000000, 0.000000000000000000, -1.000000000000000000 ) ) ;
#108387 = VECTOR ( 'NONE', #124213, 1000.000000000000000 ) ;
#108388 = VERTEX_POINT ( 'NONE', #47292 ) ;
#108389 = VERTEX_POINT ( 'NONE', #78027 ) ;
#108390 = DIRECTION ( 'NONE',  ( 0.000000000000000000, 0.000000000000000000, 1.000000000000000000 ) ) ;
#108391 = DIRECTION ( 'NONE',  ( 0.000000000000000000, 0.000000000000000000, 1.000000000000000000 ) ) ;
#108392 = DIRECTION ( 'NONE',  ( 0.000000000000000000, 0.000000000000000000, -1.000000000000000000 ) ) ;
#108393 = ORIENTED_EDGE ( 'NONE', *, *, #50795, .T. ) ;
#108394 = CONICAL_SURFACE ( 'NONE', #22741, 0.1000000000000002554, 0.003490658503988666988 ) ;
#108395 = ORIENTED_EDGE ( 'NONE', *, *, #22714, .T. ) ;
#108396 = DIRECTION ( 'NONE',  ( 0.000000000000000000, 0.000000000000000000, -1.000000000000000000 ) ) ;
#108397 = CIRCLE ( 'NONE', #31063, 0.06509327318403745899 ) ;
#108398 = DIRECTION ( 'NONE',  ( 0.000000000000000000, -0.000000000000000000, 1.000000000000000000 ) ) ;
#108399 = CARTESIAN_POINT ( 'NONE',  ( -5.600000000000023626, 12.50000000000000000, -3.983716857408426293 ) ) ;
#108400 = EDGE_LOOP ( 'NONE', ( #43373, #48407, #90549, #76727 ) ) ;
#108401 = ORIENTED_EDGE ( 'NONE', *, *, #22219, .T. ) ;
#108402 = DIRECTION ( 'NONE',  ( 0.000000000000000000, -0.000000000000000000, 1.000000000000000000 ) ) ;
#108403 = ORIENTED_EDGE ( 'NONE', *, *, #129330, .F. ) ;
#108404 = FACE_OUTER_BOUND ( 'NONE', #34277, .T. ) ;
#108405 = ORIENTED_EDGE ( 'NONE', *, *, #37873, .T. ) ;
#108406 = DIRECTION ( 'NONE',  ( -0.000000000000000000, -1.000000000000000000, -0.000000000000000000 ) ) ;
#108407 = LINE ( 'NONE', #18741, #75476 ) ;
#108408 = DIRECTION ( 'NONE',  ( 0.000000000000000000, 0.000000000000000000, -1.000000000000000000 ) ) ;
#108409 = CONICAL_SURFACE ( 'NONE', #22759, 0.1000000000000002554, 0.003490658503988666988 ) ;
#108410 = EDGE_CURVE ( 'NONE', #33730, #114232, #109276, .T. ) ;
#108411 = DIRECTION ( 'NONE',  ( 0.000000000000000000, 0.000000000000000000, 1.000000000000000000 ) ) ;
#108412 = ORIENTED_EDGE ( 'NONE', *, *, #104064, .T. ) ;
#108413 = EDGE_CURVE ( 'NONE', #89818, #56893, #76744, .T. ) ;
#108414 = CARTESIAN_POINT ( 'NONE',  ( 2.099999999999950351, 2.500000000000000000, -4.330127018922201643 ) ) ;
#108416 = CIRCLE ( 'NONE', #51995, 0.09999999999999999167 ) ;
#108415 = CIRCLE ( 'NONE', #104217, 0.06509327318403745899 ) ;
#108417 = EDGE_CURVE ( 'NONE', #10886, #118566, #15876, .T. ) ;
#108418 = ORIENTED_EDGE ( 'NONE', *, *, #108993, .F. ) ;
#108419 = VERTEX_POINT ( 'NONE', #97024 ) ;
#108420 = DIRECTION ( 'NONE',  ( 0.000000000000000000, 0.000000000000000000, 1.000000000000000000 ) ) ;
#108421 = CARTESIAN_POINT ( 'NONE',  ( -10.40000000000000213, 12.50000000000000000, 4.395220292106234439 ) ) ;
#108422 = DIRECTION ( 'NONE',  ( -4.274815082592931898E-19, -0.9999939076577903929, -0.003490651415223739937 ) ) ;
#108423 = FACE_OUTER_BOUND ( 'NONE', #38065, .T. ) ;
#108424 = DIRECTION ( 'NONE',  ( 0.000000000000000000, 0.000000000000000000, -1.000000000000000000 ) ) ;
#108425 = ADVANCED_FACE ( 'NONE', ( #55173 ), #82191, .T. ) ;
#108426 = CARTESIAN_POINT ( 'NONE',  ( 11.64999999999990798, 12.50000000000000000, 7.253104124594885960 ) ) ;
#108427 = CARTESIAN_POINT ( 'NONE',  ( 17.99892161670943125, 2.500000000000000444, -4.934975022999350536 ) ) ;
#108428 = LINE ( 'NONE', #10240, #42839 ) ;
#108429 = DIRECTION ( 'NONE',  ( 0.000000000000000000, 0.000000000000000000, 1.000000000000000000 ) ) ;
#108430 = FACE_OUTER_BOUND ( 'NONE', #122470, .T. ) ;
#108431 = AXIS2_PLACEMENT_3D ( 'NONE', #70926, #129228, #892 ) ;
#108432 = ORIENTED_EDGE ( 'NONE', *, *, #56839, .T. ) ;
#108433 = AXIS2_PLACEMENT_3D ( 'NONE', #10986, #43077, #33246 ) ;
#108434 = FACE_OUTER_BOUND ( 'NONE', #27721, .T. ) ;
#108435 = LINE ( 'NONE', #77680, #12410 ) ;
#108436 = LINE ( 'NONE', #22660, #97637 ) ;
#108437 = EDGE_CURVE ( 'NONE', #87221, #108784, #119737, .T. ) ;
#108438 = CARTESIAN_POINT ( 'NONE',  ( 154.1524742528378056, 2.500000000000000000, 1.703575533167231537 ) ) ;
#108439 = DIRECTION ( 'NONE',  ( -0.000000000000000000, -1.000000000000000000, -0.000000000000000000 ) ) ;
#108440 = CONICAL_SURFACE ( 'NONE', #26986, 0.1000000000000002554, 0.003490658503988666988 ) ;
#108441 = ORIENTED_EDGE ( 'NONE', *, *, #42967, .F. ) ;
#108442 = CIRCLE ( 'NONE', #29052, 0.1000000000000002554 ) ;
#108443 = CARTESIAN_POINT ( 'NONE',  ( -2.100000000000033396, 2.500000000000000000, -5.022947341949754119 ) ) ;
#108444 = VECTOR ( 'NONE', #8264, 1000.000000000000000 ) ;
#108445 = CARTESIAN_POINT ( 'NONE',  ( 5.449999999999936229, 12.50000000000000000, 6.560283801567334372 ) ) ;
#108447 = ORIENTED_EDGE ( 'NONE', *, *, #51437, .T. ) ;
#108446 = DIRECTION ( 'NONE',  ( 0.000000000000000000, 1.000000000000000000, 0.000000000000000000 ) ) ;
#108448 = AXIS2_PLACEMENT_3D ( 'NONE', #94630, #23312, #54696 ) ;
#108449 = ORIENTED_EDGE ( 'NONE', *, *, #112931, .F. ) ;
#108450 = DIRECTION ( 'NONE',  ( 0.000000000000000000, 0.000000000000000000, 1.000000000000000000 ) ) ;
#108451 = CONICAL_SURFACE ( 'NONE', #2028, 0.1000000000000002554, 0.003490658503988666988 ) ;
#108453 = VERTEX_POINT ( 'NONE', #25062 ) ;
#108452 = EDGE_CURVE ( 'NONE', #62906, #69160, #23598, .T. ) ;
#108454 = ORIENTED_EDGE ( 'NONE', *, *, #72646, .F. ) ;
#108455 = ORIENTED_EDGE ( 'NONE', *, *, #117257, .F. ) ;
#108456 = DIRECTION ( 'NONE',  ( -0.000000000000000000, -1.000000000000000000, -0.000000000000000000 ) ) ;
#108457 = EDGE_CURVE ( 'NONE', #112742, #109968, #52850, .T. ) ;
#108458 = CARTESIAN_POINT ( 'NONE',  ( 4.349999999999941025, 2.500000000000000000, -1.718653347947326049 ) ) ;
#108459 = CARTESIAN_POINT ( 'NONE',  ( -11.24999999999996270, 12.50000000000000000, 2.165063509461097713 ) ) ;
#108460 = CARTESIAN_POINT ( 'NONE',  ( -11.64999999999999680, 2.500000000000000000, -7.088010851410849966 ) ) ;
#108461 = AXIS2_PLACEMENT_3D ( 'NONE', #46728, #94529, #96450 ) ;
#108462 = EDGE_LOOP ( 'NONE', ( #52999, #59455 ) ) ;
#108463 = FACE_OUTER_BOUND ( 'NONE', #72965, .T. ) ;
#108464 = ORIENTED_EDGE ( 'NONE', *, *, #68620, .T. ) ;
#108465 = AXIS2_PLACEMENT_3D ( 'NONE', #88465, #128433, #39410 ) ;
#108466 = CARTESIAN_POINT ( 'NONE',  ( -4.400000000000025224, 2.500000000000000000, 3.983716857408420076 ) ) ;
#108467 = CARTESIAN_POINT ( 'NONE',  ( 21.24754738303277080, -0.7337760880902398641, -4.182111650399356506 ) ) ;
#108468 = FACE_OUTER_BOUND ( 'NONE', #18371, .T. ) ;
#108469 = DIRECTION ( 'NONE',  ( 0.000000000000000000, 0.000000000000000000, 1.000000000000000000 ) ) ;
#108470 = ADVANCED_FACE ( 'NONE', ( #75439 ), #2760, .T. ) ;
#108471 = DIRECTION ( 'NONE',  ( -0.000000000000000000, -1.000000000000000000, -0.000000000000000000 ) ) ;
#108472 = ORIENTED_EDGE ( 'NONE', *, *, #94092, .F. ) ;
#108473 = CIRCLE ( 'NONE', #89702, 0.09999999999999982514 ) ;
#108474 = ORIENTED_EDGE ( 'NONE', *, *, #41722, .F. ) ;
#108475 = ORIENTED_EDGE ( 'NONE', *, *, #73353, .T. ) ;
#108476 = ORIENTED_EDGE ( 'NONE', *, *, #105591, .T. ) ;
#108477 = EDGE_LOOP ( 'NONE', ( #18161, #65425 ) ) ;
#108478 = CARTESIAN_POINT ( 'NONE',  ( -1.250000000000037526, 12.50000000000000000, -1.472243186433550122 ) ) ;
#108479 = LINE ( 'NONE', #28654, #68659 ) ;
#108480 = ADVANCED_FACE ( 'NONE', ( #95742 ), #13115, .T. ) ;
#108481 = DIRECTION ( 'NONE',  ( -0.000000000000000000, -1.000000000000000000, -0.000000000000000000 ) ) ;
#108482 = FACE_BOUND ( 'NONE', #68942, .T. ) ;
#108483 = DIRECTION ( 'NONE',  ( 0.000000000000000000, 0.000000000000000000, 1.000000000000000000 ) ) ;
#108484 = CARTESIAN_POINT ( 'NONE',  ( 3.949999999999942446, 2.500000000000000000, -2.511473670974877948 ) ) ;
#108485 = CIRCLE ( 'NONE', #52070, 0.1000000000000000056 ) ;
#108486 = DIRECTION ( 'NONE',  ( 0.000000000000000000, -0.9999939076577903929, 0.003490651415223739937 ) ) ;
#108487 = CARTESIAN_POINT ( 'NONE',  ( 0.7999999999999553024, 2.500000000000000000, -4.330127018922201643 ) ) ;
#108488 = AXIS2_PLACEMENT_3D ( 'NONE', #55664, #95597, #5899 ) ;
#108489 = CARTESIAN_POINT ( 'NONE',  ( 186.0052083336747444, -6.551208109652278289, 3.782341765624995134 ) ) ;
#108490 = DIRECTION ( 'NONE',  ( 0.000000000000000000, 1.000000000000000000, 0.000000000000000000 ) ) ;
#108491 = AXIS2_PLACEMENT_3D ( 'NONE', #93264, #3586, #43533 ) ;
#108492 = CARTESIAN_POINT ( 'NONE',  ( -12.49999999999999289, 12.50000000000000000, 5.088040615133786027 ) ) ;
#108493 = FACE_OUTER_BOUND ( 'NONE', #75367, .T. ) ;
#108494 = ADVANCED_FACE ( 'NONE', ( #125827 ), #7341, .T. ) ;
#108496 = AXIS2_PLACEMENT_3D ( 'NONE', #64697, #94808, #35259 ) ;
#108495 = AXIS2_PLACEMENT_3D ( 'NONE', #43270, #93641, #71401 ) ;
#108497 = ORIENTED_EDGE ( 'NONE', *, *, #23495, .F. ) ;
#108498 = VERTEX_POINT ( 'NONE', #16510 ) ;
#108499 = VERTEX_POINT ( 'NONE', #95100 ) ;
#108500 = VERTEX_POINT ( 'NONE', #87191 ) ;
#108501 = CARTESIAN_POINT ( 'NONE',  ( 10.44999999999991402, 2.500000000000000000, -2.265063509461101798 ) ) ;
#108502 = AXIS2_PLACEMENT_3D ( 'NONE', #110291, #40937, #78921 ) ;
#108503 = DIRECTION ( 'NONE',  ( 0.000000000000000000, 1.000000000000000000, 0.000000000000000000 ) ) ;
#108504 = FACE_BOUND ( 'NONE', #68752, .T. ) ;
#108505 = DIRECTION ( 'NONE',  ( -0.000000000000000000, -1.000000000000000000, -0.000000000000000000 ) ) ;
#108506 = EDGE_CURVE ( 'NONE', #45092, #31883, #71722, .T. ) ;
#108507 = AXIS2_PLACEMENT_3D ( 'NONE', #81695, #50313, #90213 ) ;
#108508 = VERTEX_POINT ( 'NONE', #27619 ) ;
#108509 = ADVANCED_FACE ( 'NONE', ( #107494 ), #96742, .T. ) ;
#108510 = DIRECTION ( 'NONE',  ( -0.000000000000000000, 1.000000000000000000, -0.000000000000000000 ) ) ;
#108511 = CARTESIAN_POINT ( 'NONE',  ( -12.49999999999999467, 2.500000000000000000, -3.637306695894647390 ) ) ;
#108512 = EDGE_CURVE ( 'NONE', #8819, #83265, #9011, .T. ) ;
#108513 = CARTESIAN_POINT ( 'NONE',  ( 3.749999999999944045, 2.500000000000000000, -7.188010851410854052 ) ) ;
#108514 = EDGE_CURVE ( 'NONE', #62002, #119406, #117274, .T. ) ;
#108515 = CARTESIAN_POINT ( 'NONE',  ( -9.800000000000007816, 2.500000000000000000, -3.983716857408421852 ) ) ;
#108516 = ADVANCED_FACE ( 'NONE', ( #7986 ), #75918, .T. ) ;
#108517 = EDGE_LOOP ( 'NONE', ( #26674, #4272 ) ) ;
#108518 = CARTESIAN_POINT ( 'NONE',  ( -6.650000000000019007, 2.500000000000000000, -1.372243186433550033 ) ) ;
#108519 = VERTEX_POINT ( 'NONE', #38112 ) ;
#108520 = ADVANCED_FACE ( 'NONE', ( #25701 ), #117658, .T. ) ;
#108521 = EDGE_LOOP ( 'NONE', ( #45622, #50475 ) ) ;
#108522 = AXIS2_PLACEMENT_3D ( 'NONE', #58480, #49956, #49312 ) ;
#108523 = DIRECTION ( 'NONE',  ( -0.000000000000000000, -1.000000000000000000, -0.000000000000000000 ) ) ;
#108524 = EDGE_CURVE ( 'NONE', #117711, #94609, #17437, .T. ) ;
#108525 = DIRECTION ( 'NONE',  ( 0.000000000000000000, 0.000000000000000000, 1.000000000000000000 ) ) ;
#108526 = ORIENTED_EDGE ( 'NONE', *, *, #54934, .F. ) ;
#108527 = EDGE_CURVE ( 'NONE', #77475, #90522, #29867, .T. ) ;
#108528 = EDGE_CURVE ( 'NONE', #54254, #74055, #98300, .T. ) ;
#108529 = CIRCLE ( 'NONE', #58379, 0.06509327318403745899 ) ;
#108530 = DIRECTION ( 'NONE',  ( 0.000000000000000000, -0.9999939076577903929, 0.003490651415223739937 ) ) ;
#108531 = EDGE_CURVE ( 'NONE', #108784, #87221, #88435, .T. ) ;
#108532 = AXIS2_PLACEMENT_3D ( 'NONE', #97486, #77834, #58852 ) ;
#108533 = CARTESIAN_POINT ( 'NONE',  ( 8.349999999999923261, 12.50000000000000000, 2.922977105672686982 ) ) ;
#108534 = VERTEX_POINT ( 'NONE', #30886 ) ;
#108535 = CARTESIAN_POINT ( 'NONE',  ( -6.900000000000015454, 12.50000000000000000, 4.741630453620009789 ) ) ;
#108536 = ORIENTED_EDGE ( 'NONE', *, *, #116320, .T. ) ;
#108537 = CARTESIAN_POINT ( 'NONE',  ( 4.999999999999969802, 2.500000000000000000, 4.330127018922196314 ) ) ;
#108538 = EDGE_CURVE ( 'NONE', #16823, #32813, #51162, .T. ) ;
#108540 = ORIENTED_EDGE ( 'NONE', *, *, #97120, .F. ) ;
#108539 = VECTOR ( 'NONE', #58552, 1000.000000000000227 ) ;
#108541 = DIRECTION ( 'NONE',  ( -0.000000000000000000, 1.000000000000000000, -0.000000000000000000 ) ) ;
#108542 = FACE_BOUND ( 'NONE', #81140, .T. ) ;
#108543 = AXIS2_PLACEMENT_3D ( 'NONE', #70430, #118886, #61914 ) ;
#108544 = CIRCLE ( 'NONE', #12393, 0.09999999999999982514 ) ;
#108545 = ORIENTED_EDGE ( 'NONE', *, *, #59530, .T. ) ;
#108546 = CARTESIAN_POINT ( 'NONE',  ( 108.6775537376563534, 5.892458298213239409, 4.956757361901918735 ) ) ;
#108547 = VERTEX_POINT ( 'NONE', #70783 ) ;
#108548 = DIRECTION ( 'NONE',  ( 0.000000000000000000, -0.000000000000000000, 1.000000000000000000 ) ) ;
#108549 = DIRECTION ( 'NONE',  ( -0.000000000000000000, -1.000000000000000000, -0.000000000000000000 ) ) ;
#108550 = DIRECTION ( 'NONE',  ( 0.000000000000000000, 0.000000000000000000, 1.000000000000000000 ) ) ;
#108551 = DIRECTION ( 'NONE',  ( -4.274815082592931898E-19, -0.9999939076577903929, -0.003490651415223739937 ) ) ;
#108552 = CYLINDRICAL_SURFACE ( 'NONE', #62128, 3.000000000000000000 ) ;
#108553 = AXIS2_PLACEMENT_3D ( 'NONE', #124603, #95141, #123938 ) ;
#108554 = VERTEX_POINT ( 'NONE', #50495 ) ;
#108555 = ORIENTED_EDGE ( 'NONE', *, *, #73669, .T. ) ;
#108557 = EDGE_LOOP ( 'NONE', ( #7296, #117632 ) ) ;
#108556 = CIRCLE ( 'NONE', #43827, 0.06509327318403745899 ) ;
#108558 = LINE ( 'NONE', #107262, #60144 ) ;
#108559 = AXIS2_PLACEMENT_3D ( 'NONE', #38132, #37501, #38809 ) ;
#108560 = CARTESIAN_POINT ( 'NONE',  ( -12.09999999999999609, 12.50000000000000000, -0.06509327318403569651 ) ) ;
#108561 = DIRECTION ( 'NONE',  ( -4.274815082592931898E-19, -0.9999939076577903929, -0.003490651415223739937 ) ) ;
#108563 = ORIENTED_EDGE ( 'NONE', *, *, #59893, .F. ) ;
#108562 = VERTEX_POINT ( 'NONE', #30243 ) ;
#108564 = EDGE_LOOP ( 'NONE', ( #24304, #14222 ) ) ;
#108565 = DIRECTION ( 'NONE',  ( 0.000000000000000000, 1.000000000000000000, 0.000000000000000000 ) ) ;
#108566 = CARTESIAN_POINT ( 'NONE',  ( -1.700000000000034817, 2.500000000000000000, -4.230127018922201998 ) ) ;
#108567 = PRODUCT_CONTEXT ( 'NONE', #2834, 'mechanical' ) ;
#108568 = DIRECTION ( 'NONE',  ( 0.000000000000000000, 1.000000000000000000, 0.000000000000000000 ) ) ;
#108569 = DIRECTION ( 'NONE',  ( -4.274815082592931898E-19, -0.9999939076577903929, -0.003490651415223739937 ) ) ;
#108570 = CARTESIAN_POINT ( 'NONE',  ( -10.40000000000000213, 12.50000000000000000, -4.330127018922197202 ) ) ;
#108571 = DIRECTION ( 'NONE',  ( 0.000000000000000000, 0.000000000000000000, -1.000000000000000000 ) ) ;
#108572 = VECTOR ( 'NONE', #127238, 1000.000000000000000 ) ;
#108573 = DIRECTION ( 'NONE',  ( 0.000000000000000000, 1.000000000000000000, 0.000000000000000000 ) ) ;
#108574 = DIRECTION ( 'NONE',  ( 0.000000000000000000, 0.000000000000000000, 1.000000000000000000 ) ) ;
#108575 = EDGE_LOOP ( 'NONE', ( #1458, #11454 ) ) ;
#108576 = ORIENTED_EDGE ( 'NONE', *, *, #88300, .T. ) ;
#108577 = ADVANCED_FACE ( 'NONE', ( #1394 ), #73762, .T. ) ;
#108578 = DIRECTION ( 'NONE',  ( -4.274815082592931898E-19, -0.9999939076577903929, -0.003490651415223739937 ) ) ;
#108579 = ADVANCED_FACE ( 'NONE', ( #28943 ), #94697, .T. ) ;
#108580 = CARTESIAN_POINT ( 'NONE',  ( 2.899999999999946620, 2.500000000000000000, -5.022947341949754119 ) ) ;
#108581 = ORIENTED_EDGE ( 'NONE', *, *, #85896, .T. ) ;
#108582 = ORIENTED_EDGE ( 'NONE', *, *, #31682, .F. ) ;
#108583 = CARTESIAN_POINT ( 'NONE',  ( 185.9843750003414016, -8.734944146203032389, -1.604583208406768146E-15 ) ) ;
#108584 = DIRECTION ( 'NONE',  ( 0.000000000000000000, 0.000000000000000000, 1.000000000000000000 ) ) ;
#108585 = VECTOR ( 'NONE', #113404, 1000.000000000000000 ) ;
#108586 = DIRECTION ( 'NONE',  ( 0.000000000000000000, -0.9999939076577903929, 0.003490651415223739937 ) ) ;
#108587 = EDGE_CURVE ( 'NONE', #123389, #56994, #38779, .T. ) ;
#108588 = CARTESIAN_POINT ( 'NONE',  ( 9.599999999999914380, 12.50000000000000000, -4.330127018922201643 ) ) ;
#108589 = CARTESIAN_POINT ( 'NONE',  ( -14.19999999999998685, 12.50000000000000000, -1.084202172485504434E-16 ) ) ;
#108590 = CARTESIAN_POINT ( 'NONE',  ( -11.64999999999999680, 2.500000000000000000, -7.088010851410849966 ) ) ;
#108591 = DIRECTION ( 'NONE',  ( 0.000000000000000000, 0.000000000000000000, -1.000000000000000000 ) ) ;
#108592 = AXIS2_PLACEMENT_3D ( 'NONE', #119333, #69592, #100987 ) ;
#108593 = DIRECTION ( 'NONE',  ( -0.000000000000000000, -1.000000000000000000, -0.000000000000000000 ) ) ;
#108594 = ORIENTED_EDGE ( 'NONE', *, *, #994, .F. ) ;
#108595 = CONICAL_SURFACE ( 'NONE', #50044, 0.1000000000000002554, 0.003490658503988666988 ) ;
#108596 = ORIENTED_EDGE ( 'NONE', *, *, #382, .T. ) ;
#108597 = ADVANCED_BREP_SHAPE_REPRESENTATION ( '', ( #99052, #108296 ), #5971 ) ;
#108598 = AXIS2_PLACEMENT_3D ( 'NONE', #25774, #26431, #57168 ) ;
#108599 = ORIENTED_EDGE ( 'NONE', *, *, #85064, .F. ) ;
#108600 = ORIENTED_EDGE ( 'NONE', *, *, #30653, .T. ) ;
#108601 = CARTESIAN_POINT ( 'NONE',  ( 4.349999999999939249, 2.500000000000000000, 2.411473670974873862 ) ) ;
#108602 = DIRECTION ( 'NONE',  ( -0.000000000000000000, -1.000000000000000000, -0.000000000000000000 ) ) ;
#108603 = EDGE_LOOP ( 'NONE', ( #58836, #69242 ) ) ;
#108604 = DIRECTION ( 'NONE',  ( 0.000000000000000000, 0.000000000000000000, 1.000000000000000000 ) ) ;
#108605 = CARTESIAN_POINT ( 'NONE',  ( 10.84999999999991260, 2.500000000000000000, -2.857883832488653741 ) ) ;
#108606 = DIRECTION ( 'NONE',  ( -0.000000000000000000, 1.000000000000000000, -0.000000000000000000 ) ) ;
#108608 = ORIENTED_EDGE ( 'NONE', *, *, #63892, .T. ) ;
#108607 = CARTESIAN_POINT ( 'NONE',  ( -1.250000000000037526, 12.50000000000000000, -1.407149913249512663 ) ) ;
#108609 = CARTESIAN_POINT ( 'NONE',  ( 9.149999999999916866, 2.500000000000000000, -1.572243186433550211 ) ) ;
#108610 = DIRECTION ( 'NONE',  ( 0.000000000000000000, -0.000000000000000000, 1.000000000000000000 ) ) ;
#108611 = ADVANCED_FACE ( 'NONE', ( #68199 ), #50798, .T. ) ;
#108612 = ORIENTED_EDGE ( 'NONE', *, *, #32851, .T. ) ;
#108613 = ORIENTED_EDGE ( 'NONE', *, *, #28854, .F. ) ;
#108614 = ORIENTED_EDGE ( 'NONE', *, *, #27658, .T. ) ;
#108615 = AXIS2_PLACEMENT_3D ( 'NONE', #38855, #17882, #68268 ) ;
#108616 = ORIENTED_EDGE ( 'NONE', *, *, #124651, .T. ) ;
#108617 = DIRECTION ( 'NONE',  ( 0.000000000000000000, 1.000000000000000000, 0.000000000000000000 ) ) ;
#108618 = CARTESIAN_POINT ( 'NONE',  ( -2.100000000000033840, 12.50000000000000000, 5.088040615133786027 ) ) ;
#108619 = AXIS2_PLACEMENT_3D ( 'NONE', #67862, #58066, #8292 ) ;
#108621 = ORIENTED_EDGE ( 'NONE', *, *, #65832, .F. ) ;
#108620 = ADVANCED_FACE ( 'NONE', ( #48579 ), #77981, .T. ) ;
#108622 = DIRECTION ( 'NONE',  ( -0.000000000000000000, -1.000000000000000000, -0.000000000000000000 ) ) ;
#108623 = CARTESIAN_POINT ( 'NONE',  ( 5.599999999999934808, 12.50000000000000000, -4.676537180435978769 ) ) ;
#108624 = CARTESIAN_POINT ( 'NONE',  ( 14.79999999999989413, 2.500000000000000000, -0.2464101615137782308 ) ) ;
#108625 = DIRECTION ( 'NONE',  ( 0.000000000000000000, 0.000000000000000000, -1.000000000000000000 ) ) ;
#108626 = ADVANCED_FACE ( 'NONE', ( #39423 ), #32034, .T. ) ;
#108627 = CIRCLE ( 'NONE', #12392, 0.06509327318403741736 ) ;
#108628 = AXIS2_PLACEMENT_3D ( 'NONE', #23248, #35038, #114848 ) ;
#108629 = VERTEX_POINT ( 'NONE', #110700 ) ;
#108630 = DIRECTION ( 'NONE',  ( -0.000000000000000000, 1.000000000000000000, -0.000000000000000000 ) ) ;
#108631 = ORIENTED_EDGE ( 'NONE', *, *, #99654, .F. ) ;
#108632 = ORIENTED_EDGE ( 'NONE', *, *, #57240, .F. ) ;
#108633 = DIRECTION ( 'NONE',  ( 0.000000000000000000, 0.000000000000000000, -1.000000000000000000 ) ) ;
#108634 = EDGE_CURVE ( 'NONE', #86589, #6482, #111413, .T. ) ;
#108635 = CARTESIAN_POINT ( 'NONE',  ( 4.799999999999937650, 12.50000000000000000, -0.4115034346978156399 ) ) ;
#108636 = FACE_BOUND ( 'NONE', #68845, .T. ) ;
#108637 = VECTOR ( 'NONE', #72765, 1000.000000000000000 ) ;
#108638 = DIRECTION ( 'NONE',  ( 0.000000000000000000, 0.000000000000000000, -1.000000000000000000 ) ) ;
#108639 = DIRECTION ( 'NONE',  ( 0.000000000000000000, 0.000000000000000000, -1.000000000000000000 ) ) ;
#108640 = CARTESIAN_POINT ( 'NONE',  ( -1.050000000000038680, 12.50000000000000000, 6.906693963081109722 ) ) ;
#108641 = AXIS2_PLACEMENT_3D ( 'NONE', #68200, #18463, #40710 ) ;
#108642 = CONICAL_SURFACE ( 'NONE', #27089, 0.1000000000000000472, 0.003490658503988666988 ) ;
#108643 = VERTEX_POINT ( 'NONE', #78696 ) ;
#108644 = DIRECTION ( 'NONE',  ( 0.000000000000000000, -0.000000000000000000, 1.000000000000000000 ) ) ;
#108645 = LINE ( 'NONE', #68074, #32301 ) ;
#108646 = CARTESIAN_POINT ( 'NONE',  ( 4.149999999999939959, 12.50000000000000000, 1.537336459617582918 ) ) ;
#108647 = DIRECTION ( 'NONE',  ( -0.000000000000000000, -1.000000000000000000, -0.000000000000000000 ) ) ;
#108648 = ORIENTED_EDGE ( 'NONE', *, *, #91523, .T. ) ;
#108649 = AXIS2_PLACEMENT_3D ( 'NONE', #107345, #74666, #17671 ) ;
#108650 = DIRECTION ( 'NONE',  ( 0.000000000000000000, -0.000000000000000000, 1.000000000000000000 ) ) ;
#108651 = DIRECTION ( 'NONE',  ( 0.000000000000000000, 1.000000000000000000, 0.000000000000000000 ) ) ;
#108652 = CIRCLE ( 'NONE', #116957, 0.06509327318403745899 ) ;
#108653 = ORIENTED_EDGE ( 'NONE', *, *, #25077, .F. ) ;
#108654 = ORIENTED_EDGE ( 'NONE', *, *, #22842, .F. ) ;
#108655 = FACE_OUTER_BOUND ( 'NONE', #14670, .T. ) ;
#108656 = DIRECTION ( 'NONE',  ( -0.000000000000000000, -1.000000000000000000, -0.000000000000000000 ) ) ;
#108657 = FACE_BOUND ( 'NONE', #52672, .T. ) ;
#108658 = CARTESIAN_POINT ( 'NONE',  ( 7.699999999999922018, 2.500000000000000000, 0.3464101615137735735 ) ) ;
#108659 = EDGE_CURVE ( 'NONE', #90797, #36770, #118590, .T. ) ;
#108660 = ORIENTED_EDGE ( 'NONE', *, *, #99043, .F. ) ;
#108661 = CARTESIAN_POINT ( 'NONE',  ( 4.999999999999933387, 2.500000000000000000, 5.022947341949748790 ) ) ;
#108662 = ORIENTED_EDGE ( 'NONE', *, *, #70563, .F. ) ;
#108663 =( BOUNDED_SURFACE ( )  B_SPLINE_SURFACE ( 3, 2, ( 
 ( #27981, #65313, #94791 ),
 ( #124896, #17499, #116351 ),
 ( #107174, #35874, #77086 ),
 ( #77709, #115052, #116985 ),
 ( #86238, #35242, #96706 ),
 ( #27316, #67221, #57447 ),
 ( #105251, #36534, #105901 ),
 ( #45065, #76444, #87536 ),
 ( #97365, #26695, #5740 ),
 ( #67900, #84964, #7679 ),
 ( #46991, #47627, #127477 ),
 ( #25386, #65972, #117618 ) ),
 .UNSPECIFIED., .F., .F., .F. ) 
 B_SPLINE_SURFACE_WITH_KNOTS ( ( 4, 2, 2, 2, 2, 4 ),
 ( 3, 3 ),
 ( -5.075233897142896741E-05, 0.01652955890756899540, 0.03310987015410941925, 0.04969018140064984657, 0.05798033702392006022, 0.06627049264719027388 ),
 ( 0.000000000000000000, 1.000000000000000000 ),
 .UNSPECIFIED. ) 
 GEOMETRIC_REPRESENTATION_ITEM ( )  RATIONAL_B_SPLINE_SURFACE ( (
 ( 1.000000000000000000, 1.000000000000000000, 1.000000000000000000),
 ( 1.000000000000000000, 0.9999962913215033611, 1.000000000000000000),
 ( 1.000000000000000000, 0.9967432547760589623, 1.000000000000000000),
 ( 1.000000000000000000, 0.9780629203682255079, 1.000000000000000000),
 ( 1.000000000000000000, 0.9624374449458362735, 1.000000000000000000),
 ( 1.000000000000000000, 0.9156028756809130309, 1.000000000000000000),
 ( 1.000000000000000000, 0.8842425818972232676, 1.000000000000000000),
 ( 1.000000000000000000, 0.8293059173979305809, 1.000000000000000000),
 ( 1.000000000000000000, 0.8097380764759147809, 1.000000000000000000),
 ( 1.000000000000000000, 0.7702514575408279107, 1.000000000000000000),
 ( 1.000000000000000000, 0.7503390841288218871, 1.000000000000000000),
 ( 1.000000000000000000, 0.7318752858502189929, 1.000000000000000000) ) ) 
 REPRESENTATION_ITEM ( '' )  SURFACE ( )  );
#108664 = VERTEX_POINT ( 'NONE', #83198 ) ;
#108665 = PLANE ( 'NONE',  #115559 ) ;
#108666 = EDGE_CURVE ( 'NONE', #81572, #8476, #105160, .T. ) ;
#108667 = CARTESIAN_POINT ( 'NONE',  ( 185.5416666666666572, -4.445597072760122614, 7.699999999999998401 ) ) ;
#108668 = EDGE_CURVE ( 'NONE', #73062, #37904, #3337, .T. ) ;
#108669 = VERTEX_POINT ( 'NONE', #13784 ) ;
#108670 = LINE ( 'NONE', #18989, #17559 ) ;
#108671 = DIRECTION ( 'NONE',  ( 0.000000000000000000, 1.000000000000000000, 0.000000000000000000 ) ) ;
#108672 = EDGE_CURVE ( 'NONE', #88690, #74641, #91715, .T. ) ;
#108673 = ADVANCED_FACE ( 'NONE', ( #24261 ), #90585, .T. ) ;
#108674 = CARTESIAN_POINT ( 'NONE',  ( -8.150000000000014566, 12.50000000000000000, -6.148780366869520897 ) ) ;
#108675 = AXIS2_PLACEMENT_3D ( 'NONE', #86980, #126269, #34684 ) ;
#108676 = ADVANCED_FACE ( 'NONE', ( #121813 ), #6938, .T. ) ;
#108677 = DIRECTION ( 'NONE',  ( 0.000000000000000000, -0.9999939076577903929, 0.003490651415223739937 ) ) ;
#108678 = EDGE_LOOP ( 'NONE', ( #10349, #21409, #122662, #111572 ) ) ;
#108679 = FACE_OUTER_BOUND ( 'NONE', #11608, .T. ) ;
#108682 = ADVANCED_FACE ( 'NONE', ( #53723 ), #44627, .T. ) ;
#108681 = CIRCLE ( 'NONE', #52262, 0.1000000000000002554 ) ;
#108680 = AXIS2_PLACEMENT_3D ( 'NONE', #50824, #41022, #12163 ) ;
#108683 = CARTESIAN_POINT ( 'NONE',  ( -3.750000000000026201, 2.500000000000000000, 5.802370205355744659 ) ) ;
#108684 = CARTESIAN_POINT ( 'NONE',  ( 184.5312500006828031, 9.429780353434619030E-16, -7.700000000000000178 ) ) ;
#108685 = DIRECTION ( 'NONE',  ( 0.000000000000000000, 0.000000000000000000, 1.000000000000000000 ) ) ;
#108686 = VERTEX_POINT ( 'NONE', #93653 ) ;
#108687 = ORIENTED_EDGE ( 'NONE', *, *, #89777, .F. ) ;
#108688 = CARTESIAN_POINT ( 'NONE',  ( -12.09999999999999609, 2.500000000000000000, -3.537306695894647302 ) ) ;
#108689 = EDGE_CURVE ( 'NONE', #47413, #100917, #2857, .T. ) ;
#108690 = ORIENTED_EDGE ( 'NONE', *, *, #45358, .T. ) ;
#108691 = DIRECTION ( 'NONE',  ( 0.000000000000000000, -0.9999939076577903929, 0.003490651415223739937 ) ) ;
#108694 = DIRECTION ( 'NONE',  ( 0.000000000000000000, 0.000000000000000000, -1.000000000000000000 ) ) ;
#108693 = AXIS2_PLACEMENT_3D ( 'NONE', #113303, #113956, #94969 ) ;
#108692 = VECTOR ( 'NONE', #77379, 1000.000000000000000 ) ;
#108695 = CARTESIAN_POINT ( 'NONE',  ( -3.950000000000024603, 12.50000000000000000, 1.883746621131358934 ) ) ;
#108696 = CARTESIAN_POINT ( 'NONE',  ( 6.899999999999928413, 2.500000000000000000, 4.676537180435972552 ) ) ;
#108697 = ORIENTED_EDGE ( 'NONE', *, *, #45744, .T. ) ;
#108698 = CARTESIAN_POINT ( 'NONE',  ( -14.79999999999998295, 2.500000000000000000, -0.3464101615137760715 ) ) ;
#108699 = DIRECTION ( 'NONE',  ( 0.000000000000000000, -0.9999939076577903929, 0.003490651415223739937 ) ) ;
#108700 = CARTESIAN_POINT ( 'NONE',  ( 81.97642828244310920, 3.858501901686324675, -6.173828276686423422 ) ) ;
#108701 = CARTESIAN_POINT ( 'NONE',  ( 184.9010416670080588, -4.367472073101520635, 7.564683531249999149 ) ) ;
#108702 = CARTESIAN_POINT ( 'NONE',  ( 8.949999999999915801, 2.500000000000000000, -1.818653347947326138 ) ) ;
#108703 = CARTESIAN_POINT ( 'NONE',  ( 7.499999999999925393, 2.500000000000000000, -3.737306695894649700 ) ) ;
#108704 = ORIENTED_EDGE ( 'NONE', *, *, #114097, .F. ) ;
#108705 = ORIENTED_EDGE ( 'NONE', *, *, #116206, .T. ) ;
#108706 = DIRECTION ( 'NONE',  ( 0.000000000000000000, 0.000000000000000000, -1.000000000000000000 ) ) ;
#108707 = ORIENTED_EDGE ( 'NONE', *, *, #57557, .T. ) ;
#108708 = CARTESIAN_POINT ( 'NONE',  ( -15.39999999999997904, 2.500000000000000000, 0.000000000000000000 ) ) ;
#108710 = ORIENTED_EDGE ( 'NONE', *, *, #25320, .T. ) ;
#108709 = ORIENTED_EDGE ( 'NONE', *, *, #2584, .T. ) ;
#108711 = VERTEX_POINT ( 'NONE', #72724 ) ;
#108712 = FACE_OUTER_BOUND ( 'NONE', #36059, .T. ) ;
#108713 = CARTESIAN_POINT ( 'NONE',  ( 2.899999999999943956, 2.500000000000000000, 4.430127018922196847 ) ) ;
#108714 = AXIS2_PLACEMENT_3D ( 'NONE', #129178, #87276, #127226 ) ;
#108715 = FACE_OUTER_BOUND ( 'NONE', #30488, .T. ) ;
#108716 = CARTESIAN_POINT ( 'NONE',  ( -10.65000000000000213, 2.500000000000000000, 6.148780366869520009 ) ) ;
#108717 = DIRECTION ( 'NONE',  ( 0.000000000000000000, 0.000000000000000000, -1.000000000000000000 ) ) ;
#108718 = CARTESIAN_POINT ( 'NONE',  ( 5.399999999999936406, 2.500000000000000000, -5.122947341949753763 ) ) ;
#108719 = FACE_OUTER_BOUND ( 'NONE', #86724, .T. ) ;
#108721 = CIRCLE ( 'NONE', #62852, 0.06509327318403745899 ) ;
#108720 = DIRECTION ( 'NONE',  ( 0.000000000000000000, -0.000000000000000000, 1.000000000000000000 ) ) ;
#108722 = EDGE_LOOP ( 'NONE', ( #66725, #88545 ) ) ;
#108723 = ORIENTED_EDGE ( 'NONE', *, *, #110394, .T. ) ;
#108724 = EDGE_CURVE ( 'NONE', #61381, #94776, #19586, .T. ) ;
#108725 = DIRECTION ( 'NONE',  ( -0.000000000000000000, 1.000000000000000000, -0.000000000000000000 ) ) ;
#108726 = VERTEX_POINT ( 'NONE', #31509 ) ;
#108727 = EDGE_LOOP ( 'NONE', ( #127251, #10156, #114116, #22002 ) ) ;
#108728 = DIRECTION ( 'NONE',  ( 0.000000000000000000, -0.9999939076577903929, 0.003490651415223739937 ) ) ;
#108729 = AXIS2_PLACEMENT_3D ( 'NONE', #29959, #6560, #89512 ) ;
#108730 = ADVANCED_FACE ( 'NONE', ( #121175 ), #86381, .T. ) ;
#108731 = AXIS2_PLACEMENT_3D ( 'NONE', #106828, #6050, #17136 ) ;
#108732 = CARTESIAN_POINT ( 'NONE',  ( -11.25000000000000000, 2.500000000000000000, 2.857883832488649301 ) ) ;
#108733 = AXIS2_PLACEMENT_3D ( 'NONE', #83219, #123139, #34120 ) ;
#108734 = CARTESIAN_POINT ( 'NONE',  ( 5.799999999999933209, 12.50000000000000000, -2.385244779468109755E-15 ) ) ;
#108735 = CARTESIAN_POINT ( 'NONE',  ( 4.549999999999935874, 2.500000000000000000, 6.395190528383296602 ) ) ;
#108736 = CARTESIAN_POINT ( 'NONE',  ( 1.699999999999950218, 2.500000000000000000, 4.330127018922196314 ) ) ;
#108737 = ORIENTED_EDGE ( 'NONE', *, *, #8522, .F. ) ;
#108738 = CIRCLE ( 'NONE', #121350, 0.06509327318403745899 ) ;
#108739 = ORIENTED_EDGE ( 'NONE', *, *, #51797, .T. ) ;
#108740 = DIRECTION ( 'NONE',  ( 0.000000000000000000, -0.000000000000000000, 1.000000000000000000 ) ) ;
#108741 = ORIENTED_EDGE ( 'NONE', *, *, #73045, .T. ) ;
#108742 = CARTESIAN_POINT ( 'NONE',  ( 8.749999999999923617, 2.500000000000000000, 1.472243186433545459 ) ) ;
#108743 = AXIS2_PLACEMENT_3D ( 'NONE', #128322, #27495, #107371 ) ;
#108744 = VERTEX_POINT ( 'NONE', #61626 ) ;
#108745 = ORIENTED_EDGE ( 'NONE', *, *, #128660, .F. ) ;
#108746 = CARTESIAN_POINT ( 'NONE',  ( 1.249999999999953815, 2.500000000000000000, -2.957883832488653830 ) ) ;
#108747 = CARTESIAN_POINT ( 'NONE',  ( 5.199999999999935341, 2.500000000000000000, -3.983716857408426293 ) ) ;
#108748 = DIRECTION ( 'NONE',  ( 0.000000000000000000, 0.000000000000000000, -1.000000000000000000 ) ) ;
#108749 = DIRECTION ( 'NONE',  ( 0.000000000000000000, 0.000000000000000000, -1.000000000000000000 ) ) ;
#108750 = DIRECTION ( 'NONE',  ( 0.000000000000000000, 0.000000000000000000, 1.000000000000000000 ) ) ;
#108751 = ORIENTED_EDGE ( 'NONE', *, *, #49916, .F. ) ;
#108752 = DIRECTION ( 'NONE',  ( -4.274815082592931898E-19, -0.9999939076577903929, -0.003490651415223739937 ) ) ;
#108753 = LINE ( 'NONE', #50487, #62056 ) ;
#108754 = CARTESIAN_POINT ( 'NONE',  ( 4.999999999999936939, 12.50000000000000000, -0.6928203230275541413 ) ) ;
#108755 = CARTESIAN_POINT ( 'NONE',  ( -0.2000000000000404232, 12.50000000000000000, 3.983716857408420964 ) ) ;
#108756 = DIRECTION ( 'NONE',  ( -0.000000000000000000, 1.000000000000000000, -0.000000000000000000 ) ) ;
#108757 = ADVANCED_FACE ( 'NONE', ( #113278 ), #63552, .T. ) ;
#108758 = ORIENTED_EDGE ( 'NONE', *, *, #42961, .T. ) ;
#108759 = VERTEX_POINT ( 'NONE', #112649 ) ;
#108760 = VECTOR ( 'NONE', #60617, 1000.000000000000000 ) ;
#108761 = CARTESIAN_POINT ( 'NONE',  ( 2.099999999999950351, 2.500000000000000000, -4.922947341949753586 ) ) ;
#108762 = CIRCLE ( 'NONE', #50293, 0.1000000000000000472 ) ;
#108763 = ORIENTED_EDGE ( 'NONE', *, *, #110128, .T. ) ;
#108764 = DIRECTION ( 'NONE',  ( -0.000000000000000000, -1.000000000000000000, -0.000000000000000000 ) ) ;
#108766 = EDGE_CURVE ( 'NONE', #17919, #77627, #81875, .T. ) ;
#108765 = DIRECTION ( 'NONE',  ( -0.000000000000000000, 1.000000000000000000, -0.000000000000000000 ) ) ;
#108768 = CIRCLE ( 'NONE', #38106, 0.1000000000000000472 ) ;
#108767 = VECTOR ( 'NONE', #34915, 1000.000000000000000 ) ;
#108770 = EDGE_LOOP ( 'NONE', ( #124523, #90663, #16681, #103904 ) ) ;
#108769 = EDGE_CURVE ( 'NONE', #14739, #10534, #27898, .T. ) ;
#108771 = DIRECTION ( 'NONE',  ( 0.000000000000000000, 1.000000000000000000, 0.000000000000000000 ) ) ;
#108772 = CARTESIAN_POINT ( 'NONE',  ( -5.600000000000020073, 12.50000000000000000, 4.048810130592458201 ) ) ;
#108773 = DIRECTION ( 'NONE',  ( 0.000000000000000000, 0.000000000000000000, 1.000000000000000000 ) ) ;
#108774 = EDGE_CURVE ( 'NONE', #46669, #36193, #74011, .T. ) ;
#108775 = DIRECTION ( 'NONE',  ( 0.000000000000000000, 0.000000000000000000, 1.000000000000000000 ) ) ;
#108776 = ORIENTED_EDGE ( 'NONE', *, *, #115236, .T. ) ;
#108777 = DIRECTION ( 'NONE',  ( -0.000000000000000000, -1.000000000000000000, -0.000000000000000000 ) ) ;
#108778 = EDGE_CURVE ( 'NONE', #92869, #33146, #128267, .T. ) ;
#108779 = VERTEX_POINT ( 'NONE', #53083 ) ;
#108780 = EDGE_CURVE ( 'NONE', #34969, #89288, #43280, .T. ) ;
#108781 = CARTESIAN_POINT ( 'NONE',  ( 24.00483293780993321, 0.9037283375177144196, -4.313967621098822036 ) ) ;
#108782 = CARTESIAN_POINT ( 'NONE',  ( -11.69999999999999574, 12.50000000000000000, 4.330127018922196314 ) ) ;
#108783 = DIRECTION ( 'NONE',  ( 0.000000000000000000, -0.000000000000000000, 1.000000000000000000 ) ) ;
#108784 = VERTEX_POINT ( 'NONE', #3969 ) ;
#108785 = DIRECTION ( 'NONE',  ( 0.000000000000000000, 0.000000000000000000, -1.000000000000000000 ) ) ;
#108786 = ORIENTED_EDGE ( 'NONE', *, *, #40416, .F. ) ;
#108787 = CARTESIAN_POINT ( 'NONE',  ( 108.0000000000000142, 9.000000000000001776, 0.000000000000000000 ) ) ;
#108788 = DIRECTION ( 'NONE',  ( -0.000000000000000000, -1.000000000000000000, -0.000000000000000000 ) ) ;
#108789 = DIRECTION ( 'NONE',  ( -0.000000000000000000, 1.000000000000000000, -0.000000000000000000 ) ) ;
#108790 = ORIENTED_EDGE ( 'NONE', *, *, #67786, .T. ) ;
#108791 = CIRCLE ( 'NONE', #54509, 0.06509327318403745899 ) ;
#108792 = DIRECTION ( 'NONE',  ( -0.000000000000000000, 1.000000000000000000, -0.000000000000000000 ) ) ;
#108793 = AXIS2_PLACEMENT_3D ( 'NONE', #53526, #4382, #44331 ) ;
#108794 = DIRECTION ( 'NONE',  ( -0.000000000000000000, -1.000000000000000000, -0.000000000000000000 ) ) ;
#108795 = ADVANCED_FACE ( 'NONE', ( #83818 ), #25849, .T. ) ;
#108796 = ORIENTED_EDGE ( 'NONE', *, *, #83444, .T. ) ;
#108797 = DIRECTION ( 'NONE',  ( -0.000000000000000000, 1.000000000000000000, -0.000000000000000000 ) ) ;
#108798 = ORIENTED_EDGE ( 'NONE', *, *, #40603, .T. ) ;
#108799 = AXIS2_PLACEMENT_3D ( 'NONE', #21377, #61317, #19437 ) ;
#108800 = DIRECTION ( 'NONE',  ( 0.000000000000000000, 0.000000000000000000, 1.000000000000000000 ) ) ;
#108801 = EDGE_CURVE ( 'NONE', #124608, #77665, #44550, .T. ) ;
#108802 = ORIENTED_EDGE ( 'NONE', *, *, #39285, .T. ) ;
#108803 = CARTESIAN_POINT ( 'NONE',  ( -8.350000000000013856, 12.50000000000000000, -6.495190528383297135 ) ) ;
#108804 = DIRECTION ( 'NONE',  ( -0.000000000000000000, 1.000000000000000000, -0.000000000000000000 ) ) ;
#108805 = EDGE_LOOP ( 'NONE', ( #78176, #111080 ) ) ;
#108806 = EDGE_LOOP ( 'NONE', ( #26104, #14634 ) ) ;
#108807 = DIRECTION ( 'NONE',  ( -0.000000000000000000, 1.000000000000000000, -0.000000000000000000 ) ) ;
#108808 = CARTESIAN_POINT ( 'NONE',  ( -9.550000000000006040, 2.500000000000000000, -2.165063509461101710 ) ) ;
#108809 = ORIENTED_EDGE ( 'NONE', *, *, #5073, .T. ) ;
#108810 = ADVANCED_FACE ( 'NONE', ( #34750 ), #103113, .T. ) ;
#108812 = LINE ( 'NONE', #58456, #69811 ) ;
#108811 = AXIS2_PLACEMENT_3D ( 'NONE', #106046, #5888, #26843 ) ;
#108813 = CARTESIAN_POINT ( 'NONE',  ( 186.0312500006828031, 9.429780353434619030E-16, -7.700000000000000178 ) ) ;
#108814 = CARTESIAN_POINT ( 'NONE',  ( 12.94999999999990337, 2.500000000000000000, 2.165063509461097713 ) ) ;
#108815 = CARTESIAN_POINT ( 'NONE',  ( 103.0003941427382301, 8.699773481286413812, 0.3429536323214144589 ) ) ;
#108816 = DIRECTION ( 'NONE',  ( 0.000000000000000000, 0.000000000000000000, 1.000000000000000000 ) ) ;
#108817 = EDGE_CURVE ( 'NONE', #32380, #95927, #101058, .T. ) ;
#108818 = DIRECTION ( 'NONE',  ( -0.000000000000000000, 1.000000000000000000, -0.000000000000000000 ) ) ;
#108819 = LINE ( 'NONE', #97721, #96486 ) ;
#108820 = EDGE_CURVE ( 'NONE', #37294, #78706, #105258, .T. ) ;
#108822 = ADVANCED_FACE ( 'NONE', ( #74647 ), #97988, .T. ) ;
#108821 = CIRCLE ( 'NONE', #39903, 0.1000000000000002554 ) ;
#108823 = ORIENTED_EDGE ( 'NONE', *, *, #17420, .T. ) ;
#108824 = EDGE_LOOP ( 'NONE', ( #5803, #5330 ) ) ;
#108826 = VERTEX_POINT ( 'NONE', #118924 ) ;
#108825 = EDGE_CURVE ( 'NONE', #9410, #86367, #24908, .T. ) ;
#108827 = ORIENTED_EDGE ( 'NONE', *, *, #36978, .F. ) ;
#108828 = DIRECTION ( 'NONE',  ( 0.000000000000000000, -0.000000000000000000, 1.000000000000000000 ) ) ;
#108829 = DIRECTION ( 'NONE',  ( 0.000000000000000000, 1.000000000000000000, 0.000000000000000000 ) ) ;
#108830 = DIRECTION ( 'NONE',  ( 0.000000000000000000, 0.000000000000000000, 1.000000000000000000 ) ) ;
#108831 = VERTEX_POINT ( 'NONE', #55004 ) ;
#108832 = FACE_BOUND ( 'NONE', #56904, .T. ) ;
#108833 = ORIENTED_EDGE ( 'NONE', *, *, #79641, .F. ) ;
#108834 = CARTESIAN_POINT ( 'NONE',  ( 1.049999999999953637, 2.500000000000000000, -1.818653347947326138 ) ) ;
#108835 = CARTESIAN_POINT ( 'NONE',  ( -9.800000000000006040, 12.50000000000000000, 4.741630453620009789 ) ) ;
#108836 = ADVANCED_FACE ( 'NONE', ( #48248 ), #15047, .T. ) ;
#108837 = EDGE_CURVE ( 'NONE', #73563, #12234, #69161, .T. ) ;
#108838 = LINE ( 'NONE', #110775, #70179 ) ;
#108839 = EDGE_CURVE ( 'NONE', #53810, #99657, #38387, .T. ) ;
#108840 = LINE ( 'NONE', #17886, #120317 ) ;
#108841 = CARTESIAN_POINT ( 'NONE',  ( -5.850000000000018296, 2.500000000000000000, 2.857883832488649301 ) ) ;
#108842 = DIRECTION ( 'NONE',  ( 0.000000000000000000, 0.000000000000000000, 1.000000000000000000 ) ) ;
#108843 = CARTESIAN_POINT ( 'NONE',  ( 2.699999999999947331, 2.500000000000000000, -4.676537180435978769 ) ) ;
#108844 = DIRECTION ( 'NONE',  ( 0.000000000000000000, -0.9999939076577903929, 0.003490651415223739937 ) ) ;
#108845 = DIRECTION ( 'NONE',  ( 0.000000000000000000, 0.000000000000000000, 1.000000000000000000 ) ) ;
#108846 = CARTESIAN_POINT ( 'NONE',  ( 6.049999999999932321, 12.50000000000000000, -1.818653347947326138 ) ) ;
#108847 = ORIENTED_EDGE ( 'NONE', *, *, #58159, .T. ) ;
#108848 = ORIENTED_EDGE ( 'NONE', *, *, #73509, .F. ) ;
#108849 = ORIENTED_EDGE ( 'NONE', *, *, #106943, .F. ) ;
#108850 = EDGE_LOOP ( 'NONE', ( #101807, #96010 ) ) ;
#108851 = CARTESIAN_POINT ( 'NONE',  ( 3.549999999999943867, 12.50000000000000000, -6.213873640053564351 ) ) ;
#108852 = AXIS2_PLACEMENT_3D ( 'NONE', #98915, #69445, #30842 ) ;
#108853 = DIRECTION ( 'NONE',  ( -0.000000000000000000, 1.000000000000000000, -0.000000000000000000 ) ) ;
#108854 = VECTOR ( 'NONE', #43551, 1000.000000000000000 ) ;
#108856 = ORIENTED_EDGE ( 'NONE', *, *, #37712, .T. ) ;
#108855 = ORIENTED_EDGE ( 'NONE', *, *, #122127, .T. ) ;
#108857 = EDGE_LOOP ( 'NONE', ( #12242, #81104 ) ) ;
#108858 = DIRECTION ( 'NONE',  ( 0.000000000000000000, 0.000000000000000000, 1.000000000000000000 ) ) ;
#108859 = CARTESIAN_POINT ( 'NONE',  ( -11.05000000000000071, 2.500000000000000000, -2.411473670974874306 ) ) ;
#108860 = CARTESIAN_POINT ( 'NONE',  ( 185.7916666666666856, 4.445597072760072876, -7.700000000000080114 ) ) ;
#108861 = CARTESIAN_POINT ( 'NONE',  ( -4.350000000000023626, 12.50000000000000000, 1.818653347947321475 ) ) ;
#108862 = DIRECTION ( 'NONE',  ( 0.000000000000000000, 1.000000000000000000, 0.000000000000000000 ) ) ;
#108863 = LINE ( 'NONE', #19184, #60213 ) ;
#108864 = CIRCLE ( 'NONE', #4385, 0.1000000000000002554 ) ;
#108865 = CARTESIAN_POINT ( 'NONE',  ( -8.749999999999975131, 12.50000000000000000, -2.099970236277064473 ) ) ;
#108866 = VERTEX_POINT ( 'NONE', #28622 ) ;
#108867 = CARTESIAN_POINT ( 'NONE',  ( -6.900000000000019007, 12.50000000000000000, -4.676537180435978769 ) ) ;
#108868 = VERTEX_POINT ( 'NONE', #75291 ) ;
#108869 = ORIENTED_EDGE ( 'NONE', *, *, #28005, .F. ) ;
#108870 = EDGE_LOOP ( 'NONE', ( #124130, #74494, #57676, #124493 ) ) ;
#108871 = CARTESIAN_POINT ( 'NONE',  ( -0.6500000000000403233, 12.50000000000000000, 6.148780366869520009 ) ) ;
#108872 = EDGE_LOOP ( 'NONE', ( #91084, #74907, #100037, #44010 ) ) ;
#108873 = EDGE_LOOP ( 'NONE', ( #61613, #56041 ) ) ;
#108874 = DIRECTION ( 'NONE',  ( 0.000000000000000000, 0.000000000000000000, -1.000000000000000000 ) ) ;
#108875 = EDGE_CURVE ( 'NONE', #86483, #127093, #80135, .T. ) ;
#108876 = VECTOR ( 'NONE', #33384, 1000.000000000000000 ) ;
#108877 = CARTESIAN_POINT ( 'NONE',  ( -13.09999999999999076, 2.500000000000000000, 3.983716857408420964 ) ) ;
#108878 = DIRECTION ( 'NONE',  ( 0.000000000000000000, 0.000000000000000000, 1.000000000000000000 ) ) ;
#108879 = DIRECTION ( 'NONE',  ( 0.000000000000000000, 1.000000000000000000, 0.000000000000000000 ) ) ;
#108880 = FACE_OUTER_BOUND ( 'NONE', #55040, .T. ) ;
#108881 = VERTEX_POINT ( 'NONE', #85749 ) ;
#108882 = DIRECTION ( 'NONE',  ( 0.000000000000000000, -0.000000000000000000, 1.000000000000000000 ) ) ;
#108883 = AXIS2_PLACEMENT_3D ( 'NONE', #100078, #119703, #30056 ) ;
#108884 = AXIS2_PLACEMENT_3D ( 'NONE', #73000, #94561, #22632 ) ;
#108885 = EDGE_LOOP ( 'NONE', ( #35841, #110356 ) ) ;
#108886 = DIRECTION ( 'NONE',  ( 0.000000000000000000, 0.000000000000000000, -1.000000000000000000 ) ) ;
#108887 = EDGE_LOOP ( 'NONE', ( #67204, #66687 ) ) ;
#108888 = DIRECTION ( 'NONE',  ( 0.000000000000000000, 0.000000000000000000, -1.000000000000000000 ) ) ;
#108889 = CARTESIAN_POINT ( 'NONE',  ( 9.349999999999919709, 12.50000000000000000, -6.083687093685488989 ) ) ;
#108890 = EDGE_LOOP ( 'NONE', ( #82142, #28380, #33426, #106689 ) ) ;
#108891 = DIRECTION ( 'NONE',  ( -0.000000000000000000, -1.000000000000000000, -0.000000000000000000 ) ) ;
#108892 = DIRECTION ( 'NONE',  ( -0.000000000000000000, -1.000000000000000000, -0.000000000000000000 ) ) ;
#108893 = ORIENTED_EDGE ( 'NONE', *, *, #31272, .F. ) ;
#108894 = AXIS2_PLACEMENT_3D ( 'NONE', #84156, #84805, #74346 ) ;
#108895 = AXIS2_PLACEMENT_3D ( 'NONE', #11821, #22947, #21655 ) ;
#108896 = CARTESIAN_POINT ( 'NONE',  ( 13.14999999999990088, 12.50000000000000000, 1.818653347947321475 ) ) ;
#108897 = ORIENTED_EDGE ( 'NONE', *, *, #109891, .T. ) ;
#108898 = ORIENTED_EDGE ( 'NONE', *, *, #23778, .T. ) ;
#108899 = CARTESIAN_POINT ( 'NONE',  ( 2.049999999999948308, 2.500000000000000000, 6.395190528383296602 ) ) ;
#108900 = CARTESIAN_POINT ( 'NONE',  ( -11.44999999999999751, 12.50000000000000000, 1.818653347947321475 ) ) ;
#108901 = CARTESIAN_POINT ( 'NONE',  ( -11.44999999999999751, 2.500000000000000000, 6.148780366869520897 ) ) ;
#108902 = DIRECTION ( 'NONE',  ( 0.000000000000000000, 0.000000000000000000, 1.000000000000000000 ) ) ;
#108903 = CIRCLE ( 'NONE', #77524, 0.1000000000000000056 ) ;
#108904 = VECTOR ( 'NONE', #61327, 1000.000000000000000 ) ;
#108905 = DIRECTION ( 'NONE',  ( 0.000000000000000000, 0.000000000000000000, 1.000000000000000000 ) ) ;
#108906 = EDGE_LOOP ( 'NONE', ( #120024, #96000 ) ) ;
#108907 = LINE ( 'NONE', #19238, #105115 ) ;
#108908 = AXIS2_PLACEMENT_3D ( 'NONE', #125398, #35728, #115550 ) ;
#108909 = VERTEX_POINT ( 'NONE', #19418 ) ;
#108910 = DIRECTION ( 'NONE',  ( 0.000000000000000000, 1.000000000000000000, 0.000000000000000000 ) ) ;
#108912 = ADVANCED_FACE ( 'NONE', ( #5254 ), #75932, .T. ) ;
#108911 = CARTESIAN_POINT ( 'NONE',  ( -3.100000000000028511, 2.500000000000000000, 0.3464101615137736845 ) ) ;
#108913 = ORIENTED_EDGE ( 'NONE', *, *, #89005, .T. ) ;
#108914 = AXIS2_PLACEMENT_3D ( 'NONE', #63766, #121382, #44114 ) ;
#108915 = AXIS2_PLACEMENT_3D ( 'NONE', #28572, #77656, #117558 ) ;
#108916 = EDGE_CURVE ( 'NONE', #31016, #113497, #48844, .T. ) ;
#108917 = LINE ( 'NONE', #47445, #97438 ) ;
#108918 = CARTESIAN_POINT ( 'NONE',  ( -5.450000000000019718, 2.500000000000000000, 2.265063509461097357 ) ) ;
#108919 = CARTESIAN_POINT ( 'NONE',  ( -13.54999999999999005, 12.50000000000000000, -1.818653347947323917 ) ) ;
#108920 = DIRECTION ( 'NONE',  ( -0.000000000000000000, -1.000000000000000000, -0.000000000000000000 ) ) ;
#108921 = EDGE_CURVE ( 'NONE', #23572, #83529, #96842, .T. ) ;
#108922 = DIRECTION ( 'NONE',  ( -0.000000000000000000, -1.000000000000000000, -0.000000000000000000 ) ) ;
#108923 = ORIENTED_EDGE ( 'NONE', *, *, #106639, .F. ) ;
#108924 = CARTESIAN_POINT ( 'NONE',  ( 13.14999999999989733, 2.500000000000000000, -1.718653347947325827 ) ) ;
#108925 = LINE ( 'NONE', #88659, #72337 ) ;
#108926 = CARTESIAN_POINT ( 'NONE',  ( 4.199999999999939782, 12.50000000000000000, -2.276824562219559311E-15 ) ) ;
#108927 = ADVANCED_FACE ( 'NONE', ( #15715 ), #40442, .T. ) ;
#108928 = EDGE_CURVE ( 'NONE', #21008, #50667, #45841, .T. ) ;
#108929 = EDGE_CURVE ( 'NONE', #7665, #7181, #63408, .T. ) ;
#108930 = EDGE_LOOP ( 'NONE', ( #68043, #90240 ) ) ;
#108931 = CARTESIAN_POINT ( 'NONE',  ( 3.949999999999939782, 12.50000000000000000, 2.511473670974873507 ) ) ;
#108932 = ORIENTED_EDGE ( 'NONE', *, *, #43819, .F. ) ;
#108933 = ORIENTED_EDGE ( 'NONE', *, *, #76315, .F. ) ;
#108934 = DIRECTION ( 'NONE',  ( 0.000000000000000000, 0.000000000000000000, 1.000000000000000000 ) ) ;
#108935 = AXIS2_PLACEMENT_3D ( 'NONE', #54625, #94553, #44835 ) ;
#108936 = VERTEX_POINT ( 'NONE', #18780 ) ;
#108937 = DIRECTION ( 'NONE',  ( 0.000000000000000000, -0.000000000000000000, 1.000000000000000000 ) ) ;
#108938 = CARTESIAN_POINT ( 'NONE',  ( 3.949999999999941558, 12.50000000000000000, -6.083687093685488989 ) ) ;
#108939 = ORIENTED_EDGE ( 'NONE', *, *, #105431, .T. ) ;
#108941 = PLANE ( 'NONE',  #92664 ) ;
#108940 = VECTOR ( 'NONE', #98154, 1000.000000000000000 ) ;
#108942 = CONICAL_SURFACE ( 'NONE', #52535, 0.1000000000000002554, 0.003490658503988666988 ) ;
#108944 = ORIENTED_EDGE ( 'NONE', *, *, #79004, .F. ) ;
#108943 = CARTESIAN_POINT ( 'NONE',  ( 9.549999999999915445, 12.50000000000000000, -2.230156782645139391 ) ) ;
#108945 = AXIS2_PLACEMENT_3D ( 'NONE', #99077, #9408, #46751 ) ;
#108946 = CARTESIAN_POINT ( 'NONE',  ( -2.100000000000034284, 2.500000000000000000, -4.330127018922201643 ) ) ;
#108947 = DIRECTION ( 'NONE',  ( -4.274815082592931898E-19, -0.9999939076577903929, -0.003490651415223739937 ) ) ;
#108948 = EDGE_LOOP ( 'NONE', ( #29281, #100210 ) ) ;
#108949 = VERTEX_POINT ( 'NONE', #8953 ) ;
#108950 = ORIENTED_EDGE ( 'NONE', *, *, #56283, .F. ) ;
#108951 = LINE ( 'NONE', #19289, #23233 ) ;
#108952 = CARTESIAN_POINT ( 'NONE',  ( 2.099999999999947686, 2.500000000000000000, 5.022947341949748790 ) ) ;
#108953 = CARTESIAN_POINT ( 'NONE',  ( -11.69999999999999574, 12.50000000000000000, 4.265033745738159077 ) ) ;
#108954 = FACE_BOUND ( 'NONE', #108182, .T. ) ;
#108955 = ORIENTED_EDGE ( 'NONE', *, *, #118379, .T. ) ;
#108956 = DIRECTION ( 'NONE',  ( -0.000000000000000000, -1.000000000000000000, -0.000000000000000000 ) ) ;
#108957 = DIRECTION ( 'NONE',  ( -0.000000000000000000, 1.000000000000000000, -0.000000000000000000 ) ) ;
#108958 = ORIENTED_EDGE ( 'NONE', *, *, #18225, .T. ) ;
#108959 = CARTESIAN_POINT ( 'NONE',  ( 2.099999999999949463, 12.50000000000000000, -3.572213422710612374 ) ) ;
#108960 = CARTESIAN_POINT ( 'NONE',  ( -8.950000000000009948, 2.500000000000000000, -1.818653347947326138 ) ) ;
#108962 = ADVANCED_FACE ( 'NONE', ( #30570 ), #34172, .T. ) ;
#108961 = CARTESIAN_POINT ( 'NONE',  ( 7.899999999999924860, 2.500000000000000000, -4.430127018922202176 ) ) ;
#108963 = CARTESIAN_POINT ( 'NONE',  ( 7.049999999999926992, 2.500000000000000000, 2.165063509461097713 ) ) ;
#108964 = DIRECTION ( 'NONE',  ( -0.000000000000000000, 1.000000000000000000, -0.000000000000000000 ) ) ;
#108965 = ADVANCED_FACE ( 'NONE', ( #32507 ), #50204, .T. ) ;
#108966 = DIRECTION ( 'NONE',  ( 0.000000000000000000, 0.000000000000000000, 1.000000000000000000 ) ) ;
#108967 = DIRECTION ( 'NONE',  ( -0.000000000000000000, 1.000000000000000000, -0.000000000000000000 ) ) ;
#108968 = EDGE_CURVE ( 'NONE', #37478, #25981, #107315, .T. ) ;
#108969 = CIRCLE ( 'NONE', #10758, 0.06509327318403745899 ) ;
#108970 = EDGE_LOOP ( 'NONE', ( #107958, #24516 ) ) ;
#108971 = ORIENTED_EDGE ( 'NONE', *, *, #45603, .T. ) ;
#108972 = ORIENTED_EDGE ( 'NONE', *, *, #113563, .T. ) ;
#108973 = ORIENTED_EDGE ( 'NONE', *, *, #9112, .F. ) ;
#108974 = EDGE_LOOP ( 'NONE', ( #18298, #91067 ) ) ;
#108975 = CARTESIAN_POINT ( 'NONE',  ( -14.34999999999998543, 12.50000000000000000, 2.576566944158914740 ) ) ;
#108976 = EDGE_CURVE ( 'NONE', #128150, #108123, #124038, .T. ) ;
#108977 = CARTESIAN_POINT ( 'NONE',  ( 1.649999999999949729, 12.50000000000000000, 7.253104124594885960 ) ) ;
#108979 = ADVANCED_FACE ( 'NONE', ( #70469 ), #34271, .T. ) ;
#108978 = ORIENTED_EDGE ( 'NONE', *, *, #116178, .T. ) ;
#108980 = FACE_BOUND ( 'NONE', #56383, .T. ) ;
#108981 = CIRCLE ( 'NONE', #2361, 0.09999999999999982514 ) ;
#108982 = FACE_OUTER_BOUND ( 'NONE', #13629, .T. ) ;
#108983 = EDGE_CURVE ( 'NONE', #33136, #103573, #31207, .T. ) ;
#108984 = AXIS2_PLACEMENT_3D ( 'NONE', #47743, #90215, #127586 ) ;
#108985 = ADVANCED_FACE ( 'NONE', ( #22031 ), #89465, .T. ) ;
#108986 = ADVANCED_FACE ( 'NONE', ( #61302 ), #55184, .T. ) ;
#108987 = DIRECTION ( 'NONE',  ( -0.000000000000000000, -1.000000000000000000, -0.000000000000000000 ) ) ;
#108988 = LINE ( 'NONE', #19993, #30375 ) ;
#108989 = CARTESIAN_POINT ( 'NONE',  ( -8.550000000000007816, 12.50000000000000000, 6.083687093685482772 ) ) ;
#108990 = CARTESIAN_POINT ( 'NONE',  ( 5.599999999999933031, 2.500000000000000000, 0.3464101615137735735 ) ) ;
#108991 = DIRECTION ( 'NONE',  ( 0.000000000000000000, 1.000000000000000000, 0.000000000000000000 ) ) ;
#108992 = ORIENTED_EDGE ( 'NONE', *, *, #3647, .T. ) ;
#108993 = EDGE_CURVE ( 'NONE', #38652, #97177, #40380, .T. ) ;
#108994 = AXIS2_PLACEMENT_3D ( 'NONE', #95433, #26688, #66603 ) ;
#108995 = ORIENTED_EDGE ( 'NONE', *, *, #26685, .F. ) ;
#108996 = ORIENTED_EDGE ( 'NONE', *, *, #77893, .T. ) ;
#108997 = AXIS2_PLACEMENT_3D ( 'NONE', #44243, #84167, #34452 ) ;
#108998 = ORIENTED_EDGE ( 'NONE', *, *, #83900, .F. ) ;
#108999 = ORIENTED_EDGE ( 'NONE', *, *, #9053, .T. ) ;
#109000 = CONICAL_SURFACE ( 'NONE', #52583, 0.1000000000000002554, 0.003490658503988666988 ) ;
#109001 = DIRECTION ( 'NONE',  ( 0.000000000000000000, -0.000000000000000000, 1.000000000000000000 ) ) ;
#109002 = CARTESIAN_POINT ( 'NONE',  ( -15.79999999999998117, 2.500000000000000000, 0.000000000000000000 ) ) ;
#109003 = VERTEX_POINT ( 'NONE', #80303 ) ;
#109004 = DIRECTION ( 'NONE',  ( -0.000000000000000000, 1.000000000000000000, -0.000000000000000000 ) ) ;
#109005 = AXIS2_PLACEMENT_3D ( 'NONE', #50083, #88693, #89969 ) ;
#109006 = CARTESIAN_POINT ( 'NONE',  ( 0.8499999999999550138, 2.500000000000000000, -5.802370205355749988 ) ) ;
#109007 = DIRECTION ( 'NONE',  ( 0.000000000000000000, 0.000000000000000000, -1.000000000000000000 ) ) ;
#109008 = AXIS2_PLACEMENT_3D ( 'NONE', #126551, #36884, #25762 ) ;
#109009 = CIRCLE ( 'NONE', #90227, 0.06509327318403745899 ) ;
#109010 = CARTESIAN_POINT ( 'NONE',  ( 184.7760416670080588, 6.551208109652274736, 3.782341765625001351 ) ) ;
#109011 = DIRECTION ( 'NONE',  ( 0.000000000000000000, 0.000000000000000000, -1.000000000000000000 ) ) ;
#109012 = CARTESIAN_POINT ( 'NONE',  ( -8.750000000000012434, 2.500000000000000000, -5.702370205355745014 ) ) ;
#109013 = CARTESIAN_POINT ( 'NONE',  ( 7.499999999999960032, 2.500000000000000000, -2.276824562219559311E-15 ) ) ;
#109014 = ORIENTED_EDGE ( 'NONE', *, *, #64408, .T. ) ;
#109015 = CARTESIAN_POINT ( 'NONE',  ( 2.099999999999948574, 2.500000000000000000, 4.330127018922196314 ) ) ;
#109016 = ORIENTED_EDGE ( 'NONE', *, *, #90137, .F. ) ;
#109017 = EDGE_LOOP ( 'NONE', ( #96043, #36433, #55990, #69913 ) ) ;
#109018 = DIRECTION ( 'NONE',  ( 0.000000000000000000, 0.000000000000000000, -1.000000000000000000 ) ) ;
#109019 = DIRECTION ( 'NONE',  ( 0.000000000000000000, 0.000000000000000000, -1.000000000000000000 ) ) ;
#109020 = FACE_OUTER_BOUND ( 'NONE', #45667, .T. ) ;
#109021 = EDGE_LOOP ( 'NONE', ( #38966, #74591 ) ) ;
#109022 = EDGE_LOOP ( 'NONE', ( #93216, #124994, #43322, #16810 ) ) ;
#109023 = CARTESIAN_POINT ( 'NONE',  ( 185.0312500006828031, 9.429780353434619030E-16, -7.700000000000000178 ) ) ;
#109024 = EDGE_CURVE ( 'NONE', #56575, #20148, #113675, .T. ) ;
#109025 = CARTESIAN_POINT ( 'NONE',  ( -1.450000000000035927, 2.500000000000000000, -1.718653347947326049 ) ) ;
#109027 = CARTESIAN_POINT ( 'NONE',  ( 179.5000000000000000, 1.375000000000000222, 6.000000000000000000 ) ) ;
#109026 = AXIS2_PLACEMENT_3D ( 'NONE', #119593, #69868, #101253 ) ;
#109028 = ORIENTED_EDGE ( 'NONE', *, *, #62027, .T. ) ;
#109029 = CIRCLE ( 'NONE', #52606, 8.699999999999999289 ) ;
#109030 = CIRCLE ( 'NONE', #86043, 0.06509327318403745899 ) ;
#109031 = CARTESIAN_POINT ( 'NONE',  ( 184.5000000000000000, 0.000000000000000000, 7.700000000000000178 ) ) ;
#109032 = ORIENTED_EDGE ( 'NONE', *, *, #120950, .T. ) ;
#109033 = CARTESIAN_POINT ( 'NONE',  ( -10.85000000000000142, 12.50000000000000000, 6.430097255199259010 ) ) ;
#109034 = ORIENTED_EDGE ( 'NONE', *, *, #40367, .F. ) ;
#109035 = DIRECTION ( 'NONE',  ( -0.000000000000000000, -1.000000000000000000, -0.000000000000000000 ) ) ;
#109036 = CIRCLE ( 'NONE', #52615, 0.09999999999999982514 ) ;
#109037 = DIRECTION ( 'NONE',  ( -4.274815082592931898E-19, -0.9999939076577903929, -0.003490651415223739937 ) ) ;
#109038 = CARTESIAN_POINT ( 'NONE',  ( 115.5000000000000000, 5.000000000000000000, -4.999999999999997335 ) ) ;
#109039 = EDGE_CURVE ( 'NONE', #5490, #3622, #82388, .T. ) ;
#109040 = LINE ( 'NONE', #129379, #25012 ) ;
#109041 = VERTEX_POINT ( 'NONE', #61949 ) ;
#109042 = AXIS2_PLACEMENT_3D ( 'NONE', #61348, #101265, #11595 ) ;
#109043 = LINE ( 'NONE', #99263, #7033 ) ;
#109044 = ORIENTED_EDGE ( 'NONE', *, *, #205, .T. ) ;
#109045 = ORIENTED_EDGE ( 'NONE', *, *, #95557, .F. ) ;
#109046 = DIRECTION ( 'NONE',  ( -4.274815082592931898E-19, -0.9999939076577903929, -0.003490651415223739937 ) ) ;
#109047 = DIRECTION ( 'NONE',  ( -0.000000000000000000, 1.000000000000000000, -0.000000000000000000 ) ) ;
#109048 = CARTESIAN_POINT ( 'NONE',  ( -11.84999999999999787, 12.50000000000000000, -2.446380397790836270 ) ) ;
#109049 = CARTESIAN_POINT ( 'NONE',  ( 7.699999999999922018, 2.500000000000000000, 0.3464101615137735735 ) ) ;
#109050 = CARTESIAN_POINT ( 'NONE',  ( 13.54999999999989768, 12.50000000000000000, -2.446380397790840266 ) ) ;
#109051 = DIRECTION ( 'NONE',  ( 0.000000000000000000, -0.000000000000000000, 1.000000000000000000 ) ) ;
#109052 = PLANE ( 'NONE',  #36365 ) ;
#109053 = DIRECTION ( 'NONE',  ( 0.000000000000000000, 1.000000000000000000, 0.000000000000000000 ) ) ;
#109054 = CARTESIAN_POINT ( 'NONE',  ( 7.899999999999924860, 12.50000000000000000, -5.022947341949754119 ) ) ;
#109055 = CIRCLE ( 'NONE', #127954, 0.1000000000000002554 ) ;
#109056 = AXIS2_PLACEMENT_3D ( 'NONE', #97640, #80589, #108099 ) ;
#109057 = EDGE_CURVE ( 'NONE', #68357, #126539, #10264, .T. ) ;
#109058 = VERTEX_POINT ( 'NONE', #41679 ) ;
#109059 = DIRECTION ( 'NONE',  ( -4.274815082592931898E-19, -0.9999939076577903929, -0.003490651415223739937 ) ) ;
#109060 = CARTESIAN_POINT ( 'NONE',  ( -7.500000000000001776, 2.500000000000000000, -9.999999999999998224 ) ) ;
#109061 = DIRECTION ( 'NONE',  ( 0.000000000000000000, -0.9999939076577903929, 0.003490651415223739937 ) ) ;
#109062 = DIRECTION ( 'NONE',  ( 0.000000000000000000, -0.000000000000000000, 1.000000000000000000 ) ) ;
#109063 = CARTESIAN_POINT ( 'NONE',  ( -9.600000000000006750, 2.500000000000000000, 0.6928203230275494784 ) ) ;
#109064 = CONICAL_SURFACE ( 'NONE', #40149, 0.1000000000000000472, 0.003490658503988666988 ) ;
#109065 = EDGE_CURVE ( 'NONE', #38979, #87148, #72414, .T. ) ;
#109066 = CIRCLE ( 'NONE', #40150, 0.09999999999999982514 ) ;
#109067 = ORIENTED_EDGE ( 'NONE', *, *, #111124, .F. ) ;
#109068 = CARTESIAN_POINT ( 'NONE',  ( -8.350000000000012079, 2.500000000000000000, -1.372243186433550033 ) ) ;
#109069 = AXIS2_PLACEMENT_3D ( 'NONE', #78671, #87811, #28924 ) ;
#109070 = AXIS2_PLACEMENT_3D ( 'NONE', #33123, #73025, #112953 ) ;
#109071 = VECTOR ( 'NONE', #13218, 1000.000000000000000 ) ;
#109072 = DIRECTION ( 'NONE',  ( 0.000000000000000000, 0.000000000000000000, -1.000000000000000000 ) ) ;
#109074 = ORIENTED_EDGE ( 'NONE', *, *, #3459, .F. ) ;
#109073 = DIRECTION ( 'NONE',  ( 0.000000000000000000, 0.000000000000000000, -1.000000000000000000 ) ) ;
#109075 = EDGE_CURVE ( 'NONE', #47875, #29014, #15452, .T. ) ;
#109076 = EDGE_CURVE ( 'NONE', #1255, #123959, #29906, .T. ) ;
#109077 = EDGE_CURVE ( 'NONE', #32548, #124869, #25943, .T. ) ;
#109078 = EDGE_CURVE ( 'NONE', #37781, #14798, #122164, .T. ) ;
#109079 = EDGE_CURVE ( 'NONE', #122539, #22326, #12172, .T. ) ;
#109080 = VECTOR ( 'NONE', #16683, 1000.000000000000000 ) ;
#109081 = ORIENTED_EDGE ( 'NONE', *, *, #34539, .F. ) ;
#109082 = DIRECTION ( 'NONE',  ( 0.000000000000000000, 1.000000000000000000, 0.000000000000000000 ) ) ;
#109083 = VERTEX_POINT ( 'NONE', #35074 ) ;
#109084 = ORIENTED_EDGE ( 'NONE', *, *, #89057, .F. ) ;
#109085 = VECTOR ( 'NONE', #35586, 1000.000000000000000 ) ;
#109086 = ORIENTED_EDGE ( 'NONE', *, *, #27403, .F. ) ;
#109087 = VECTOR ( 'NONE', #123203, 1000.000000000000000 ) ;
#109088 = CARTESIAN_POINT ( 'NONE',  ( -6.650000000000014566, 2.500000000000000000, 2.165063509461097713 ) ) ;
#109089 = EDGE_CURVE ( 'NONE', #43890, #51917, #88630, .T. ) ;
#109090 = CIRCLE ( 'NONE', #42312, 0.06509327318403743123 ) ;
#109091 = CARTESIAN_POINT ( 'NONE',  ( 19.61395058415646986, 2.556813634648396505, -4.305699210822436562 ) ) ;
#109092 = DIRECTION ( 'NONE',  ( 0.000000000000000000, 0.000000000000000000, 1.000000000000000000 ) ) ;
#109093 = ADVANCED_FACE ( 'NONE', ( #13468 ), #23796, .T. ) ;
#109094 = CARTESIAN_POINT ( 'NONE',  ( 16.32066102237061500, 2.500000000000000000, -4.877377760480841040 ) ) ;
#109096 = ORIENTED_EDGE ( 'NONE', *, *, #6395, .F. ) ;
#109095 = ADVANCED_FACE ( 'NONE', ( #74980 ), #9205, .T. ) ;
#109097 = PLANE ( 'NONE',  #44070 ) ;
#109098 = VERTEX_POINT ( 'NONE', #65133 ) ;
#109099 = DIRECTION ( 'NONE',  ( 0.000000000000000000, 0.000000000000000000, -1.000000000000000000 ) ) ;
#109100 = CARTESIAN_POINT ( 'NONE',  ( 19.21290572970781696, 2.587129408759358373, 2.394140119531668720 ) ) ;
#109101 = DIRECTION ( 'NONE',  ( 0.000000000000000000, 0.000000000000000000, 1.000000000000000000 ) ) ;
#109102 = DIRECTION ( 'NONE',  ( 0.000000000000000000, 0.000000000000000000, 1.000000000000000000 ) ) ;
#109103 = VERTEX_POINT ( 'NONE', #123426 ) ;
#109104 = ORIENTED_EDGE ( 'NONE', *, *, #97909, .T. ) ;
#109105 = EDGE_LOOP ( 'NONE', ( #121610, #33542 ) ) ;
#109106 = EDGE_LOOP ( 'NONE', ( #43093, #82377 ) ) ;
#109107 = EDGE_LOOP ( 'NONE', ( #78803, #88801, #120665, #86474 ) ) ;
#109108 = DIRECTION ( 'NONE',  ( 0.000000000000000000, 0.000000000000000000, 1.000000000000000000 ) ) ;
#109109 = DIRECTION ( 'NONE',  ( 0.000000000000000000, 0.000000000000000000, 1.000000000000000000 ) ) ;
#109110 = DIRECTION ( 'NONE',  ( 0.000000000000000000, -0.000000000000000000, 1.000000000000000000 ) ) ;
#109111 = FACE_BOUND ( 'NONE', #90642, .T. ) ;
#109112 = CARTESIAN_POINT ( 'NONE',  ( -8.350000000000012079, 2.500000000000000000, -2.757883832488654097 ) ) ;
#109113 = LINE ( 'NONE', #89498, #65153 ) ;
#109114 = CARTESIAN_POINT ( 'NONE',  ( 7.949999999999922018, 2.500000000000000000, -2.065063509461102065 ) ) ;
#109115 = LINE ( 'NONE', #1748, #110650 ) ;
#109116 = AXIS2_PLACEMENT_3D ( 'NONE', #107037, #67092, #47497 ) ;
#109117 = AXIS2_PLACEMENT_3D ( 'NONE', #30259, #79349, #29586 ) ;
#109119 = AXIS2_PLACEMENT_3D ( 'NONE', #64145, #83788, #43887 ) ;
#109118 = CARTESIAN_POINT ( 'NONE',  ( 8.749999999999957367, 2.500000000000000000, 2.165063509461097713 ) ) ;
#109120 = DIRECTION ( 'NONE',  ( 0.000000000000000000, -0.000000000000000000, 1.000000000000000000 ) ) ;
#109121 = DIRECTION ( 'NONE',  ( 0.000000000000000000, 0.000000000000000000, -1.000000000000000000 ) ) ;
#109122 = EDGE_CURVE ( 'NONE', #47582, #37369, #115814, .T. ) ;
#109123 = AXIS2_PLACEMENT_3D ( 'NONE', #20362, #31473, #40670 ) ;
#109125 = DIRECTION ( 'NONE',  ( 0.000000000000000000, 1.000000000000000000, 0.000000000000000000 ) ) ;
#109124 = CIRCLE ( 'NONE', #33936, 0.1000000000000002554 ) ;
#109126 = EDGE_CURVE ( 'NONE', #16861, #69482, #59409, .T. ) ;
#109127 = AXIS2_PLACEMENT_3D ( 'NONE', #113215, #13069, #53028 ) ;
#109128 = ORIENTED_EDGE ( 'NONE', *, *, #128060, .T. ) ;
#109129 = ORIENTED_EDGE ( 'NONE', *, *, #20602, .T. ) ;
#109130 = ORIENTED_EDGE ( 'NONE', *, *, #85142, .F. ) ;
#109131 = ORIENTED_EDGE ( 'NONE', *, *, #40631, .F. ) ;
#109132 = AXIS2_PLACEMENT_3D ( 'NONE', #76193, #123989, #15956 ) ;
#109133 = DIRECTION ( 'NONE',  ( -0.000000000000000000, 1.000000000000000000, -0.000000000000000000 ) ) ;
#109134 = VECTOR ( 'NONE', #44731, 1000.000000000000000 ) ;
#109135 = DIRECTION ( 'NONE',  ( -0.000000000000000000, -1.000000000000000000, -0.000000000000000000 ) ) ;
#109136 = ADVANCED_FACE ( 'NONE', ( #95271 ), #83524, .T. ) ;
#109137 = FACE_BOUND ( 'NONE', #41178, .T. ) ;
#109138 = CIRCLE ( 'NONE', #63192, 0.06509327318403745899 ) ;
#109139 = DIRECTION ( 'NONE',  ( 0.000000000000000000, 1.000000000000000000, 0.000000000000000000 ) ) ;
#109140 = ADVANCED_FACE ( 'NONE', ( #84137 ), #73964, .T. ) ;
#109141 = ADVANCED_FACE ( 'NONE', ( #92687 ), #93977, .T. ) ;
#109142 = EDGE_LOOP ( 'NONE', ( #8103, #58969, #113927, #46662 ) ) ;
#109143 = CARTESIAN_POINT ( 'NONE',  ( 12.89999999999989733, 2.500000000000000000, -0.1000000000000023925 ) ) ;
#109144 = CARTESIAN_POINT ( 'NONE',  ( -4.600000000000024514, 12.50000000000000000, 3.637306695894644726 ) ) ;
#109145 = DIRECTION ( 'NONE',  ( 0.000000000000000000, 1.000000000000000000, 0.000000000000000000 ) ) ;
#109146 = PLANE ( 'NONE',  #87678 ) ;
#109147 = CARTESIAN_POINT ( 'NONE',  ( 4.599999999999936584, 12.50000000000000000, 4.330127018922196314 ) ) ;
#109148 = ORIENTED_EDGE ( 'NONE', *, *, #34224, .F. ) ;
#109149 = CARTESIAN_POINT ( 'NONE',  ( 0.8499999999999545697, 2.500000000000000000, -1.372243186433550033 ) ) ;
#109150 = ADVANCED_FACE ( 'NONE', ( #105064 ), #126291, .T. ) ;
#109151 = EDGE_LOOP ( 'NONE', ( #28702, #105319, #59297, #82492 ) ) ;
#109152 = ORIENTED_EDGE ( 'NONE', *, *, #111733, .T. ) ;
#109153 = DIRECTION ( 'NONE',  ( 0.000000000000000000, 0.000000000000000000, 1.000000000000000000 ) ) ;
#109154 = DIRECTION ( 'NONE',  ( 0.000000000000000000, -0.9999939076577903929, 0.003490651415223739937 ) ) ;
#109155 = EDGE_LOOP ( 'NONE', ( #75547, #10053 ) ) ;
#109156 = AXIS2_PLACEMENT_3D ( 'NONE', #108919, #89934, #91235 ) ;
#109157 = DIRECTION ( 'NONE',  ( -4.274815082592931898E-19, -0.9999939076577903929, -0.003490651415223739937 ) ) ;
#109158 = CARTESIAN_POINT ( 'NONE',  ( -4.200000000000025935, 2.500000000000000000, -2.385244779468109755E-15 ) ) ;
#109159 = VERTEX_POINT ( 'NONE', #125369 ) ;
#109160 = PLANE ( 'NONE',  #61979 ) ;
#109161 = EDGE_LOOP ( 'NONE', ( #57321, #60322, #65798, #106960 ) ) ;
#109162 = CARTESIAN_POINT ( 'NONE',  ( 11.24999999999994493, 2.500000000000000000, 6.395190528383296602 ) ) ;
#109163 = EDGE_CURVE ( 'NONE', #27375, #118968, #30063, .T. ) ;
#109164 = CIRCLE ( 'NONE', #113384, 0.5000000000000000000 ) ;
#109165 = EDGE_LOOP ( 'NONE', ( #842, #111987, #64378, #54406 ) ) ;
#109166 = CARTESIAN_POINT ( 'NONE',  ( 186.5729166673494888, 4.445597072760099522, -7.700000000000035705 ) ) ;
#109167 = FACE_BOUND ( 'NONE', #36708, .T. ) ;
#109168 = AXIS2_PLACEMENT_3D ( 'NONE', #52504, #121897, #74735 ) ;
#109169 = EDGE_LOOP ( 'NONE', ( #112335, #106921 ) ) ;
#109170 = CIRCLE ( 'NONE', #69467, 0.06509327318403745899 ) ;
#109171 = CARTESIAN_POINT ( 'NONE',  ( -8.950000000000006395, 2.500000000000000000, 6.941600689897073018 ) ) ;
#109172 = ORIENTED_EDGE ( 'NONE', *, *, #53121, .F. ) ;
#109173 = DIRECTION ( 'NONE',  ( -0.000000000000000000, 1.000000000000000000, -0.000000000000000000 ) ) ;
#109174 = CARTESIAN_POINT ( 'NONE',  ( -8.150000000000014566, 12.50000000000000000, -6.776507416713036136 ) ) ;
#109175 = FACE_OUTER_BOUND ( 'NONE', #8208, .T. ) ;
#109176 = DIRECTION ( 'NONE',  ( 0.000000000000000000, 0.000000000000000000, 1.000000000000000000 ) ) ;
#109177 = CARTESIAN_POINT ( 'NONE',  ( 17.28960762337857915, 1.567482926518815267, -5.035524966326118346 ) ) ;
#109178 = AXIS2_PLACEMENT_3D ( 'NONE', #48113, #119405, #29754 ) ;
#109179 = ORIENTED_EDGE ( 'NONE', *, *, #68764, .T. ) ;
#109180 = ORIENTED_EDGE ( 'NONE', *, *, #79556, .F. ) ;
#109181 = VECTOR ( 'NONE', #51844, 1000.000000000000000 ) ;
#109182 = EDGE_LOOP ( 'NONE', ( #127545, #78689 ) ) ;
#109183 = CARTESIAN_POINT ( 'NONE',  ( -3.950000000000026379, 2.500000000000000000, 6.841600689897072485 ) ) ;
#109184 = EDGE_CURVE ( 'NONE', #104949, #66592, #73676, .T. ) ;
#109186 = AXIS2_PLACEMENT_3D ( 'NONE', #39218, #49026, #109200 ) ;
#109185 = DIRECTION ( 'NONE',  ( 0.000000000000000000, -0.9999939076577903929, 0.003490651415223739937 ) ) ;
#109187 = AXIS2_PLACEMENT_3D ( 'NONE', #17764, #48528, #37434 ) ;
#109188 = AXIS2_PLACEMENT_3D ( 'NONE', #63637, #32260, #2767 ) ;
#109189 = CARTESIAN_POINT ( 'NONE',  ( 15.39999999999989200, 2.500000000000000000, -0.5928203230275542746 ) ) ;
#109191 = ORIENTED_EDGE ( 'NONE', *, *, #35425, .F. ) ;
#109190 = EDGE_LOOP ( 'NONE', ( #88928, #23015 ) ) ;
#109192 = ORIENTED_EDGE ( 'NONE', *, *, #119476, .F. ) ;
#109193 = CARTESIAN_POINT ( 'NONE',  ( -1.250000000000001554, 2.500000000000000000, 2.265063509461097357 ) ) ;
#109194 = CONICAL_SURFACE ( 'NONE', #46498, 0.09999999999999982514, 0.003490658503988666988 ) ;
#109195 = CARTESIAN_POINT ( 'NONE',  ( 1.049999999999953637, 12.50000000000000000, -1.753560074763288679 ) ) ;
#109196 = CONTEXT_DEPENDENT_SHAPE_REPRESENTATION ( #91522, #6478 ) ;
#109197 = CARTESIAN_POINT ( 'NONE',  ( -2.700000000000029932, 12.50000000000000000, -0.2813168883297408329 ) ) ;
#109198 = CIRCLE ( 'NONE', #38215, 0.06509327318403745899 ) ;
#109199 = CARTESIAN_POINT ( 'NONE',  ( -1.050000000000037792, 2.500000000000000000, 6.148780366869520009 ) ) ;
#109200 = DIRECTION ( 'NONE',  ( 0.000000000000000000, -0.000000000000000000, 1.000000000000000000 ) ) ;
#109201 = CARTESIAN_POINT ( 'NONE',  ( 108.0000000000000142, 5.000000000000000000, 5.000000000000004441 ) ) ;
#109202 = FACE_OUTER_BOUND ( 'NONE', #1992, .T. ) ;
#109203 = ADVANCED_FACE ( 'NONE', ( #23952 ), #115523, .T. ) ;
#109204 = FACE_OUTER_BOUND ( 'NONE', #22951, .T. ) ;
#109205 = ORIENTED_EDGE ( 'NONE', *, *, #69836, .T. ) ;
#109206 = ORIENTED_EDGE ( 'NONE', *, *, #96126, .F. ) ;
#109207 = CARTESIAN_POINT ( 'NONE',  ( -0.4500000000000397571, 2.500000000000000000, -2.265063509461101798 ) ) ;
#109208 = DIRECTION ( 'NONE',  ( 0.000000000000000000, 0.000000000000000000, -1.000000000000000000 ) ) ;
#109209 = EDGE_LOOP ( 'NONE', ( #119798, #76985 ) ) ;
#109210 = EDGE_LOOP ( 'NONE', ( #118414, #20243 ) ) ;
#109211 = VECTOR ( 'NONE', #69468, 1000.000000000000000 ) ;
#109212 = CARTESIAN_POINT ( 'NONE',  ( 186.9010416670080303, -4.367472073101519747, 7.564683531249999149 ) ) ;
#109213 = DIRECTION ( 'NONE',  ( 1.000000000000000000, 0.000000000000000000, 0.000000000000000000 ) ) ;
#109214 = CARTESIAN_POINT ( 'NONE',  ( 3.949999999999938893, 2.500000000000000000, 6.148780366869520009 ) ) ;
#109215 = DIRECTION ( 'NONE',  ( 0.000000000000000000, 0.000000000000000000, -1.000000000000000000 ) ) ;
#109216 = CARTESIAN_POINT ( 'NONE',  ( -6.050000000000022027, 12.50000000000000000, -6.213873640053564351 ) ) ;
#109217 = VECTOR ( 'NONE', #72927, 1000.000000000000000 ) ;
#109218 = CARTESIAN_POINT ( 'NONE',  ( 1.249999999999952038, 12.50000000000000000, 2.792790559304612064 ) ) ;
#109219 = FACE_OUTER_BOUND ( 'NONE', #114735, .T. ) ;
#109220 = CIRCLE ( 'NONE', #42338, 0.06509327318403745899 ) ;
#109221 = VECTOR ( 'NONE', #117739, 1000.000000000000000 ) ;
#109222 = CARTESIAN_POINT ( 'NONE',  ( 5.399999999999935518, 2.500000000000000000, -4.230127018922201998 ) ) ;
#109223 = VECTOR ( 'NONE', #127585, 1000.000000000000000 ) ;
#109224 = ORIENTED_EDGE ( 'NONE', *, *, #72266, .T. ) ;
#109225 = VECTOR ( 'NONE', #19585, 1000.000000000000000 ) ;
#109226 = EDGE_CURVE ( 'NONE', #116825, #15903, #124073, .T. ) ;
#109227 = ORIENTED_EDGE ( 'NONE', *, *, #16173, .T. ) ;
#109228 = AXIS2_PLACEMENT_3D ( 'NONE', #76520, #73442, #125594 ) ;
#109229 = AXIS2_PLACEMENT_3D ( 'NONE', #96158, #34693, #75873 ) ;
#109230 = EDGE_LOOP ( 'NONE', ( #23345, #86225 ) ) ;
#109231 = ORIENTED_EDGE ( 'NONE', *, *, #52214, .F. ) ;
#109232 = DIRECTION ( 'NONE',  ( 0.000000000000000000, 1.000000000000000000, 0.000000000000000000 ) ) ;
#109233 = DIRECTION ( 'NONE',  ( 0.000000000000000000, 1.000000000000000000, 0.000000000000000000 ) ) ;
#109234 = CIRCLE ( 'NONE', #113452, 0.09999999999999999167 ) ;
#109235 = ADVANCED_FACE ( 'NONE', ( #44220 ), #13306, .T. ) ;
#109236 = EDGE_LOOP ( 'NONE', ( #76146, #54023, #85267, #29550 ) ) ;
#109237 = DIRECTION ( 'NONE',  ( 0.000000000000000000, 1.000000000000000000, 0.000000000000000000 ) ) ;
#109238 = CARTESIAN_POINT ( 'NONE',  ( 3.549999999999944755, 2.500000000000000000, -2.511473670974877948 ) ) ;
#109239 = DIRECTION ( 'NONE',  ( 0.000000000000000000, 1.000000000000000000, 0.000000000000000000 ) ) ;
#109241 = ORIENTED_EDGE ( 'NONE', *, *, #26699, .F. ) ;
#109240 = LINE ( 'NONE', #30725, #22440 ) ;
#109242 = ADVANCED_FACE ( 'NONE', ( #74333 ), #105358, .T. ) ;
#109243 = ADVANCED_FACE ( 'NONE', ( #14108 ), #124128, .T. ) ;
#109244 = EDGE_CURVE ( 'NONE', #104766, #41779, #63507, .T. ) ;
#109245 = CARTESIAN_POINT ( 'NONE',  ( 2.500000000000002220, -1.500000000000000000, -9.999999999999998224 ) ) ;
#109246 = EDGE_CURVE ( 'NONE', #102257, #90767, #55970, .T. ) ;
#109248 = FACE_OUTER_BOUND ( 'NONE', #66051, .T. ) ;
#109247 = AXIS2_PLACEMENT_3D ( 'NONE', #104915, #103661, #83994 ) ;
#109249 = ORIENTED_EDGE ( 'NONE', *, *, #12052, .T. ) ;
#109250 = EDGE_CURVE ( 'NONE', #11624, #9428, #108299, .T. ) ;
#109251 = ORIENTED_EDGE ( 'NONE', *, *, #120447, .T. ) ;
#109253 = VERTEX_POINT ( 'NONE', #126663 ) ;
#109252 = ADVANCED_FACE ( 'NONE', ( #127311 ), #44730, .T. ) ;
#109254 = VERTEX_POINT ( 'NONE', #106997 ) ;
#109255 = DIRECTION ( 'NONE',  ( 0.000000000000000000, 1.000000000000000000, 0.000000000000000000 ) ) ;
#109256 = EDGE_CURVE ( 'NONE', #96511, #109502, #101158, .T. ) ;
#109257 = ADVANCED_FACE ( 'NONE', ( #67058 ), #13401, .T. ) ;
#109259 = AXIS2_PLACEMENT_3D ( 'NONE', #84636, #34264, #22516 ) ;
#109258 = CARTESIAN_POINT ( 'NONE',  ( 7.899999999999924860, 2.500000000000000000, -5.022947341949754119 ) ) ;
#109260 = CARTESIAN_POINT ( 'NONE',  ( -0.8500000000000386136, 12.50000000000000000, 1.472243186433545459 ) ) ;
#109262 = EDGE_CURVE ( 'NONE', #58840, #73617, #32320, .T. ) ;
#109261 = CONICAL_SURFACE ( 'NONE', #109358, 0.1000000000000000472, 0.003490658503988666988 ) ;
#109263 = CIRCLE ( 'NONE', #90468, 0.06509327318403745899 ) ;
#109264 = EDGE_CURVE ( 'NONE', #73752, #63793, #97198, .T. ) ;
#109265 = ORIENTED_EDGE ( 'NONE', *, *, #55626, .T. ) ;
#109266 = CARTESIAN_POINT ( 'NONE',  ( 2.499999999999947153, 12.50000000000000000, -3.637306695894650055 ) ) ;
#109267 = DIRECTION ( 'NONE',  ( 0.000000000000000000, 1.000000000000000000, 0.000000000000000000 ) ) ;
#109268 = DIRECTION ( 'NONE',  ( 0.000000000000000000, 0.000000000000000000, -1.000000000000000000 ) ) ;
#109269 = LINE ( 'NONE', #127625, #63036 ) ;
#109271 = EDGE_CURVE ( 'NONE', #126334, #105882, #53230, .T. ) ;
#109270 = AXIS2_PLACEMENT_3D ( 'NONE', #57628, #75317, #36052 ) ;
#109272 = CONICAL_SURFACE ( 'NONE', #67486, 0.1000000000000002554, 0.003490658503988666988 ) ;
#109273 = AXIS2_PLACEMENT_3D ( 'NONE', #47211, #5970, #87755 ) ;
#109274 = ORIENTED_EDGE ( 'NONE', *, *, #8890, .F. ) ;
#109275 = DIRECTION ( 'NONE',  ( 0.000000000000000000, -0.000000000000000000, 1.000000000000000000 ) ) ;
#109276 = CIRCLE ( 'NONE', #115620, 0.1000000000000002554 ) ;
#109277 = ORIENTED_EDGE ( 'NONE', *, *, #49453, .T. ) ;
#109278 = ORIENTED_EDGE ( 'NONE', *, *, #35929, .T. ) ;
#109279 = CARTESIAN_POINT ( 'NONE',  ( 6.049999999999932321, 12.50000000000000000, 6.776507416713035248 ) ) ;
#109280 = DIRECTION ( 'NONE',  ( -0.000000000000000000, 1.000000000000000000, -0.000000000000000000 ) ) ;
#109281 = FACE_BOUND ( 'NONE', #40392, .T. ) ;
#109282 = FACE_OUTER_BOUND ( 'NONE', #51843, .T. ) ;
#109284 = CIRCLE ( 'NONE', #23506, 0.09999999999999982514 ) ;
#109283 = DIRECTION ( 'NONE',  ( 0.000000000000000000, 1.000000000000000000, 0.000000000000000000 ) ) ;
#109286 = DIRECTION ( 'NONE',  ( 0.000000000000000000, 0.000000000000000000, 1.000000000000000000 ) ) ;
#109285 = AXIS2_PLACEMENT_3D ( 'NONE', #126378, #66792, #7879 ) ;
#109287 = CIRCLE ( 'NONE', #86286, 0.06509327318403745899 ) ;
#109288 = CIRCLE ( 'NONE', #52864, 0.1000000000000002554 ) ;
#109289 = ORIENTED_EDGE ( 'NONE', *, *, #127267, .T. ) ;
#109290 = FACE_OUTER_BOUND ( 'NONE', #6097, .T. ) ;
#109291 = PLANE ( 'NONE',  #40613 ) ;
#109292 = CARTESIAN_POINT ( 'NONE',  ( 2.899999999999946620, 2.500000000000000000, 0.7928203230275495672 ) ) ;
#109293 = AXIS2_PLACEMENT_3D ( 'NONE', #20779, #108503, #58770 ) ;
#109294 = CARTESIAN_POINT ( 'NONE',  ( -10.60000000000000142, 2.500000000000000000, -0.3464101615137782364 ) ) ;
#109295 = ORIENTED_EDGE ( 'NONE', *, *, #16603, .T. ) ;
#109296 = FACE_OUTER_BOUND ( 'NONE', #110584, .T. ) ;
#109297 = DIRECTION ( 'NONE',  ( -0.000000000000000000, 1.000000000000000000, -0.000000000000000000 ) ) ;
#109298 = CIRCLE ( 'NONE', #36158, 0.06509327318403745899 ) ;
#109299 = VERTEX_POINT ( 'NONE', #58577 ) ;
#109300 = ORIENTED_EDGE ( 'NONE', *, *, #17137, .T. ) ;
#109301 = CARTESIAN_POINT ( 'NONE',  ( -11.64999999999999680, 12.50000000000000000, -7.188010851410850499 ) ) ;
#109302 = LINE ( 'NONE', #59597, #84068 ) ;
#109303 = FACE_BOUND ( 'NONE', #44384, .T. ) ;
#109304 = DIRECTION ( 'NONE',  ( -0.000000000000000000, 1.000000000000000000, -0.000000000000000000 ) ) ;
#109305 = ADVANCED_FACE ( 'NONE', ( #36363 ), #126376, .T. ) ;
#109306 = CARTESIAN_POINT ( 'NONE',  ( -6.250000000000017764, 2.500000000000000000, 2.957883832488649389 ) ) ;
#109307 = ADVANCED_FACE ( 'NONE', ( #87363 ), #120031, .T. ) ;
#109309 = VERTEX_POINT ( 'NONE', #37646 ) ;
#109308 = VECTOR ( 'NONE', #79284, 1000.000000000000000 ) ;
#109311 = AXIS2_PLACEMENT_3D ( 'NONE', #15695, #23599, #84459 ) ;
#109310 = LINE ( 'NONE', #77909, #94741 ) ;
#109312 = CARTESIAN_POINT ( 'NONE',  ( 184.2500000000000000, 9.429780353434619030E-16, -7.700000000000000178 ) ) ;
#109313 = ORIENTED_EDGE ( 'NONE', *, *, #85031, .T. ) ;
#109314 = CARTESIAN_POINT ( 'NONE',  ( -3.950000000000029932, 2.500000000000000000, -6.148780366869526226 ) ) ;
#109315 = DIRECTION ( 'NONE',  ( 0.000000000000000000, 1.000000000000000000, 0.000000000000000000 ) ) ;
#109316 = ADVANCED_FACE ( 'NONE', ( #48103 ), #107668, .T. ) ;
#109317 = VECTOR ( 'NONE', #17485, 1000.000000000000000 ) ;
#109318 = AXIS2_PLACEMENT_3D ( 'NONE', #127040, #9824, #34957 ) ;
#109319 = AXIS2_PLACEMENT_3D ( 'NONE', #19515, #110479, #18221 ) ;
#109320 = CIRCLE ( 'NONE', #69613, 0.09999999999999982514 ) ;
#109321 = DIRECTION ( 'NONE',  ( 0.000000000000000000, 1.000000000000000000, 0.000000000000000000 ) ) ;
#109322 = CARTESIAN_POINT ( 'NONE',  ( -7.050000000000016698, 12.50000000000000000, -6.495190528383302464 ) ) ;
#109323 = AXIS2_PLACEMENT_3D ( 'NONE', #16938, #78505, #86351 ) ;
#109325 = ORIENTED_EDGE ( 'NONE', *, *, #68644, .T. ) ;
#109324 = CONICAL_SURFACE ( 'NONE', #75875, 0.1000000000000000472, 0.003490658503988666988 ) ;
#109326 = AXIS2_PLACEMENT_3D ( 'NONE', #60496, #100402, #91871 ) ;
#109327 = CARTESIAN_POINT ( 'NONE',  ( 7.699999999999925571, 12.50000000000000000, -4.611443907251940644 ) ) ;
#109328 = CARTESIAN_POINT ( 'NONE',  ( -11.84999999999999609, 2.500000000000000000, 1.718653347947321386 ) ) ;
#109329 = CIRCLE ( 'NONE', #67546, 0.09999999999999982514 ) ;
#109330 = CARTESIAN_POINT ( 'NONE',  ( 10.39999999999991509, 2.500000000000000000, -0.6928203230275542523 ) ) ;
#109332 = EDGE_LOOP ( 'NONE', ( #126043, #83572 ) ) ;
#109331 = AXIS2_PLACEMENT_3D ( 'NONE', #81052, #73157, #22144 ) ;
#109333 = EDGE_LOOP ( 'NONE', ( #58450, #114217, #99738, #19871 ) ) ;
#109334 = CARTESIAN_POINT ( 'NONE',  ( 17.50982737979238735, 2.500000000000000000, 4.074750942089363726 ) ) ;
#109335 = VECTOR ( 'NONE', #29555, 1000.000000000000000 ) ;
#109336 = VERTEX_POINT ( 'NONE', #95905 ) ;
#109337 = FACE_OUTER_BOUND ( 'NONE', #16054, .T. ) ;
#109338 = CARTESIAN_POINT ( 'NONE',  ( 87.50000000000002842, -7.402262750143065340, -1.385127402881715764 ) ) ;
#109339 = CARTESIAN_POINT ( 'NONE',  ( -0.6000000000000388356, 12.50000000000000000, 4.676537180435972552 ) ) ;
#109340 = EDGE_LOOP ( 'NONE', ( #3236, #41597 ) ) ;
#109341 = DIRECTION ( 'NONE',  ( 0.000000000000000000, 0.000000000000000000, 1.000000000000000000 ) ) ;
#109342 = FACE_OUTER_BOUND ( 'NONE', #45573, .T. ) ;
#109343 = DIRECTION ( 'NONE',  ( -0.000000000000000000, 1.000000000000000000, -0.000000000000000000 ) ) ;
#109344 = CARTESIAN_POINT ( 'NONE',  ( 184.5000000000000000, -7.430520870378829024, -1.418378131116527108 ) ) ;
#109345 = DIRECTION ( 'NONE',  ( 0.000000000000000000, 1.000000000000000000, 0.000000000000000000 ) ) ;
#109346 = CARTESIAN_POINT ( 'NONE',  ( -8.550000000000007816, 12.50000000000000000, 6.148780366869520009 ) ) ;
#109347 = CIRCLE ( 'NONE', #50868, 0.06509327318403745899 ) ;
#109348 = ORIENTED_EDGE ( 'NONE', *, *, #75144, .F. ) ;
#109349 = VERTEX_POINT ( 'NONE', #26526 ) ;
#109350 = DIRECTION ( 'NONE',  ( -0.000000000000000000, 1.000000000000000000, -0.000000000000000000 ) ) ;
#109351 = ORIENTED_EDGE ( 'NONE', *, *, #29892, .F. ) ;
#109352 = CARTESIAN_POINT ( 'NONE',  ( -7.300000000000018474, 2.500000000000000000, 0.3464101615137735735 ) ) ;
#109354 = ORIENTED_EDGE ( 'NONE', *, *, #101781, .F. ) ;
#109353 = EDGE_LOOP ( 'NONE', ( #82070, #101423 ) ) ;
#109355 = VERTEX_POINT ( 'NONE', #88665 ) ;
#109356 = PLANE ( 'NONE',  #1925 ) ;
#109357 = CIRCLE ( 'NONE', #59206, 0.06509327318403745899 ) ;
#109358 = AXIS2_PLACEMENT_3D ( 'NONE', #964, #63105, #40924 ) ;
#109359 = DIRECTION ( 'NONE',  ( 0.000000000000000000, 1.000000000000000000, 0.000000000000000000 ) ) ;
#109360 = CARTESIAN_POINT ( 'NONE',  ( 1.899999999999949507, 2.500000000000000000, 4.676537180435972552 ) ) ;
#109361 = SHAPE_REPRESENTATION_RELATIONSHIP ( 'NONE' , 'NONE' ,  #5058, #78940 ) ;
#109362 = CARTESIAN_POINT ( 'NONE',  ( 13.54999999999990123, 2.500000000000000000, 1.818653347947321475 ) ) ;
#109363 = PLANE ( 'NONE',  #104505 ) ;
#109364 = DIRECTION ( 'NONE',  ( 0.000000000000000000, 0.000000000000000000, 1.000000000000000000 ) ) ;
#109365 = ADVANCED_FACE ( 'NONE', ( #87995 ), #19771, .T. ) ;
#109366 = PLANE ( 'NONE',  #16222 ) ;
#109367 = CARTESIAN_POINT ( 'NONE',  ( 0.5999999999999621192, 2.500000000000000000, 0.3464101615137758494 ) ) ;
#109368 = EDGE_CURVE ( 'NONE', #35141, #117766, #118120, .T. ) ;
#109369 = AXIS2_PLACEMENT_3D ( 'NONE', #124280, #47016, #67245 ) ;
#109370 = AXIS2_PLACEMENT_3D ( 'NONE', #37116, #98578, #118241 ) ;
#109371 = CARTESIAN_POINT ( 'NONE',  ( -0.4500000000000402012, 2.500000000000000000, 2.165063509461097713 ) ) ;
#109372 = VERTEX_POINT ( 'NONE', #125997 ) ;
#109373 = AXIS2_PLACEMENT_3D ( 'NONE', #102105, #24673, #21610 ) ;
#109374 = ORIENTED_EDGE ( 'NONE', *, *, #53901, .T. ) ;
#109375 = VECTOR ( 'NONE', #123111, 1000.000000000000000 ) ;
#109376 = CARTESIAN_POINT ( 'NONE',  ( 7.699999999999923794, 12.50000000000000000, -3.983716857408426293 ) ) ;
#109377 = ORIENTED_EDGE ( 'NONE', *, *, #15312, .F. ) ;
#109378 = ADVANCED_FACE ( 'NONE', ( #128624 ), #38960, .T. ) ;
#109379 = ORIENTED_EDGE ( 'NONE', *, *, #80297, .F. ) ;
#109380 = DIRECTION ( 'NONE',  ( 0.000000000000000000, 0.000000000000000000, -1.000000000000000000 ) ) ;
#109381 = CARTESIAN_POINT ( 'NONE',  ( 186.9895833340161744, -4.445597072760123503, -7.699999999999989519 ) ) ;
#109382 = CARTESIAN_POINT ( 'NONE',  ( -0.4000000000000396572, 2.500000000000000000, 4.330127018922196314 ) ) ;
#109383 = CARTESIAN_POINT ( 'NONE',  ( -10.40000000000000391, 2.500000000000000000, -3.637306695894645614 ) ) ;
#109384 = AXIS2_PLACEMENT_3D ( 'NONE', #18597, #119365, #127909 ) ;
#109385 = CIRCLE ( 'NONE', #92666, 0.06509327318403745899 ) ;
#109386 = CARTESIAN_POINT ( 'NONE',  ( 9.549999999999918998, 12.50000000000000000, -6.495190528383302464 ) ) ;
#109387 = ORIENTED_EDGE ( 'NONE', *, *, #7721, .F. ) ;
#109388 = ORIENTED_EDGE ( 'NONE', *, *, #85250, .T. ) ;
#109389 = CARTESIAN_POINT ( 'NONE',  ( 5.449999999999934452, 2.500000000000000000, 2.165063509461097713 ) ) ;
#109390 = ORIENTED_EDGE ( 'NONE', *, *, #124240, .F. ) ;
#109392 = EDGE_CURVE ( 'NONE', #111853, #1262, #23894, .T. ) ;
#109391 = FACE_OUTER_BOUND ( 'NONE', #60958, .T. ) ;
#109393 = EDGE_LOOP ( 'NONE', ( #3069, #122954 ) ) ;
#109394 = ORIENTED_EDGE ( 'NONE', *, *, #55447, .F. ) ;
#109395 = CARTESIAN_POINT ( 'NONE',  ( -6.900000000000015454, 2.500000000000000000, 4.083716857408420609 ) ) ;
#109396 = CARTESIAN_POINT ( 'NONE',  ( 12.49999999999990230, 12.50000000000000000, -0.6928203230275541413 ) ) ;
#109397 = EDGE_CURVE ( 'NONE', #72434, #18337, #92937, .T. ) ;
#109398 = PLANE ( 'NONE',  #19446 ) ;
#109399 = CARTESIAN_POINT ( 'NONE',  ( 6.649999999999930189, 2.500000000000000000, 5.802370205355744659 ) ) ;
#109400 = DIRECTION ( 'NONE',  ( 0.000000000000000000, 0.000000000000000000, 1.000000000000000000 ) ) ;
#109401 = ORIENTED_EDGE ( 'NONE', *, *, #64794, .T. ) ;
#109402 = CARTESIAN_POINT ( 'NONE',  ( 1.249999999999952038, 12.50000000000000000, 2.857883832488649301 ) ) ;
#109404 = AXIS2_PLACEMENT_3D ( 'NONE', #13080, #24219, #104063 ) ;
#109403 = DIRECTION ( 'NONE',  ( -0.000000000000000000, -1.000000000000000000, -0.000000000000000000 ) ) ;
#109405 = EDGE_CURVE ( 'NONE', #90044, #117253, #110869, .T. ) ;
#109406 = AXIS2_PLACEMENT_3D ( 'NONE', #8240, #67810, #86806 ) ;
#109407 = ADVANCED_FACE ( 'NONE', ( #42148 ), #9300, .T. ) ;
#109408 = CARTESIAN_POINT ( 'NONE',  ( -15.39999999999998082, 12.50000000000000000, 0.7579135962115892688 ) ) ;
#109409 = EDGE_CURVE ( 'NONE', #92182, #21147, #97038, .T. ) ;
#109410 = CARTESIAN_POINT ( 'NONE',  ( -13.74999999999995381, 12.50000000000000000, 2.165063509461101265 ) ) ;
#109411 = EDGE_CURVE ( 'NONE', #52245, #6156, #51085, .T. ) ;
#109412 = CARTESIAN_POINT ( 'NONE',  ( -3.100000000000028955, 12.50000000000000000, 3.918623584224383727 ) ) ;
#109413 = ORIENTED_EDGE ( 'NONE', *, *, #5101, .F. ) ;
#109414 = AXIS2_PLACEMENT_3D ( 'NONE', #35078, #114895, #63232 ) ;
#109415 = CIRCLE ( 'NONE', #96882, 0.1000000000000002554 ) ;
#109416 = AXIS2_PLACEMENT_3D ( 'NONE', #38511, #6412, #78438 ) ;
#109417 = ORIENTED_EDGE ( 'NONE', *, *, #73201, .T. ) ;
#109418 = AXIS2_PLACEMENT_3D ( 'NONE', #26613, #94065, #75696 ) ;
#109419 = EDGE_CURVE ( 'NONE', #44266, #74448, #3048, .T. ) ;
#109420 = AXIS2_PLACEMENT_3D ( 'NONE', #5399, #95080, #44694 ) ;
#109421 = LINE ( 'NONE', #19760, #63368 ) ;
#109422 = EDGE_CURVE ( 'NONE', #42047, #101516, #7134, .T. ) ;
#109423 = ORIENTED_EDGE ( 'NONE', *, *, #10409, .T. ) ;
#109424 = CARTESIAN_POINT ( 'NONE',  ( -4.150000000000025224, 12.50000000000000000, 7.188010851410848723 ) ) ;
#109425 = CARTESIAN_POINT ( 'NONE',  ( 8.299999999999922551, 12.50000000000000000, -4.395220292106239768 ) ) ;
#109426 = VECTOR ( 'NONE', #63215, 1000.000000000000000 ) ;
#109427 = CIRCLE ( 'NONE', #92702, 0.1000000000000002554 ) ;
#109428 = EDGE_CURVE ( 'NONE', #88657, #66180, #69666, .T. ) ;
#109429 = VECTOR ( 'NONE', #13262, 1000.000000000000000 ) ;
#109430 = VERTEX_POINT ( 'NONE', #71601 ) ;
#109431 = CARTESIAN_POINT ( 'NONE',  ( 4.999999999999971578, 12.50000000000000000, -2.276824562219559311E-15 ) ) ;
#109432 = DIRECTION ( 'NONE',  ( 0.000000000000000000, 0.000000000000000000, 1.000000000000000000 ) ) ;
#109433 = ADVANCED_FACE ( 'NONE', ( #111528 ), #31061, .T. ) ;
#109434 = DIRECTION ( 'NONE',  ( 0.000000000000000000, 1.000000000000000000, 0.000000000000000000 ) ) ;
#109435 = CARTESIAN_POINT ( 'NONE',  ( 4.149999999999939959, 12.50000000000000000, 2.857883832488649301 ) ) ;
#109436 = ADVANCED_FACE ( 'NONE', ( #129267 ), #13484, .T. ) ;
#109437 = DIRECTION ( 'NONE',  ( -1.000000000000000000, -0.000000000000000000, -0.000000000000000000 ) ) ;
#109438 = VERTEX_POINT ( 'NONE', #59229 ) ;
#109439 =( BOUNDED_CURVE ( )  B_SPLINE_CURVE ( 2, ( #95645, #112717, #83260, #103543, #114628, #124466, #35447 ),
 .UNSPECIFIED., .F., .F. ) 
 B_SPLINE_CURVE_WITH_KNOTS ( ( 3, 2, 2, 3 ),
 ( 0.000000000000000000, 0.02380952380952383249, 0.04761904761904766498, 0.07142857142857149400 ),
 .UNSPECIFIED. ) 
 CURVE ( )  GEOMETRIC_REPRESENTATION_ITEM ( )  RATIONAL_B_SPLINE_CURVE ( ( 1.000000000000000000, 0.8660254037844387076, 1.000000000000000000, 0.8660254037844387076, 1.000000000000000000, 0.8660254037844383745, 1.000000000000000444 ) ) 
 REPRESENTATION_ITEM ( '' )  );
#109440 = DIRECTION ( 'NONE',  ( 0.000000000000000000, 0.000000000000000000, -1.000000000000000000 ) ) ;
#109441 = DIRECTION ( 'NONE',  ( 0.000000000000000000, -0.000000000000000000, 1.000000000000000000 ) ) ;
#109442 = CARTESIAN_POINT ( 'NONE',  ( -0.6500000000000394351, 2.500000000000000000, 2.611473670974873151 ) ) ;
#109443 = AXIS2_PLACEMENT_3D ( 'NONE', #64207, #101566, #2701 ) ;
#109444 = VERTEX_POINT ( 'NONE', #119397 ) ;
#109445 = DIRECTION ( 'NONE',  ( 0.000000000000000000, 0.000000000000000000, -1.000000000000000000 ) ) ;
#109446 = ORIENTED_EDGE ( 'NONE', *, *, #74986, .F. ) ;
#109447 = FACE_OUTER_BOUND ( 'NONE', #51608, .T. ) ;
#109448 = CARTESIAN_POINT ( 'NONE',  ( 0.4499999999999552136, 12.50000000000000000, 6.495190528383297135 ) ) ;
#109449 = CARTESIAN_POINT ( 'NONE',  ( -12.49999999999999289, 12.50000000000000000, -5.088040615133788691 ) ) ;
#109450 = AXIS2_PLACEMENT_3D ( 'NONE', #62115, #22843, #71268 ) ;
#109451 = ORIENTED_EDGE ( 'NONE', *, *, #126707, .F. ) ;
#109452 = AXIS2_PLACEMENT_3D ( 'NONE', #57154, #57807, #88540 ) ;
#109453 = AXIS2_PLACEMENT_3D ( 'NONE', #33779, #63889, #55360 ) ;
#109454 = CARTESIAN_POINT ( 'NONE',  ( 5.599999999999931255, 2.500000000000000000, 4.676537180435972552 ) ) ;
#109455 = DIRECTION ( 'NONE',  ( 0.000000000000000000, 0.000000000000000000, -1.000000000000000000 ) ) ;
#109456 = ORIENTED_EDGE ( 'NONE', *, *, #95935, .T. ) ;
#109457 = DIRECTION ( 'NONE',  ( 0.000000000000000000, 0.000000000000000000, -1.000000000000000000 ) ) ;
#109458 = AXIS2_PLACEMENT_3D ( 'NONE', #19465, #128815, #80338 ) ;
#109459 = ORIENTED_EDGE ( 'NONE', *, *, #44375, .F. ) ;
#109460 = VECTOR ( 'NONE', #21322, 1000.000000000000000 ) ;
#109461 = CARTESIAN_POINT ( 'NONE',  ( -7.500000000000001776, 1.500000000000000000, 9.000000000000001776 ) ) ;
#109462 = AXIS2_PLACEMENT_3D ( 'NONE', #41906, #11778, #74419 ) ;
#109463 = EDGE_CURVE ( 'NONE', #11053, #4868, #109656, .T. ) ;
#109464 = ORIENTED_EDGE ( 'NONE', *, *, #75560, .F. ) ;
#109465 = CARTESIAN_POINT ( 'NONE',  ( 11.44999999999990870, 12.50000000000000000, -1.818653347947326138 ) ) ;
#109466 = CARTESIAN_POINT ( 'NONE',  ( -12.49999999999995914, 2.500000000000000000, -0.09999999999999815981 ) ) ;
#109467 = EDGE_CURVE ( 'NONE', #118617, #9793, #99784, .T. ) ;
#109468 = ORIENTED_EDGE ( 'NONE', *, *, #21342, .T. ) ;
#109469 = EDGE_LOOP ( 'NONE', ( #88439, #71717, #18131, #73524 ) ) ;
#109470 = CIRCLE ( 'NONE', #59328, 0.06509327318403745899 ) ;
#109471 = CARTESIAN_POINT ( 'NONE',  ( -7.100000000000014744, 2.500000000000000000, 4.330127018922196314 ) ) ;
#109472 = CARTESIAN_POINT ( 'NONE',  ( 10.64999999999990976, 2.500000000000000000, -6.248780366869526759 ) ) ;
#109473 = ORIENTED_EDGE ( 'NONE', *, *, #110819, .T. ) ;
#109474 = LINE ( 'NONE', #78083, #6995 ) ;
#109475 = FACE_OUTER_BOUND ( 'NONE', #7691, .T. ) ;
#109476 = CONICAL_SURFACE ( 'NONE', #82298, 0.1000000000000002554, 0.003490658503988666988 ) ;
#109478 = AXIS2_PLACEMENT_3D ( 'NONE', #71558, #1524, #51303 ) ;
#109477 = DIRECTION ( 'NONE',  ( 0.000000000000000000, 0.000000000000000000, 1.000000000000000000 ) ) ;
#109479 = VECTOR ( 'NONE', #75072, 1000.000000000000000 ) ;
#109480 = DIRECTION ( 'NONE',  ( -0.000000000000000000, -1.000000000000000000, -0.000000000000000000 ) ) ;
#109481 = CARTESIAN_POINT ( 'NONE',  ( 13.34999999999990017, 12.50000000000000000, 1.537336459617582918 ) ) ;
#109482 = CARTESIAN_POINT ( 'NONE',  ( 9.399999999999915090, 2.500000000000000000, 4.676537180435972552 ) ) ;
#109483 = CIRCLE ( 'NONE', #126207, 0.06509327318403745899 ) ;
#109484 = CARTESIAN_POINT ( 'NONE',  ( 5.199999999999931788, 2.500000000000000000, 4.576537180435972019 ) ) ;
#109485 = AXIS2_PLACEMENT_3D ( 'NONE', #44761, #74860, #13343 ) ;
#109486 = VERTEX_POINT ( 'NONE', #9465 ) ;
#109487 = ORIENTED_EDGE ( 'NONE', *, *, #104925, .F. ) ;
#109488 = VERTEX_POINT ( 'NONE', #12030 ) ;
#109489 = ORIENTED_EDGE ( 'NONE', *, *, #61233, .F. ) ;
#109490 = DIRECTION ( 'NONE',  ( 0.000000000000000000, 1.000000000000000000, 0.000000000000000000 ) ) ;
#109491 = DIRECTION ( 'NONE',  ( 0.000000000000000000, 1.000000000000000000, 0.000000000000000000 ) ) ;
#109492 = DIRECTION ( 'NONE',  ( 0.000000000000000000, 0.000000000000000000, -1.000000000000000000 ) ) ;
#109493 = ORIENTED_EDGE ( 'NONE', *, *, #97697, .T. ) ;
#109494 = FACE_BOUND ( 'NONE', #94852, .T. ) ;
#109495 = VERTEX_POINT ( 'NONE', #266 ) ;
#109496 = DIRECTION ( 'NONE',  ( -0.000000000000000000, -1.000000000000000000, -0.000000000000000000 ) ) ;
#109497 = DIRECTION ( 'NONE',  ( 0.000000000000000000, 0.000000000000000000, -1.000000000000000000 ) ) ;
#109498 = DIRECTION ( 'NONE',  ( 0.000000000000000000, 0.000000000000000000, 1.000000000000000000 ) ) ;
#109499 = FACE_OUTER_BOUND ( 'NONE', #88807, .T. ) ;
#109500 = DIRECTION ( 'NONE',  ( 0.000000000000000000, 0.000000000000000000, 1.000000000000000000 ) ) ;
#109501 = CARTESIAN_POINT ( 'NONE',  ( -9.600000000000008527, 2.500000000000000000, -3.537306695894645969 ) ) ;
#109502 = VERTEX_POINT ( 'NONE', #80143 ) ;
#109503 = DIRECTION ( 'NONE',  ( 0.000000000000000000, -0.9999939076577903929, 0.003490651415223739937 ) ) ;
#109504 = AXIS2_PLACEMENT_3D ( 'NONE', #121083, #21596, #92255 ) ;
#109505 = DIRECTION ( 'NONE',  ( -0.000000000000000000, 1.000000000000000000, -0.000000000000000000 ) ) ;
#109506 = PLANE ( 'NONE',  #91995 ) ;
#109507 = EDGE_CURVE ( 'NONE', #26903, #64905, #65728, .T. ) ;
#109508 = VECTOR ( 'NONE', #51983, 1000.000000000000000 ) ;
#109510 = VERTEX_POINT ( 'NONE', #51979 ) ;
#109509 = CONICAL_SURFACE ( 'NONE', #126231, 0.1000000000000002554, 0.003490658503988666988 ) ;
#109511 = ORIENTED_EDGE ( 'NONE', *, *, #98125, .F. ) ;
#109512 = ORIENTED_EDGE ( 'NONE', *, *, #45289, .T. ) ;
#109513 = AXIS2_PLACEMENT_3D ( 'NONE', #51966, #120692, #915 ) ;
#109514 = EDGE_LOOP ( 'NONE', ( #64051, #24100, #83390, #102365 ) ) ;
#109516 = AXIS2_PLACEMENT_3D ( 'NONE', #17414, #57361, #97282 ) ;
#109515 = DIRECTION ( 'NONE',  ( 0.000000000000000000, 1.000000000000000000, 0.000000000000000000 ) ) ;
#109517 = CIRCLE ( 'NONE', #52784, 0.1000000000000000472 ) ;
#109518 = DIRECTION ( 'NONE',  ( 0.000000000000000000, 0.000000000000000000, -1.000000000000000000 ) ) ;
#109520 = ORIENTED_EDGE ( 'NONE', *, *, #49242, .F. ) ;
#109519 = VERTEX_POINT ( 'NONE', #91893 ) ;
#109521 = ORIENTED_EDGE ( 'NONE', *, *, #22000, .T. ) ;
#109522 = CARTESIAN_POINT ( 'NONE',  ( 14.14999999999989733, 2.500000000000000000, 1.572243186433545548 ) ) ;
#109523 = EDGE_CURVE ( 'NONE', #72018, #125678, #86660, .T. ) ;
#109524 = AXIS2_PLACEMENT_3D ( 'NONE', #101389, #94778, #105240 ) ;
#109525 = CIRCLE ( 'NONE', #84479, 0.1000000000000000472 ) ;
#109526 = CIRCLE ( 'NONE', #53087, 0.1000000000000002554 ) ;
#109527 = CARTESIAN_POINT ( 'NONE',  ( 4.349999999999939249, 12.50000000000000000, 2.511473670974873507 ) ) ;
#109528 = FACE_OUTER_BOUND ( 'NONE', #14134, .T. ) ;
#109529 = DIRECTION ( 'NONE',  ( 0.000000000000000000, 1.000000000000000000, 0.000000000000000000 ) ) ;
#109530 = DIRECTION ( 'NONE',  ( -0.000000000000000000, 1.000000000000000000, -0.000000000000000000 ) ) ;
#109531 = PLANE ( 'NONE',  #51885 ) ;
#109532 = VECTOR ( 'NONE', #100216, 1000.000000000000000 ) ;
#109533 = EDGE_CURVE ( 'NONE', #125468, #70303, #76211, .T. ) ;
#109534 = CARTESIAN_POINT ( 'NONE',  ( -4.800000000000024691, 2.500000000000000000, 4.576537180435972019 ) ) ;
#109535 = EDGE_CURVE ( 'NONE', #25981, #37478, #5085, .T. ) ;
#109536 = ORIENTED_EDGE ( 'NONE', *, *, #107218, .F. ) ;
#109537 = CARTESIAN_POINT ( 'NONE',  ( -3.350000000000028511, 2.500000000000000000, 1.572243186433545548 ) ) ;
#109538 = ORIENTED_EDGE ( 'NONE', *, *, #112824, .F. ) ;
#109539 = ORIENTED_EDGE ( 'NONE', *, *, #54304, .T. ) ;
#109540 = EDGE_LOOP ( 'NONE', ( #71463, #58683, #19118, #46349 ) ) ;
#109541 = CARTESIAN_POINT ( 'NONE',  ( 6.449999999999933564, 12.50000000000000000, -6.841600689897078702 ) ) ;
#109542 = ORIENTED_EDGE ( 'NONE', *, *, #99287, .T. ) ;
#109543 = EDGE_CURVE ( 'NONE', #83720, #87809, #99196, .T. ) ;
#109544 = ORIENTED_EDGE ( 'NONE', *, *, #66111, .F. ) ;
#109545 = CIRCLE ( 'NONE', #875, 0.09999999999999982514 ) ;
#109546 = FACE_OUTER_BOUND ( 'NONE', #79379, .T. ) ;
#109547 = CARTESIAN_POINT ( 'NONE',  ( -8.750000000000012434, 2.500000000000000000, -5.802370205355744659 ) ) ;
#109548 = LINE ( 'NONE', #50612, #4016 ) ;
#109549 = CARTESIAN_POINT ( 'NONE',  ( 1.649999999999951505, 12.50000000000000000, -1.537336459617587581 ) ) ;
#109550 = DIRECTION ( 'NONE',  ( 0.000000000000000000, 1.000000000000000000, 0.000000000000000000 ) ) ;
#109551 = VERTEX_POINT ( 'NONE', #123916 ) ;
#109552 = CARTESIAN_POINT ( 'NONE',  ( 2.899999999999946620, 2.500000000000000000, -5.122947341949753763 ) ) ;
#109553 = AXIS2_PLACEMENT_3D ( 'NONE', #122216, #52817, #12868 ) ;
#109554 = AXIS2_PLACEMENT_3D ( 'NONE', #62926, #24939, #43308 ) ;
#109555 = ORIENTED_EDGE ( 'NONE', *, *, #58446, .F. ) ;
#109556 = DIRECTION ( 'NONE',  ( -0.000000000000000000, 1.000000000000000000, -0.000000000000000000 ) ) ;
#109557 = EDGE_LOOP ( 'NONE', ( #73901, #82508, #37933, #91542 ) ) ;
#109558 = DIRECTION ( 'NONE',  ( 0.000000000000000000, 0.000000000000000000, -1.000000000000000000 ) ) ;
#109559 = FACE_OUTER_BOUND ( 'NONE', #110976, .T. ) ;
#109560 = VERTEX_POINT ( 'NONE', #34279 ) ;
#109561 = FACE_OUTER_BOUND ( 'NONE', #61845, .T. ) ;
#109562 = DIRECTION ( 'NONE',  ( 0.000000000000000000, 1.000000000000000000, 0.000000000000000000 ) ) ;
#109563 = ORIENTED_EDGE ( 'NONE', *, *, #97152, .F. ) ;
#109564 = VECTOR ( 'NONE', #126593, 1000.000000000000000 ) ;
#109565 = AXIS2_PLACEMENT_3D ( 'NONE', #33137, #5571, #33759 ) ;
#109566 = EDGE_CURVE ( 'NONE', #100401, #109850, #74050, .T. ) ;
#109567 = DIRECTION ( 'NONE',  ( -0.000000000000000000, 1.000000000000000000, -0.000000000000000000 ) ) ;
#109568 = ORIENTED_EDGE ( 'NONE', *, *, #79414, .F. ) ;
#109569 = VERTEX_POINT ( 'NONE', #104291 ) ;
#109570 = DIRECTION ( 'NONE',  ( 0.000000000000000000, -0.000000000000000000, 1.000000000000000000 ) ) ;
#109571 = DIRECTION ( 'NONE',  ( -0.000000000000000000, 1.000000000000000000, -0.000000000000000000 ) ) ;
#109572 = EDGE_CURVE ( 'NONE', #122791, #91186, #90768, .T. ) ;
#109573 = DIRECTION ( 'NONE',  ( 0.000000000000000000, 0.000000000000000000, 1.000000000000000000 ) ) ;
#109574 = DIRECTION ( 'NONE',  ( -0.000000000000000000, 1.000000000000000000, -0.000000000000000000 ) ) ;
#109575 = EDGE_CURVE ( 'NONE', #80133, #26576, #78278, .T. ) ;
#109576 = DIRECTION ( 'NONE',  ( 0.000000000000000000, 1.000000000000000000, 0.000000000000000000 ) ) ;
#109577 = EDGE_LOOP ( 'NONE', ( #1911, #120337 ) ) ;
#109578 = CIRCLE ( 'NONE', #38585, 0.1000000000000002554 ) ;
#109579 = CONICAL_SURFACE ( 'NONE', #92858, 0.1000000000000002554, 0.003490658503988666988 ) ;
#109580 = CIRCLE ( 'NONE', #67703, 0.06509327318403745899 ) ;
#109581 = DIRECTION ( 'NONE',  ( -0.000000000000000000, 1.000000000000000000, -0.000000000000000000 ) ) ;
#109582 = EDGE_CURVE ( 'NONE', #42734, #3753, #25082, .T. ) ;
#109583 = ADVANCED_FACE ( 'NONE', ( #64985 ), #109749, .T. ) ;
#109584 = EDGE_CURVE ( 'NONE', #46350, #94980, #15235, .T. ) ;
#109585 = EDGE_CURVE ( 'NONE', #77027, #102170, #32412, .T. ) ;
#109586 = ORIENTED_EDGE ( 'NONE', *, *, #42622, .F. ) ;
#109587 = CIRCLE ( 'NONE', #117882, 0.1000000000000002554 ) ;
#109588 = CARTESIAN_POINT ( 'NONE',  ( -0.6500000000000398792, 2.500000000000000000, -6.741600689897078169 ) ) ;
#109589 = CARTESIAN_POINT ( 'NONE',  ( -4.200000000000029488, 2.500000000000000000, -4.330127018922201643 ) ) ;
#109590 = ADVANCED_FACE ( 'NONE', ( #53902 ), #9404, .T. ) ;
#109591 = DIRECTION ( 'NONE',  ( 0.000000000000000000, 0.000000000000000000, -1.000000000000000000 ) ) ;
#109592 = DIRECTION ( 'NONE',  ( -0.000000000000000000, 1.000000000000000000, -0.000000000000000000 ) ) ;
#109593 = DIRECTION ( 'NONE',  ( 0.000000000000000000, 0.000000000000000000, -1.000000000000000000 ) ) ;
#109594 = CARTESIAN_POINT ( 'NONE',  ( 14.14999999999989377, 2.500000000000000000, -1.572243186433550211 ) ) ;
#109595 = FACE_OUTER_BOUND ( 'NONE', #91110, .T. ) ;
#109596 = ORIENTED_EDGE ( 'NONE', *, *, #83554, .F. ) ;
#109597 = EDGE_CURVE ( 'NONE', #8654, #43734, #55363, .T. ) ;
#109598 = CARTESIAN_POINT ( 'NONE',  ( -14.59999999999998366, 2.500000000000000000, -1.084202172485504434E-16 ) ) ;
#109599 = DIRECTION ( 'NONE',  ( 0.000000000000000000, 1.000000000000000000, 0.000000000000000000 ) ) ;
#109600 = DIRECTION ( 'NONE',  ( 0.000000000000000000, 0.000000000000000000, -1.000000000000000000 ) ) ;
#109601 = CONICAL_SURFACE ( 'NONE', #117987, 0.1000000000000002554, 0.003490658503988666988 ) ;
#109602 = AXIS2_PLACEMENT_3D ( 'NONE', #115645, #64621, #126776 ) ;
#109603 = AXIS2_PLACEMENT_3D ( 'NONE', #97415, #77763, #58792 ) ;
#109604 = ORIENTED_EDGE ( 'NONE', *, *, #56730, .F. ) ;
#109605 = DIRECTION ( 'NONE',  ( 0.000000000000000000, 1.000000000000000000, 0.000000000000000000 ) ) ;
#109606 = VECTOR ( 'NONE', #107513, 1000.000000000000000 ) ;
#109607 = VECTOR ( 'NONE', #101977, 1000.000000000000000 ) ;
#109608 = ORIENTED_EDGE ( 'NONE', *, *, #128005, .T. ) ;
#109609 = CONICAL_SURFACE ( 'NONE', #51130, 0.09999999999999999167, 0.003490658503988666988 ) ;
#109610 = ORIENTED_EDGE ( 'NONE', *, *, #105764, .F. ) ;
#109611 = DIRECTION ( 'NONE',  ( -0.000000000000000000, 1.000000000000000000, -0.000000000000000000 ) ) ;
#109612 = ORIENTED_EDGE ( 'NONE', *, *, #17046, .F. ) ;
#109613 = DIRECTION ( 'NONE',  ( 0.000000000000000000, 1.000000000000000000, 0.000000000000000000 ) ) ;
#109614 = CARTESIAN_POINT ( 'NONE',  ( -11.25000000000000000, 2.500000000000000000, 7.188010851410848723 ) ) ;
#109616 = VERTEX_POINT ( 'NONE', #34925 ) ;
#109615 = AXIS2_PLACEMENT_3D ( 'NONE', #117605, #27971, #58089 ) ;
#109617 = AXIS2_PLACEMENT_3D ( 'NONE', #90212, #111138, #43097 ) ;
#109618 = CIRCLE ( 'NONE', #46834, 0.1000000000000002554 ) ;
#109619 = DIRECTION ( 'NONE',  ( -4.274815082592931898E-19, -0.9999939076577903929, -0.003490651415223739937 ) ) ;
#109620 = FACE_OUTER_BOUND ( 'NONE', #2889, .T. ) ;
#109621 = AXIS2_PLACEMENT_3D ( 'NONE', #128249, #66079, #86357 ) ;
#109622 = FACE_OUTER_BOUND ( 'NONE', #72865, .T. ) ;
#109623 = VERTEX_POINT ( 'NONE', #93826 ) ;
#109625 = VERTEX_POINT ( 'NONE', #55193 ) ;
#109624 = EDGE_CURVE ( 'NONE', #118224, #87786, #11445, .T. ) ;
#109626 = ORIENTED_EDGE ( 'NONE', *, *, #37624, .T. ) ;
#109627 = DIRECTION ( 'NONE',  ( 0.000000000000000000, -0.000000000000000000, 1.000000000000000000 ) ) ;
#109628 = CARTESIAN_POINT ( 'NONE',  ( 183.7812500006828031, 0.000000000000000000, 7.700000000000000178 ) ) ;
#109629 = DIRECTION ( 'NONE',  ( -0.000000000000000000, -1.000000000000000000, -0.000000000000000000 ) ) ;
#109630 = FACE_BOUND ( 'NONE', #104780, .T. ) ;
#109631 = EDGE_LOOP ( 'NONE', ( #107153, #6607 ) ) ;
#109632 = DIRECTION ( 'NONE',  ( 0.000000000000000000, 0.000000000000000000, 1.000000000000000000 ) ) ;
#109633 = CARTESIAN_POINT ( 'NONE',  ( 12.29999999999990656, 2.500000000000000000, -4.776537180435977525 ) ) ;
#109634 = VECTOR ( 'NONE', #44044, 1000.000000000000000 ) ;
#109635 = ORIENTED_EDGE ( 'NONE', *, *, #48656, .F. ) ;
#109636 = EDGE_CURVE ( 'NONE', #94218, #59296, #30349, .T. ) ;
#109637 = CARTESIAN_POINT ( 'NONE',  ( -8.750000000000008882, 2.500000000000000000, -2.757883832488654097 ) ) ;
#109638 = DIRECTION ( 'NONE',  ( 0.000000000000000000, 0.000000000000000000, 1.000000000000000000 ) ) ;
#109639 = DIRECTION ( 'NONE',  ( -4.274815082592931898E-19, -0.9999939076577903929, -0.003490651415223739937 ) ) ;
#109640 = DIRECTION ( 'NONE',  ( -0.000000000000000000, 1.000000000000000000, -0.000000000000000000 ) ) ;
#109641 = DIRECTION ( 'NONE',  ( 0.000000000000000000, 0.000000000000000000, 1.000000000000000000 ) ) ;
#109642 = CARTESIAN_POINT ( 'NONE',  ( 8.749999999999957367, 12.50000000000000000, -6.495190528383302464 ) ) ;
#109643 = DIRECTION ( 'NONE',  ( -4.274815082592931898E-19, -0.9999939076577903929, -0.003490651415223739937 ) ) ;
#109644 = AXIS2_PLACEMENT_3D ( 'NONE', #98521, #78281, #67790 ) ;
#109645 = CONICAL_SURFACE ( 'NONE', #69935, 0.09999999999999982514, 0.003490658503988666988 ) ;
#109646 = VERTEX_POINT ( 'NONE', #44077 ) ;
#109647 = VERTEX_POINT ( 'NONE', #13313 ) ;
#109648 = ORIENTED_EDGE ( 'NONE', *, *, #90938, .F. ) ;
#109649 = ORIENTED_EDGE ( 'NONE', *, *, #115871, .F. ) ;
#109650 = ORIENTED_EDGE ( 'NONE', *, *, #84854, .T. ) ;
#109651 = DIRECTION ( 'NONE',  ( 0.000000000000000000, 1.000000000000000000, 0.000000000000000000 ) ) ;
#109652 = DIRECTION ( 'NONE',  ( -0.000000000000000000, -1.000000000000000000, -0.000000000000000000 ) ) ;
#109653 = ORIENTED_EDGE ( 'NONE', *, *, #39200, .T. ) ;
#109654 = FACE_BOUND ( 'NONE', #93684, .T. ) ;
#109655 = DIRECTION ( 'NONE',  ( 0.000000000000000000, -0.9999939076577903929, 0.003490651415223739937 ) ) ;
#109656 = CIRCLE ( 'NONE', #103307, 0.1000000000000002554 ) ;
#109657 = FACE_OUTER_BOUND ( 'NONE', #37725, .T. ) ;
#109658 = CONICAL_SURFACE ( 'NONE', #28181, 0.1000000000000002554, 0.003490658503988666988 ) ;
#109659 = CARTESIAN_POINT ( 'NONE',  ( -2.900000000000029221, 2.500000000000000000, -0.6928203230275541413 ) ) ;
#109660 = CARTESIAN_POINT ( 'NONE',  ( 184.4999999999999716, -0.6202644670797828885, 7.670962774272589435 ) ) ;
#109661 = DIRECTION ( 'NONE',  ( 0.000000000000000000, 0.000000000000000000, -1.000000000000000000 ) ) ;
#109662 = DIRECTION ( 'NONE',  ( -0.000000000000000000, -1.000000000000000000, -0.000000000000000000 ) ) ;
#109663 = ORIENTED_EDGE ( 'NONE', *, *, #89463, .T. ) ;
#109664 = ORIENTED_EDGE ( 'NONE', *, *, #20445, .T. ) ;
#109665 = ADVANCED_FACE ( 'NONE', ( #123285 ), #30255, .T. ) ;
#109666 = CONICAL_SURFACE ( 'NONE', #55378, 0.09999999999999982514, 0.003490658503988666988 ) ;
#109667 = VERTEX_POINT ( 'NONE', #24441 ) ;
#109668 = EDGE_LOOP ( 'NONE', ( #89607, #85863, #3799, #115478 ) ) ;
#109669 = CIRCLE ( 'NONE', #13500, 0.1000000000000002554 ) ;
#109670 = ORIENTED_EDGE ( 'NONE', *, *, #39439, .F. ) ;
#109671 = ORIENTED_EDGE ( 'NONE', *, *, #99074, .T. ) ;
#109672 = CARTESIAN_POINT ( 'NONE',  ( 15.40585131959762499, 2.499999999999999112, 5.817868759122426958 ) ) ;
#109674 = AXIS2_PLACEMENT_3D ( 'NONE', #83882, #16408, #76000 ) ;
#109673 = LINE ( 'NONE', #119471, #80236 ) ;
#109675 = EDGE_LOOP ( 'NONE', ( #95184, #87236, #102717, #112940 ) ) ;
#109676 = DIRECTION ( 'NONE',  ( 0.000000000000000000, -0.9999939076577903929, 0.003490651415223739937 ) ) ;
#109677 = CIRCLE ( 'NONE', #78296, 0.06509327318403745899 ) ;
#109678 = EDGE_CURVE ( 'NONE', #99929, #24133, #21929, .T. ) ;
#109679 = FACE_OUTER_BOUND ( 'NONE', #34475, .T. ) ;
#109680 = CARTESIAN_POINT ( 'NONE',  ( 3.549999999999943867, 12.50000000000000000, -6.148780366869526226 ) ) ;
#109681 = CARTESIAN_POINT ( 'NONE',  ( 186.2343750003414016, 8.734944146203032389, 5.348610694689227483E-16 ) ) ;
#109682 = DIRECTION ( 'NONE',  ( -1.000000000000000000, 0.000000000000000000, 0.000000000000000000 ) ) ;
#109683 = CARTESIAN_POINT ( 'NONE',  ( 2.949999999999946887, 12.50000000000000000, -2.230156782645139391 ) ) ;
#109684 = EDGE_CURVE ( 'NONE', #95907, #6696, #90868, .T. ) ;
#109685 = DIRECTION ( 'NONE',  ( 0.000000000000000000, 0.000000000000000000, -1.000000000000000000 ) ) ;
#109686 = EDGE_CURVE ( 'NONE', #36888, #117215, #15632, .T. ) ;
#109687 = VERTEX_POINT ( 'NONE', #95118 ) ;
#109688 = LINE ( 'NONE', #27241, #27464 ) ;
#109689 = VERTEX_POINT ( 'NONE', #94452 ) ;
#109690 = VERTEX_POINT ( 'NONE', #83369 ) ;
#109691 = CARTESIAN_POINT ( 'NONE',  ( 14.34999999999989306, 2.500000000000000000, -1.918653347947326004 ) ) ;
#109692 = ADVANCED_FACE ( 'NONE', ( #73523 ), #72099, .T. ) ;
#109693 = CIRCLE ( 'NONE', #28211, 0.06509327318403741736 ) ;
#109694 = CIRCLE ( 'NONE', #62900, 0.06509327318403745899 ) ;
#109695 = CARTESIAN_POINT ( 'NONE',  ( 2.049999999999950084, 12.50000000000000000, -2.230156782645139391 ) ) ;
#109696 = AXIS2_PLACEMENT_3D ( 'NONE', #51893, #33546, #62985 ) ;
#109697 = DIRECTION ( 'NONE',  ( 0.000000000000000000, 0.000000000000000000, 1.000000000000000000 ) ) ;
#109698 = EDGE_CURVE ( 'NONE', #15257, #9179, #74150, .T. ) ;
#109699 = ORIENTED_EDGE ( 'NONE', *, *, #107527, .F. ) ;
#109700 = VERTEX_POINT ( 'NONE', #56462 ) ;
#109701 = DIRECTION ( 'NONE',  ( -4.274815082592931898E-19, -0.9999939076577903929, -0.003490651415223739937 ) ) ;
#109702 = CIRCLE ( 'NONE', #126423, 0.06509327318403741736 ) ;
#109703 = CIRCLE ( 'NONE', #26078, 0.06509327318403743123 ) ;
#109704 = CARTESIAN_POINT ( 'NONE',  ( -12.29999999999999538, 12.50000000000000000, 4.741630453620009789 ) ) ;
#109705 = CARTESIAN_POINT ( 'NONE',  ( -7.500000000000016875, 12.50000000000000000, 0.6928203230275494784 ) ) ;
#109706 = DIRECTION ( 'NONE',  ( 0.000000000000000000, -0.000000000000000000, 1.000000000000000000 ) ) ;
#109707 = ORIENTED_EDGE ( 'NONE', *, *, #50320, .F. ) ;
#109708 = AXIS2_PLACEMENT_3D ( 'NONE', #94123, #82390, #35224 ) ;
#109709 = DIRECTION ( 'NONE',  ( 0.000000000000000000, -0.000000000000000000, 1.000000000000000000 ) ) ;
#109710 = ORIENTED_EDGE ( 'NONE', *, *, #9967, .T. ) ;
#109711 = CARTESIAN_POINT ( 'NONE',  ( -5.450000000000019718, 12.50000000000000000, 2.099970236277060032 ) ) ;
#109712 = CIRCLE ( 'NONE', #97178, 0.1000000000000000472 ) ;
#109713 = AXIS2_PLACEMENT_3D ( 'NONE', #1931, #72627, #101437 ) ;
#109714 = VERTEX_POINT ( 'NONE', #96382 ) ;
#109715 = CARTESIAN_POINT ( 'NONE',  ( -13.74999999999998934, 2.500000000000000000, -1.572243186433547990 ) ) ;
#109716 = DIRECTION ( 'NONE',  ( 0.000000000000000000, 0.000000000000000000, 1.000000000000000000 ) ) ;
#109717 = DIRECTION ( 'NONE',  ( -0.000000000000000000, -1.000000000000000000, -0.000000000000000000 ) ) ;
#109718 = AXIS2_PLACEMENT_3D ( 'NONE', #122933, #73812, #54191 ) ;
#109719 = CARTESIAN_POINT ( 'NONE',  ( -10.20000000000000284, 2.500000000000000000, -0.3464101615137782364 ) ) ;
#109720 = VERTEX_POINT ( 'NONE', #106226 ) ;
#109721 = CARTESIAN_POINT ( 'NONE',  ( -13.34999999999999076, 2.500000000000000000, -2.165063509461099489 ) ) ;
#109722 = VERTEX_POINT ( 'NONE', #126510 ) ;
#109723 = EDGE_LOOP ( 'NONE', ( #83859, #84628 ) ) ;
#109724 = DIRECTION ( 'NONE',  ( -4.274815082592931898E-19, -0.9999939076577903929, -0.003490651415223739937 ) ) ;
#109725 = CARTESIAN_POINT ( 'NONE',  ( 97.50000000000000000, -1.500000000000000222, -1.322875655532295136 ) ) ;
#109726 = DIRECTION ( 'NONE',  ( 0.000000000000000000, -0.000000000000000000, 1.000000000000000000 ) ) ;
#109727 = CYLINDRICAL_SURFACE ( 'NONE', #39681, 7.700000000000000178 ) ;
#109728 = DIRECTION ( 'NONE',  ( -0.000000000000000000, -1.000000000000000000, -0.000000000000000000 ) ) ;
#109729 = FACE_OUTER_BOUND ( 'NONE', #12339, .T. ) ;
#109730 = CARTESIAN_POINT ( 'NONE',  ( 5.849999999999935696, 2.500000000000000000, -6.395190528383301931 ) ) ;
#109731 = DIRECTION ( 'NONE',  ( -0.000000000000000000, -1.000000000000000000, -0.000000000000000000 ) ) ;
#109732 = DIRECTION ( 'NONE',  ( 0.000000000000000000, -0.000000000000000000, 1.000000000000000000 ) ) ;
#109733 = EDGE_CURVE ( 'NONE', #46924, #129420, #107509, .T. ) ;
#109734 = EDGE_CURVE ( 'NONE', #70361, #94856, #42876, .T. ) ;
#109735 = EDGE_CURVE ( 'NONE', #19417, #52442, #13582, .T. ) ;
#109736 = CONICAL_SURFACE ( 'NONE', #70028, 0.09999999999999982514, 0.003490658503988666988 ) ;
#109737 = EDGE_CURVE ( 'NONE', #63445, #22700, #76117, .T. ) ;
#109738 = CONICAL_SURFACE ( 'NONE', #40805, 0.1000000000000000472, 0.003490658503988666988 ) ;
#109739 = EDGE_LOOP ( 'NONE', ( #111345, #88578 ) ) ;
#109740 = EDGE_CURVE ( 'NONE', #65438, #82940, #120120, .T. ) ;
#109741 = LINE ( 'NONE', #10856, #57045 ) ;
#109742 = CARTESIAN_POINT ( 'NONE',  ( -1.700000000000034817, 2.500000000000000000, -4.330127018922201643 ) ) ;
#109743 = FACE_OUTER_BOUND ( 'NONE', #126045, .T. ) ;
#109744 = CARTESIAN_POINT ( 'NONE',  ( -12.69999999999999218, 2.500000000000000000, -4.676537180435975216 ) ) ;
#109745 = DIRECTION ( 'NONE',  ( -0.000000000000000000, 1.000000000000000000, -0.000000000000000000 ) ) ;
#109746 = ORIENTED_EDGE ( 'NONE', *, *, #118116, .T. ) ;
#109747 = ADVANCED_FACE ( 'NONE', ( #117289 ), #34448, .T. ) ;
#109748 = FACE_OUTER_BOUND ( 'NONE', #72334, .T. ) ;
#109749 = CONICAL_SURFACE ( 'NONE', #46968, 0.1000000000000002554, 0.003490658503988666988 ) ;
#109750 = ADVANCED_FACE ( 'NONE', ( #57774 ), #63692, .T. ) ;
#109751 = AXIS2_PLACEMENT_3D ( 'NONE', #75196, #73903, #105302 ) ;
#109752 = DIRECTION ( 'NONE',  ( 0.000000000000000000, -0.000000000000000000, 1.000000000000000000 ) ) ;
#109754 = ORIENTED_EDGE ( 'NONE', *, *, #87969, .T. ) ;
#109753 = LINE ( 'NONE', #20084, #98529 ) ;
#109755 = ORIENTED_EDGE ( 'NONE', *, *, #43878, .T. ) ;
#109756 = CARTESIAN_POINT ( 'NONE',  ( 3.299999999999944755, 2.500000000000000000, -4.430127018922202176 ) ) ;
#109757 = AXIS2_PLACEMENT_3D ( 'NONE', #296, #120103, #114141 ) ;
#109758 = CONICAL_SURFACE ( 'NONE', #38675, 0.1000000000000002554, 0.003490658503988666988 ) ;
#109759 = ORIENTED_EDGE ( 'NONE', *, *, #118271, .T. ) ;
#109760 = ORIENTED_EDGE ( 'NONE', *, *, #88062, .T. ) ;
#109761 = VERTEX_POINT ( 'NONE', #47955 ) ;
#109762 = CARTESIAN_POINT ( 'NONE',  ( -6.650000000000015454, 2.500000000000000000, 2.857883832488649301 ) ) ;
#109763 = CARTESIAN_POINT ( 'NONE',  ( -0.6500000000000403233, 12.50000000000000000, 6.083687093685482772 ) ) ;
#109764 = FACE_OUTER_BOUND ( 'NONE', #39264, .T. ) ;
#109765 = CARTESIAN_POINT ( 'NONE',  ( 2.949999999999946887, 12.50000000000000000, -2.165063509461101710 ) ) ;
#109766 = EDGE_LOOP ( 'NONE', ( #96506, #15441, #58131, #31276 ) ) ;
#109767 = CARTESIAN_POINT ( 'NONE',  ( -3.550000000000030909, 12.50000000000000000, -6.841600689897078702 ) ) ;
#109768 = ORIENTED_EDGE ( 'NONE', *, *, #26978, .T. ) ;
#109769 = DIRECTION ( 'NONE',  ( 0.000000000000000000, 0.000000000000000000, 1.000000000000000000 ) ) ;
#109770 = CARTESIAN_POINT ( 'NONE',  ( 2.899999999999946620, 2.500000000000000000, -5.022947341949754119 ) ) ;
#109771 = CARTESIAN_POINT ( 'NONE',  ( 9.399999999999918643, 2.500000000000000000, -0.3464101615137782364 ) ) ;
#109772 = CIRCLE ( 'NONE', #126499, 0.06509327318403745899 ) ;
#109773 = ORIENTED_EDGE ( 'NONE', *, *, #116802, .F. ) ;
#109774 = ORIENTED_EDGE ( 'NONE', *, *, #20431, .F. ) ;
#109775 = ORIENTED_EDGE ( 'NONE', *, *, #87826, .F. ) ;
#109776 = AXIS2_PLACEMENT_3D ( 'NONE', #97808, #8133, #29095 ) ;
#109777 = VERTEX_POINT ( 'NONE', #75462 ) ;
#109778 = ORIENTED_EDGE ( 'NONE', *, *, #53050, .F. ) ;
#109779 = DIRECTION ( 'NONE',  ( 0.000000000000000000, 0.000000000000000000, 1.000000000000000000 ) ) ;
#109780 = DIRECTION ( 'NONE',  ( 0.000000000000000000, 0.000000000000000000, 1.000000000000000000 ) ) ;
#109781 = AXIS2_PLACEMENT_3D ( 'NONE', #24994, #16437, #17066 ) ;
#109782 = CARTESIAN_POINT ( 'NONE',  ( 11.44999999999990870, 2.500000000000000000, -1.718653347947326049 ) ) ;
#109783 = FACE_BOUND ( 'NONE', #7772, .T. ) ;
#109784 = DIRECTION ( 'NONE',  ( 0.000000000000000000, 1.000000000000000000, 0.000000000000000000 ) ) ;
#109785 = CARTESIAN_POINT ( 'NONE',  ( 186.8645833340161175, -6.668395609140180369, 3.849999999999994760 ) ) ;
#109786 = DIRECTION ( 'NONE',  ( 0.000000000000000000, 0.000000000000000000, 1.000000000000000000 ) ) ;
#109787 = CARTESIAN_POINT ( 'NONE',  ( 4.599999999999940137, 2.500000000000000000, -5.122947341949753763 ) ) ;
#109788 = AXIS2_PLACEMENT_3D ( 'NONE', #87467, #124838, #24703 ) ;
#109789 = ADVANCED_FACE ( 'NONE', ( #68219 ), #84614, .T. ) ;
#109790 = AXIS2_PLACEMENT_3D ( 'NONE', #2433, #1162, #21445 ) ;
#109791 = CIRCLE ( 'NONE', #40862, 0.06509327318403745899 ) ;
#109792 = FACE_OUTER_BOUND ( 'NONE', #72508, .T. ) ;
#109793 = CIRCLE ( 'NONE', #128602, 0.09999999999999982514 ) ;
#109794 = CARTESIAN_POINT ( 'NONE',  ( -9.350000000000008527, 2.500000000000000000, -6.741600689897071952 ) ) ;
#109795 = CARTESIAN_POINT ( 'NONE',  ( -1.900000000000034994, 2.500000000000000000, -4.676537180435978769 ) ) ;
#109796 = CIRCLE ( 'NONE', #63830, 0.1000000000000002554 ) ;
#109797 = AXIS2_PLACEMENT_3D ( 'NONE', #2255, #93881, #103042 ) ;
#109798 = DIRECTION ( 'NONE',  ( 0.000000000000000000, -0.9999939076577903929, 0.003490651415223739937 ) ) ;
#109799 = ORIENTED_EDGE ( 'NONE', *, *, #74964, .F. ) ;
#109800 = ORIENTED_EDGE ( 'NONE', *, *, #127186, .T. ) ;
#109801 = ORIENTED_EDGE ( 'NONE', *, *, #64217, .T. ) ;
#109802 = EDGE_LOOP ( 'NONE', ( #78957, #109912 ) ) ;
#109803 = CIRCLE ( 'NONE', #116052, 0.06509327318403745899 ) ;
#109804 = DIRECTION ( 'NONE',  ( -0.000000000000000000, 1.000000000000000000, -0.000000000000000000 ) ) ;
#109805 = LINE ( 'NONE', #98042, #31949 ) ;
#109806 = FACE_BOUND ( 'NONE', #129406, .T. ) ;
#109807 = LINE ( 'NONE', #99992, #112628 ) ;
#109808 = ORIENTED_EDGE ( 'NONE', *, *, #103812, .T. ) ;
#109809 = LINE ( 'NONE', #20143, #122037 ) ;
#109810 = DIRECTION ( 'NONE',  ( -0.000000000000000000, 1.000000000000000000, -0.000000000000000000 ) ) ;
#109811 = CARTESIAN_POINT ( 'NONE',  ( 7.299999999999927880, 2.500000000000000000, -4.676537180435977881 ) ) ;
#109812 = CARTESIAN_POINT ( 'NONE',  ( -5.000000000000024869, 2.500000000000000000, -5.022947341949754119 ) ) ;
#109814 = EDGE_LOOP ( 'NONE', ( #114026, #41549 ) ) ;
#109813 = VECTOR ( 'NONE', #56354, 1000.000000000000000 ) ;
#109815 = DIRECTION ( 'NONE',  ( -0.000000000000000000, 1.000000000000000000, -0.000000000000000000 ) ) ;
#109816 = VERTEX_POINT ( 'NONE', #35560 ) ;
#109817 = ORIENTED_EDGE ( 'NONE', *, *, #11414, .F. ) ;
#109818 = CARTESIAN_POINT ( 'NONE',  ( 6.249999999999930722, 2.500000000000000000, 7.188010851410848723 ) ) ;
#109819 = DIRECTION ( 'NONE',  ( 0.000000000000000000, 1.000000000000000000, 0.000000000000000000 ) ) ;
#109820 = CIRCLE ( 'NONE', #51351, 0.09999999999999982514 ) ;
#109821 = ORIENTED_EDGE ( 'NONE', *, *, #2888, .F. ) ;
#109822 = AXIS2_PLACEMENT_3D ( 'NONE', #74221, #21912, #23840 ) ;
#109823 = VECTOR ( 'NONE', #115564, 1000.000000000000000 ) ;
#109824 = ADVANCED_FACE ( 'NONE', ( #127789 ), #113859, .T. ) ;
#109825 = CARTESIAN_POINT ( 'NONE',  ( -8.950000000000009948, 2.500000000000000000, 2.511473670974873507 ) ) ;
#109826 = DIRECTION ( 'NONE',  ( 0.000000000000000000, 0.000000000000000000, 1.000000000000000000 ) ) ;
#109827 = VERTEX_POINT ( 'NONE', #6690 ) ;
#109828 = FACE_OUTER_BOUND ( 'NONE', #116721, .T. ) ;
#109829 = VERTEX_POINT ( 'NONE', #46660 ) ;
#109830 = EDGE_CURVE ( 'NONE', #112785, #41715, #128556, .T. ) ;
#109831 = DIRECTION ( 'NONE',  ( 0.000000000000000000, 0.000000000000000000, 1.000000000000000000 ) ) ;
#109832 = EDGE_CURVE ( 'NONE', #60441, #10391, #49121, .T. ) ;
#109833 = EDGE_LOOP ( 'NONE', ( #16870, #6602 ) ) ;
#109834 = CARTESIAN_POINT ( 'NONE',  ( 1.449999999999949551, 2.500000000000000000, 6.741600689897071952 ) ) ;
#109835 = CIRCLE ( 'NONE', #122367, 0.06509327318403745899 ) ;
#109836 = ORIENTED_EDGE ( 'NONE', *, *, #19615, .F. ) ;
#109838 = CARTESIAN_POINT ( 'NONE',  ( 12.89999999999990266, 12.50000000000000000, 5.088040615133786027 ) ) ;
#109837 = VECTOR ( 'NONE', #80365, 1000.000000000000000 ) ;
#109839 = EDGE_LOOP ( 'NONE', ( #51025, #13879, #102901, #24823 ) ) ;
#109840 = CARTESIAN_POINT ( 'NONE',  ( 1.249999999999988898, 2.500000000000000000, -6.495190528383302464 ) ) ;
#109841 = CARTESIAN_POINT ( 'NONE',  ( 1.899999999999949507, 12.50000000000000000, 3.983716857408420964 ) ) ;
#109842 = EDGE_CURVE ( 'NONE', #12245, #18723, #116677, .T. ) ;
#109843 = EDGE_CURVE ( 'NONE', #119953, #62336, #99286, .T. ) ;
#109844 = DIRECTION ( 'NONE',  ( -0.000000000000000000, -1.000000000000000000, -0.000000000000000000 ) ) ;
#109845 = ADVANCED_FACE ( 'NONE', ( #76766 ), #57113, .T. ) ;
#109846 = LINE ( 'NONE', #117699, #88381 ) ;
#109847 = ADVANCED_FACE ( 'NONE', ( #87213 ), #28177, .T. ) ;
#109848 = ADVANCED_FACE ( 'NONE', ( #79977 ), #20421, .T. ) ;
#109849 = FACE_OUTER_BOUND ( 'NONE', #5577, .T. ) ;
#109850 = VERTEX_POINT ( 'NONE', #40061 ) ;
#109851 = ORIENTED_EDGE ( 'NONE', *, *, #63489, .T. ) ;
#109852 = EDGE_LOOP ( 'NONE', ( #86691, #10411, #65967, #68336 ) ) ;
#109853 = DIRECTION ( 'NONE',  ( -0.000000000000000000, -1.000000000000000000, -0.000000000000000000 ) ) ;
#109854 = AXIS2_PLACEMENT_3D ( 'NONE', #127198, #37527, #105617 ) ;
#109855 = CONICAL_SURFACE ( 'NONE', #40921, 0.09999999999999982514, 0.003490658503988666988 ) ;
#109856 = DIRECTION ( 'NONE',  ( -0.000000000000000000, 1.000000000000000000, -0.000000000000000000 ) ) ;
#109857 = DIRECTION ( 'NONE',  ( 0.000000000000000000, 1.000000000000000000, 0.000000000000000000 ) ) ;
#109859 = VERTEX_POINT ( 'NONE', #29588 ) ;
#109858 = ORIENTED_EDGE ( 'NONE', *, *, #72783, .T. ) ;
#109860 = ORIENTED_EDGE ( 'NONE', *, *, #72761, .T. ) ;
#109861 = EDGE_CURVE ( 'NONE', #87809, #44827, #90421, .T. ) ;
#109862 = CARTESIAN_POINT ( 'NONE',  ( -0.6500000000000398792, 12.50000000000000000, -2.511473670974877948 ) ) ;
#109863 = ORIENTED_EDGE ( 'NONE', *, *, #83385, .T. ) ;
#109864 = FACE_OUTER_BOUND ( 'NONE', #79600, .T. ) ;
#109865 = DIRECTION ( 'NONE',  ( 0.000000000000000000, -0.000000000000000000, 1.000000000000000000 ) ) ;
#109866 = CARTESIAN_POINT ( 'NONE',  ( 165.4999999999999716, 0.000000000000000000, 2.000000000000000000 ) ) ;
#109867 = CIRCLE ( 'NONE', #19978, 0.1000000000000000472 ) ;
#109868 = FACE_OUTER_BOUND ( 'NONE', #50624, .T. ) ;
#109869 = DIRECTION ( 'NONE',  ( 0.000000000000000000, 0.000000000000000000, -1.000000000000000000 ) ) ;
#109870 = FACE_OUTER_BOUND ( 'NONE', #60169, .T. ) ;
#109871 = AXIS2_PLACEMENT_3D ( 'NONE', #67991, #118384, #37268 ) ;
#109872 = CARTESIAN_POINT ( 'NONE',  ( 3.749999999999942268, 2.500000000000000000, -5.802370205355749988 ) ) ;
#109873 = ORIENTED_EDGE ( 'NONE', *, *, #18703, .F. ) ;
#109874 = VERTEX_POINT ( 'NONE', #119906 ) ;
#109875 = DIRECTION ( 'NONE',  ( -0.000000000000000000, 1.000000000000000000, -0.000000000000000000 ) ) ;
#109876 = VECTOR ( 'NONE', #63127, 1000.000000000000000 ) ;
#109877 = AXIS2_PLACEMENT_3D ( 'NONE', #23118, #63047, #13283 ) ;
#109878 = VERTEX_POINT ( 'NONE', #78710 ) ;
#109879 = VERTEX_POINT ( 'NONE', #120551 ) ;
#109880 = CARTESIAN_POINT ( 'NONE',  ( 185.8177083336747444, 4.367472073101515306, 7.564683531250000925 ) ) ;
#109881 = CARTESIAN_POINT ( 'NONE',  ( -3.100000000000028511, 2.500000000000000000, -3.983716857408426293 ) ) ;
#109882 = CARTESIAN_POINT ( 'NONE',  ( -15.19999999999998153, 12.50000000000000000, -0.3464101615137759604 ) ) ;
#109883 = CONICAL_SURFACE ( 'NONE', #103526, 0.1000000000000002554, 0.003490658503988666988 ) ;
#109884 = CARTESIAN_POINT ( 'NONE',  ( 195.5000000000000000, 0.000000000000000000, 0.000000000000000000 ) ) ;
#109885 = DIRECTION ( 'NONE',  ( 0.000000000000000000, 1.000000000000000000, 0.000000000000000000 ) ) ;
#109886 = FACE_OUTER_BOUND ( 'NONE', #33057, .T. ) ;
#109887 = FACE_OUTER_BOUND ( 'NONE', #26595, .T. ) ;
#109888 = EDGE_CURVE ( 'NONE', #20699, #29164, #118053, .T. ) ;
#109889 = CONICAL_SURFACE ( 'NONE', #80554, 0.1000000000000002554, 0.003490658503988666988 ) ;
#109890 = EDGE_CURVE ( 'NONE', #80232, #15598, #5171, .T. ) ;
#109891 = EDGE_CURVE ( 'NONE', #27804, #104330, #88907, .T. ) ;
#109892 = DIRECTION ( 'NONE',  ( 0.000000000000000000, 0.000000000000000000, 1.000000000000000000 ) ) ;
#109893 = AXIS2_PLACEMENT_3D ( 'NONE', #106343, #16652, #96499 ) ;
#109894 = VECTOR ( 'NONE', #23053, 1000.000000000000000 ) ;
#109895 = EDGE_LOOP ( 'NONE', ( #95124, #118730, #24604, #36825 ) ) ;
#109896 = EDGE_CURVE ( 'NONE', #2388, #60152, #107685, .T. ) ;
#109897 = AXIS2_PLACEMENT_3D ( 'NONE', #36294, #128550, #116752 ) ;
#109898 = ORIENTED_EDGE ( 'NONE', *, *, #62571, .F. ) ;
#109899 = ORIENTED_EDGE ( 'NONE', *, *, #54537, .T. ) ;
#109900 = EDGE_CURVE ( 'NONE', #115572, #74354, #103588, .T. ) ;
#109901 = ORIENTED_EDGE ( 'NONE', *, *, #15334, .T. ) ;
#109902 = DIRECTION ( 'NONE',  ( 0.000000000000000000, 0.000000000000000000, 1.000000000000000000 ) ) ;
#109903 = DIRECTION ( 'NONE',  ( 0.000000000000000000, 1.000000000000000000, 0.000000000000000000 ) ) ;
#109904 = EDGE_CURVE ( 'NONE', #115877, #29350, #71430, .T. ) ;
#109905 = ORIENTED_EDGE ( 'NONE', *, *, #66068, .F. ) ;
#109906 = EDGE_CURVE ( 'NONE', #123035, #17965, #110086, .T. ) ;
#109907 = DIRECTION ( 'NONE',  ( 0.000000000000000000, 0.000000000000000000, 1.000000000000000000 ) ) ;
#109908 = CARTESIAN_POINT ( 'NONE',  ( -5.850000000000018296, 12.50000000000000000, 1.407149913249508000 ) ) ;
#109909 = ADVANCED_FACE ( 'NONE', ( #60979 ), #100892, .T. ) ;
#109910 = PLANE ( 'NONE',  #9345 ) ;
#109912 = ORIENTED_EDGE ( 'NONE', *, *, #92723, .F. ) ;
#109911 = CARTESIAN_POINT ( 'NONE',  ( -11.24999999999996270, 2.500000000000000000, 6.395190528383296602 ) ) ;
#109913 = LINE ( 'NONE', #91553, #13976 ) ;
#109914 = VECTOR ( 'NONE', #8529, 1000.000000000000000 ) ;
#109915 = EDGE_CURVE ( 'NONE', #12077, #1020, #128641, .T. ) ;
#109916 = DIRECTION ( 'NONE',  ( -0.000000000000000000, -1.000000000000000000, -0.000000000000000000 ) ) ;
#109917 = ORIENTED_EDGE ( 'NONE', *, *, #128230, .T. ) ;
#109918 = ORIENTED_EDGE ( 'NONE', *, *, #115388, .F. ) ;
#109919 = VERTEX_POINT ( 'NONE', #50510 ) ;
#109920 = VERTEX_POINT ( 'NONE', #9305 ) ;
#109921 = CARTESIAN_POINT ( 'NONE',  ( -3.750000000000029310, 12.50000000000000000, -7.188010851410854052 ) ) ;
#109922 = AXIS2_PLACEMENT_3D ( 'NONE', #77297, #117187, #27534 ) ;
#109923 = AXIS2_PLACEMENT_3D ( 'NONE', #10605, #17864, #39478 ) ;
#109924 = DIRECTION ( 'NONE',  ( -0.000000000000000000, -1.000000000000000000, -0.000000000000000000 ) ) ;
#109925 = CARTESIAN_POINT ( 'NONE',  ( 3.749999999999944045, 12.50000000000000000, -2.922977105672691422 ) ) ;
#109926 = CIRCLE ( 'NONE', #61907, 0.1000000000000002554 ) ;
#109927 = AXIS2_PLACEMENT_3D ( 'NONE', #90291, #20286, #121061 ) ;
#109928 = DIRECTION ( 'NONE',  ( 0.000000000000000000, 0.000000000000000000, 1.000000000000000000 ) ) ;
#109929 = ORIENTED_EDGE ( 'NONE', *, *, #57575, .F. ) ;
#109930 = CARTESIAN_POINT ( 'NONE',  ( 0.6499999999999543920, 12.50000000000000000, 6.841600689897072485 ) ) ;
#109931 = PLANE ( 'NONE',  #41352 ) ;
#109932 = CARTESIAN_POINT ( 'NONE',  ( 105.0000000000000142, 9.000000000000001776, 0.2500000000000003886 ) ) ;
#109933 = DIRECTION ( 'NONE',  ( 0.000000000000000000, 0.000000000000000000, 1.000000000000000000 ) ) ;
#109934 = ADVANCED_FACE ( 'NONE', ( #31530 ), #124413, .T. ) ;
#109935 = AXIS2_PLACEMENT_3D ( 'NONE', #87058, #115881, #66132 ) ;
#109936 = VERTEX_POINT ( 'NONE', #109442 ) ;
#109937 = CARTESIAN_POINT ( 'NONE',  ( 9.599999999999914380, 12.50000000000000000, 4.395220292106234439 ) ) ;
#109939 = CONICAL_SURFACE ( 'NONE', #40999, 0.09999999999999999167, 0.003490658503988666988 ) ;
#109938 = CIRCLE ( 'NONE', #86932, 0.1000000000000000056 ) ;
#109940 = VERTEX_POINT ( 'NONE', #767 ) ;
#109941 = VERTEX_POINT ( 'NONE', #41368 ) ;
#109942 = DIRECTION ( 'NONE',  ( 0.000000000000000000, -0.9999939076577903929, 0.003490651415223739937 ) ) ;
#109943 = DIRECTION ( 'NONE',  ( 0.000000000000000000, 1.000000000000000000, 0.000000000000000000 ) ) ;
#109944 = FACE_BOUND ( 'NONE', #107050, .T. ) ;
#109945 = CARTESIAN_POINT ( 'NONE',  ( 9.349999999999919709, 2.500000000000000000, 2.611473670974873151 ) ) ;
#109946 = CARTESIAN_POINT ( 'NONE',  ( -10.65000000000000213, 12.50000000000000000, 6.148780366869520009 ) ) ;
#109947 = DIRECTION ( 'NONE',  ( 0.000000000000000000, 1.000000000000000000, 0.000000000000000000 ) ) ;
#109948 = AXIS2_PLACEMENT_3D ( 'NONE', #58938, #128341, #20301 ) ;
#109949 = AXIS2_PLACEMENT_3D ( 'NONE', #34830, #74732, #24984 ) ;
#109950 = EDGE_CURVE ( 'NONE', #4680, #1374, #11535, .T. ) ;
#109951 = DIRECTION ( 'NONE',  ( 0.000000000000000000, 0.000000000000000000, -1.000000000000000000 ) ) ;
#109952 = CARTESIAN_POINT ( 'NONE',  ( -9.150000000000009237, 2.500000000000000000, -1.472243186433550122 ) ) ;
#109953 = DIRECTION ( 'NONE',  ( 0.000000000000000000, 0.000000000000000000, 1.000000000000000000 ) ) ;
#109954 = DIRECTION ( 'NONE',  ( 0.000000000000000000, 0.000000000000000000, -1.000000000000000000 ) ) ;
#109955 = ORIENTED_EDGE ( 'NONE', *, *, #81856, .T. ) ;
#109956 = CARTESIAN_POINT ( 'NONE',  ( -13.74999999999995381, 2.500000000000000000, -2.165063509461099489 ) ) ;
#109957 = LINE ( 'NONE', #80505, #72520 ) ;
#109958 = ORIENTED_EDGE ( 'NONE', *, *, #65950, .T. ) ;
#109959 = ORIENTED_EDGE ( 'NONE', *, *, #29162, .T. ) ;
#109960 = DIRECTION ( 'NONE',  ( 0.000000000000000000, 0.000000000000000000, -1.000000000000000000 ) ) ;
#109961 = EDGE_CURVE ( 'NONE', #111598, #25747, #81277, .T. ) ;
#109962 = CARTESIAN_POINT ( 'NONE',  ( 9.999999999999911182, 2.500000000000000000, 5.022947341949748790 ) ) ;
#109963 = FACE_BOUND ( 'NONE', #128543, .T. ) ;
#109964 = DIRECTION ( 'NONE',  ( 0.000000000000000000, -0.9999939076577903929, 0.003490651415223739937 ) ) ;
#109965 = AXIS2_PLACEMENT_3D ( 'NONE', #5341, #55737, #35468 ) ;
#109966 = CARTESIAN_POINT ( 'NONE',  ( 2.899999999999944844, 12.50000000000000000, 5.022947341949748790 ) ) ;
#109967 = VECTOR ( 'NONE', #5877, 1000.000000000000000 ) ;
#109968 = VERTEX_POINT ( 'NONE', #111350 ) ;
#109969 = CARTESIAN_POINT ( 'NONE',  ( -3.550000000000027800, 2.500000000000000000, 6.148780366869520009 ) ) ;
#109970 = CARTESIAN_POINT ( 'NONE',  ( 185.0000000000000000, 0.000000000000000000, 7.700000000000000178 ) ) ;
#109971 = ORIENTED_EDGE ( 'NONE', *, *, #107143, .F. ) ;
#109972 = FACE_OUTER_BOUND ( 'NONE', #48840, .T. ) ;
#109973 = CYLINDRICAL_SURFACE ( 'NONE', #11448, 7.700000000000000178 ) ;
#109974 = AXIS2_PLACEMENT_3D ( 'NONE', #68568, #100601, #69873 ) ;
#109975 = CARTESIAN_POINT ( 'NONE',  ( 9.799999999999913669, 2.500000000000000000, -4.083716857408426826 ) ) ;
#109976 = CARTESIAN_POINT ( 'NONE',  ( 6.049999999999935874, 2.500000000000000000, -6.941600689897077459 ) ) ;
#109977 = AXIS2_PLACEMENT_3D ( 'NONE', #63045, #102958, #93161 ) ;
#109978 = ORIENTED_EDGE ( 'NONE', *, *, #129344, .F. ) ;
#109980 = EDGE_CURVE ( 'NONE', #35273, #25034, #36688, .T. ) ;
#109979 = VECTOR ( 'NONE', #41289, 1000.000000000000000 ) ;
#109981 = CARTESIAN_POINT ( 'NONE',  ( -12.49999999999995914, 2.500000000000000000, 1.843143693225357538E-15 ) ) ;
#109982 = FACE_OUTER_BOUND ( 'NONE', #9851, .T. ) ;
#109983 = DIRECTION ( 'NONE',  ( 0.000000000000000000, 1.000000000000000000, 0.000000000000000000 ) ) ;
#109984 = LINE ( 'NONE', #103224, #21953 ) ;
#109985 = VERTEX_POINT ( 'NONE', #116 ) ;
#109986 = ORIENTED_EDGE ( 'NONE', *, *, #91397, .T. ) ;
#109987 = DIRECTION ( 'NONE',  ( -0.000000000000000000, 1.000000000000000000, -0.000000000000000000 ) ) ;
#109988 = EDGE_CURVE ( 'NONE', #27877, #41297, #120212, .T. ) ;
#109989 = ORIENTED_EDGE ( 'NONE', *, *, #110242, .F. ) ;
#109990 = CARTESIAN_POINT ( 'NONE',  ( -6.900000000000019007, 2.500000000000000000, 0.4464101615137735513 ) ) ;
#109991 = CARTESIAN_POINT ( 'NONE',  ( 7.899999999999923084, 12.50000000000000000, 0.6928203230275494784 ) ) ;
#109992 = FACE_OUTER_BOUND ( 'NONE', #45556, .T. ) ;
#109993 = ORIENTED_EDGE ( 'NONE', *, *, #61725, .T. ) ;
#109994 = DIRECTION ( 'NONE',  ( -0.000000000000000000, 1.000000000000000000, -0.000000000000000000 ) ) ;
#109995 = DIRECTION ( 'NONE',  ( 0.000000000000000000, 1.000000000000000000, 0.000000000000000000 ) ) ;
#109996 = CARTESIAN_POINT ( 'NONE',  ( -11.44999999999999929, 2.500000000000000000, -6.148780366869522673 ) ) ;
#109997 = EDGE_CURVE ( 'NONE', #73842, #59320, #19952, .T. ) ;
#109998 = EDGE_CURVE ( 'NONE', #55268, #52643, #17788, .T. ) ;
#109999 = DIRECTION ( 'NONE',  ( 0.000000000000000000, -1.000000000000000000, -0.000000000000000000 ) ) ;
#110000 = LINE ( 'NONE', #67461, #84143 ) ;
#110001 = EDGE_CURVE ( 'NONE', #126026, #17990, #99378, .T. ) ;
#110002 = EDGE_CURVE ( 'NONE', #89736, #83886, #55457, .T. ) ;
#110003 = CIRCLE ( 'NONE', #112151, 0.06509327318403745899 ) ;
#110004 = DIRECTION ( 'NONE',  ( 0.000000000000000000, 0.000000000000000000, -1.000000000000000000 ) ) ;
#110005 = EDGE_LOOP ( 'NONE', ( #115441, #72307 ) ) ;
#110006 = ORIENTED_EDGE ( 'NONE', *, *, #49597, .F. ) ;
#110007 = FACE_OUTER_BOUND ( 'NONE', #103726, .T. ) ;
#110008 = EDGE_LOOP ( 'NONE', ( #15848, #109417 ) ) ;
#110009 = CIRCLE ( 'NONE', #106081, 0.06509327318403745899 ) ;
#110010 = FACE_OUTER_BOUND ( 'NONE', #114345, .T. ) ;
#110012 = ORIENTED_EDGE ( 'NONE', *, *, #124031, .F. ) ;
#110011 = ORIENTED_EDGE ( 'NONE', *, *, #108993, .T. ) ;
#110013 = AXIS2_PLACEMENT_3D ( 'NONE', #69241, #50271, #71186 ) ;
#110014 = VERTEX_POINT ( 'NONE', #123133 ) ;
#110015 = EDGE_CURVE ( 'NONE', #106414, #27768, #13799, .T. ) ;
#110016 = CARTESIAN_POINT ( 'NONE',  ( 87.50000000000000000, -1.433398978532513413, -7.395196794792769701 ) ) ;
#110017 = CONICAL_SURFACE ( 'NONE', #101695, 0.1000000000000002554, 0.003490658503988666988 ) ;
#110018 = ADVANCED_FACE ( 'NONE', ( #122492 ), #13675, .T. ) ;
#110019 = FACE_OUTER_BOUND ( 'NONE', #116246, .T. ) ;
#110020 = EDGE_CURVE ( 'NONE', #94676, #8586, #9485, .T. ) ;
#110021 = FACE_OUTER_BOUND ( 'NONE', #5952, .T. ) ;
#110022 = CIRCLE ( 'NONE', #13847, 0.06509327318403745899 ) ;
#110023 = DIRECTION ( 'NONE',  ( 0.000000000000000000, -0.9999939076577903929, 0.003490651415223739937 ) ) ;
#110024 = DIRECTION ( 'NONE',  ( -4.274815082592931898E-19, -0.9999939076577903929, -0.003490651415223739937 ) ) ;
#110025 = CARTESIAN_POINT ( 'NONE',  ( 2.499999999999983569, 2.500000000000000000, -4.230127018922201998 ) ) ;
#110026 = PLANE ( 'NONE',  #24660 ) ;
#110027 = CARTESIAN_POINT ( 'NONE',  ( 9.349999999999919709, 2.500000000000000000, 2.511473670974873507 ) ) ;
#110028 = PLANE ( 'NONE',  #106303 ) ;
#110029 = VECTOR ( 'NONE', #29940, 1000.000000000000000 ) ;
#110030 = ORIENTED_EDGE ( 'NONE', *, *, #5526, .T. ) ;
#110032 = AXIS2_PLACEMENT_3D ( 'NONE', #63470, #62825, #52350 ) ;
#110031 = CIRCLE ( 'NONE', #124696, 0.06509327318403745899 ) ;
#110033 = DIRECTION ( 'NONE',  ( 1.000000000000000000, 0.000000000000000000, 0.000000000000000000 ) ) ;
#110034 = EDGE_LOOP ( 'NONE', ( #120864, #78566, #64851, #110035 ) ) ;
#110035 = ORIENTED_EDGE ( 'NONE', *, *, #1368, .F. ) ;
#110036 = DIRECTION ( 'NONE',  ( 0.000000000000000000, -0.000000000000000000, 1.000000000000000000 ) ) ;
#110037 = CARTESIAN_POINT ( 'NONE',  ( 5.599999999999931255, 2.500000000000000000, 3.983716857408420076 ) ) ;
#110038 = CARTESIAN_POINT ( 'NONE',  ( 186.9062500006828316, -8.891194145520236347, -1.633285867636356299E-15 ) ) ;
#110039 = CARTESIAN_POINT ( 'NONE',  ( 2.949999999999946887, 12.50000000000000000, -6.495190528383302464 ) ) ;
#110040 = LINE ( 'NONE', #100215, #38602 ) ;
#110041 = CARTESIAN_POINT ( 'NONE',  ( -1.250000000000036193, 2.500000000000000000, 1.572243186433545548 ) ) ;
#110042 = ORIENTED_EDGE ( 'NONE', *, *, #100965, .F. ) ;
#110043 = VERTEX_POINT ( 'NONE', #23634 ) ;
#110044 = FACE_OUTER_BOUND ( 'NONE', #45401, .T. ) ;
#110045 = VERTEX_POINT ( 'NONE', #92365 ) ;
#110046 = CARTESIAN_POINT ( 'NONE',  ( 186.4583333333333428, 4.445597072760147483, 7.699999999999948663 ) ) ;
#110047 = ORIENTED_EDGE ( 'NONE', *, *, #18401, .F. ) ;
#110048 = EDGE_CURVE ( 'NONE', #92609, #70125, #105636, .T. ) ;
#110049 = ORIENTED_EDGE ( 'NONE', *, *, #90607, .F. ) ;
#110050 = DIRECTION ( 'NONE',  ( 0.000000000000000000, -0.000000000000000000, 1.000000000000000000 ) ) ;
#110051 = DIRECTION ( 'NONE',  ( 0.000000000000000000, 0.000000000000000000, -1.000000000000000000 ) ) ;
#110052 = EDGE_CURVE ( 'NONE', #70966, #58229, #109835, .T. ) ;
#110053 = AXIS2_PLACEMENT_3D ( 'NONE', #119814, #20331, #21619 ) ;
#110054 = DIRECTION ( 'NONE',  ( 0.000000000000000000, -0.000000000000000000, 1.000000000000000000 ) ) ;
#110056 = FACE_OUTER_BOUND ( 'NONE', #11826, .T. ) ;
#110055 = AXIS2_PLACEMENT_3D ( 'NONE', #113272, #125653, #84466 ) ;
#110057 = EDGE_CURVE ( 'NONE', #116464, #22615, #80512, .T. ) ;
#110058 = CARTESIAN_POINT ( 'NONE',  ( -10.60000000000000142, 12.50000000000000000, 0.3464101615137736845 ) ) ;
#110059 = ORIENTED_EDGE ( 'NONE', *, *, #70107, .T. ) ;
#110060 = DIRECTION ( 'NONE',  ( -0.000000000000000000, 1.000000000000000000, -0.000000000000000000 ) ) ;
#110061 = DIRECTION ( 'NONE',  ( 0.000000000000000000, 0.000000000000000000, -1.000000000000000000 ) ) ;
#110062 = CARTESIAN_POINT ( 'NONE',  ( 1.849999999999950573, 12.50000000000000000, -1.753560074763288679 ) ) ;
#110063 = DIRECTION ( 'NONE',  ( 0.000000000000000000, 0.000000000000000000, 1.000000000000000000 ) ) ;
#110064 = EDGE_CURVE ( 'NONE', #114100, #89801, #42659, .T. ) ;
#110066 = CIRCLE ( 'NONE', #11846, 0.06509327318403745899 ) ;
#110065 = CIRCLE ( 'NONE', #107994, 0.1000000000000002554 ) ;
#110067 = CARTESIAN_POINT ( 'NONE',  ( -2.300000000000033573, 2.500000000000000000, -3.983716857408426293 ) ) ;
#110068 = VERTEX_POINT ( 'NONE', #81899 ) ;
#110069 = ORIENTED_EDGE ( 'NONE', *, *, #84589, .F. ) ;
#110070 = LINE ( 'NONE', #38777, #27850 ) ;
#110071 = ORIENTED_EDGE ( 'NONE', *, *, #51081, .T. ) ;
#110072 = CIRCLE ( 'NONE', #53631, 0.09999999999999982514 ) ;
#110073 = DIRECTION ( 'NONE',  ( -0.000000000000000000, -1.000000000000000000, -0.000000000000000000 ) ) ;
#110074 = DIRECTION ( 'NONE',  ( -0.000000000000000000, 1.000000000000000000, -0.000000000000000000 ) ) ;
#110075 = CIRCLE ( 'NONE', #51597, 0.06509327318403745899 ) ;
#110076 = ORIENTED_EDGE ( 'NONE', *, *, #105236, .F. ) ;
#110077 = DIRECTION ( 'NONE',  ( -4.274815082592931898E-19, -0.9999939076577903929, -0.003490651415223739937 ) ) ;
#110078 = FACE_OUTER_BOUND ( 'NONE', #40771, .T. ) ;
#110079 = CARTESIAN_POINT ( 'NONE',  ( -2.050000000000032685, 12.50000000000000000, -2.099970236277064473 ) ) ;
#110080 = EDGE_CURVE ( 'NONE', #91594, #30984, #24068, .T. ) ;
#110081 = DIRECTION ( 'NONE',  ( 0.000000000000000000, 1.000000000000000000, 0.000000000000000000 ) ) ;
#110082 = CARTESIAN_POINT ( 'NONE',  ( -10.45000000000000462, 2.500000000000000000, -2.065063509461098068 ) ) ;
#110083 = ORIENTED_EDGE ( 'NONE', *, *, #23139, .F. ) ;
#110084 = CARTESIAN_POINT ( 'NONE',  ( 59.88086527148990967, 3.776023839181152031, -4.996434403472031605 ) ) ;
#110085 = CARTESIAN_POINT ( 'NONE',  ( 1.449999999999951772, 2.500000000000000000, -6.048780366869526581 ) ) ;
#110086 = LINE ( 'NONE', #129111, #111896 ) ;
#110087 = CIRCLE ( 'NONE', #3480, 0.06509327318403741736 ) ;
#110088 = ORIENTED_EDGE ( 'NONE', *, *, #36245, .T. ) ;
#110089 = CONICAL_SURFACE ( 'NONE', #36943, 0.1000000000000000472, 0.003490658503988666988 ) ;
#110090 = EDGE_CURVE ( 'NONE', #104330, #27804, #76392, .T. ) ;
#110091 = ORIENTED_EDGE ( 'NONE', *, *, #101185, .T. ) ;
#110092 = DIRECTION ( 'NONE',  ( -0.000000000000000000, -1.000000000000000000, -0.000000000000000000 ) ) ;
#110093 = DIRECTION ( 'NONE',  ( 0.000000000000000000, 1.000000000000000000, 0.000000000000000000 ) ) ;
#110094 = AXIS2_PLACEMENT_3D ( 'NONE', #93393, #73109, #34490 ) ;
#110095 = CARTESIAN_POINT ( 'NONE',  ( 130.5000000000000000, 0.5000000000000000000, 7.499999999999998224 ) ) ;
#110096 = AXIS2_PLACEMENT_3D ( 'NONE', #60084, #99998, #39165 ) ;
#110097 = ORIENTED_EDGE ( 'NONE', *, *, #98631, .T. ) ;
#110098 = DIRECTION ( 'NONE',  ( -0.000000000000000000, 1.000000000000000000, -0.000000000000000000 ) ) ;
#110099 = CIRCLE ( 'NONE', #72556, 0.09999999999999982514 ) ;
#110100 = CARTESIAN_POINT ( 'NONE',  ( -5.200000000000022382, 2.500000000000000000, 0.3464101615137735735 ) ) ;
#110101 = VERTEX_POINT ( 'NONE', #82575 ) ;
#110102 = CARTESIAN_POINT ( 'NONE',  ( -2.300000000000033573, 12.50000000000000000, 4.611443907251934426 ) ) ;
#110103 = AXIS2_PLACEMENT_3D ( 'NONE', #113869, #24202, #6448 ) ;
#110104 = EDGE_CURVE ( 'NONE', #48106, #11230, #82662, .T. ) ;
#110105 = ORIENTED_EDGE ( 'NONE', *, *, #50618, .F. ) ;
#110107 = CIRCLE ( 'NONE', #101711, 0.1000000000000002554 ) ;
#110106 = DIRECTION ( 'NONE',  ( -4.274815082592931898E-19, -0.9999939076577903929, -0.003490651415223739937 ) ) ;
#110109 = CIRCLE ( 'NONE', #108140, 0.1000000000000002554 ) ;
#110108 = VECTOR ( 'NONE', #56066, 1000.000000000000000 ) ;
#110110 = VERTEX_POINT ( 'NONE', #72745 ) ;
#110111 = DIRECTION ( 'NONE',  ( 0.000000000000000000, 0.000000000000000000, -1.000000000000000000 ) ) ;
#110112 = LINE ( 'NONE', #13829, #77251 ) ;
#110113 = ORIENTED_EDGE ( 'NONE', *, *, #98876, .T. ) ;
#110114 = EDGE_CURVE ( 'NONE', #56654, #37929, #53406, .T. ) ;
#110115 = ORIENTED_EDGE ( 'NONE', *, *, #119772, .F. ) ;
#110116 = CARTESIAN_POINT ( 'NONE',  ( 6.049999999999934097, 2.500000000000000000, -2.511473670974877948 ) ) ;
#110117 = CARTESIAN_POINT ( 'NONE',  ( 4.399999999999937295, 2.500000000000000000, 3.883716857408421319 ) ) ;
#110118 = VERTEX_POINT ( 'NONE', #62289 ) ;
#110119 = CARTESIAN_POINT ( 'NONE',  ( -1.650000000000034772, 12.50000000000000000, 5.802370205355744659 ) ) ;
#110120 = DIRECTION ( 'NONE',  ( 0.000000000000000000, -0.000000000000000000, 1.000000000000000000 ) ) ;
#110121 = FACE_OUTER_BOUND ( 'NONE', #2529, .T. ) ;
#110122 = CARTESIAN_POINT ( 'NONE',  ( 9.549999999999918998, 12.50000000000000000, 2.165063509461097713 ) ) ;
#110123 = FACE_OUTER_BOUND ( 'NONE', #113824, .T. ) ;
#110124 = LINE ( 'NONE', #2085, #53582 ) ;
#110125 = DIRECTION ( 'NONE',  ( -0.000000000000000000, 1.000000000000000000, -0.000000000000000000 ) ) ;
#110126 = AXIS2_PLACEMENT_3D ( 'NONE', #99374, #9694, #29351 ) ;
#110127 = ORIENTED_EDGE ( 'NONE', *, *, #108201, .F. ) ;
#110129 = ORIENTED_EDGE ( 'NONE', *, *, #116176, .T. ) ;
#110128 = EDGE_CURVE ( 'NONE', #61045, #4682, #102209, .T. ) ;
#110130 = ORIENTED_EDGE ( 'NONE', *, *, #63740, .F. ) ;
#110131 = FACE_OUTER_BOUND ( 'NONE', #108870, .T. ) ;
#110132 = DIRECTION ( 'NONE',  ( 0.000000000000000000, 0.000000000000000000, -1.000000000000000000 ) ) ;
#110133 = CARTESIAN_POINT ( 'NONE',  ( 10.59999999999991260, 12.50000000000000000, 0.3464101615137735735 ) ) ;
#110135 = VERTEX_POINT ( 'NONE', #112670 ) ;
#110134 = VERTEX_POINT ( 'NONE', #43296 ) ;
#110136 = FACE_BOUND ( 'NONE', #40968, .T. ) ;
#110137 = EDGE_LOOP ( 'NONE', ( #80812, #13670, #74102, #2723 ) ) ;
#110138 = CARTESIAN_POINT ( 'NONE',  ( -7.100000000000017408, 12.50000000000000000, -0.6928203230275542523 ) ) ;
#110139 = DIRECTION ( 'NONE',  ( -0.000000000000000000, 1.000000000000000000, -0.000000000000000000 ) ) ;
#110141 = EDGE_CURVE ( 'NONE', #9133, #49498, #97217, .T. ) ;
#110140 = CARTESIAN_POINT ( 'NONE',  ( 11.04999999999990656, 2.500000000000000000, -6.048780366869526581 ) ) ;
#110142 = FACE_OUTER_BOUND ( 'NONE', #108313, .T. ) ;
#110143 = AXIS2_PLACEMENT_3D ( 'NONE', #40478, #79736, #119648 ) ;
#110144 = DIRECTION ( 'NONE',  ( 0.000000000000000000, -0.000000000000000000, 1.000000000000000000 ) ) ;
#110145 = CONICAL_SURFACE ( 'NONE', #53703, 0.1000000000000002554, 0.003490658503988666988 ) ;
#110146 = DIRECTION ( 'NONE',  ( 0.000000000000000000, 0.000000000000000000, -1.000000000000000000 ) ) ;
#110147 = LINE ( 'NONE', #109501, #35079 ) ;
#110148 = DIRECTION ( 'NONE',  ( 0.000000000000000000, 1.000000000000000000, 0.000000000000000000 ) ) ;
#110149 = EDGE_CURVE ( 'NONE', #105625, #83483, #55672, .T. ) ;
#110150 = EDGE_CURVE ( 'NONE', #127039, #97686, #117056, .T. ) ;
#110151 = CARTESIAN_POINT ( 'NONE',  ( -7.900000000000011013, 2.500000000000000000, 5.022947341949748790 ) ) ;
#110152 = ADVANCED_FACE ( 'NONE', ( #115205 ), #45002, .T. ) ;
#110153 = ADVANCED_FACE ( 'NONE', ( #85765 ), #5262, .T. ) ;
#110154 = DIRECTION ( 'NONE',  ( 0.000000000000000000, 0.000000000000000000, -1.000000000000000000 ) ) ;
#110155 = CIRCLE ( 'NONE', #24471, 0.1000000000000002554 ) ;
#110156 = EDGE_LOOP ( 'NONE', ( #4476, #119128 ) ) ;
#110157 = ORIENTED_EDGE ( 'NONE', *, *, #77205, .F. ) ;
#110158 = ORIENTED_EDGE ( 'NONE', *, *, #96650, .T. ) ;
#110159 = ORIENTED_EDGE ( 'NONE', *, *, #2436, .T. ) ;
#110160 = DIRECTION ( 'NONE',  ( 0.000000000000000000, 0.000000000000000000, 1.000000000000000000 ) ) ;
#110161 = EDGE_CURVE ( 'NONE', #112209, #85431, #61741, .T. ) ;
#110162 = DIRECTION ( 'NONE',  ( 0.000000000000000000, 0.000000000000000000, -1.000000000000000000 ) ) ;
#110165 = ORIENTED_EDGE ( 'NONE', *, *, #31437, .F. ) ;
#110164 = ORIENTED_EDGE ( 'NONE', *, *, #79319, .F. ) ;
#110163 = EDGE_CURVE ( 'NONE', #37879, #31124, #95168, .T. ) ;
#110166 = ORIENTED_EDGE ( 'NONE', *, *, #63155, .F. ) ;
#110167 = LINE ( 'NONE', #80061, #43840 ) ;
#110169 = CIRCLE ( 'NONE', #85014, 0.09999999999999999167 ) ;
#110168 = AXIS2_PLACEMENT_3D ( 'NONE', #129409, #55646, #37778 ) ;
#110170 = EDGE_CURVE ( 'NONE', #112646, #101562, #67392, .T. ) ;
#110171 = VECTOR ( 'NONE', #58474, 1000.000000000000000 ) ;
#110172 = EDGE_CURVE ( 'NONE', #1307, #70184, #41261, .T. ) ;
#110173 = CARTESIAN_POINT ( 'NONE',  ( 7.499999999999961808, 12.50000000000000000, -4.330127018922201643 ) ) ;
#110174 = DIRECTION ( 'NONE',  ( -0.000000000000000000, -1.000000000000000000, -0.000000000000000000 ) ) ;
#110175 = DIRECTION ( 'NONE',  ( 0.000000000000000000, 0.000000000000000000, 1.000000000000000000 ) ) ;
#110176 = PLANE ( 'NONE',  #24212 ) ;
#110177 = CARTESIAN_POINT ( 'NONE',  ( 5.449999999999936229, 2.500000000000000000, 6.395190528383296602 ) ) ;
#110178 = CARTESIAN_POINT ( 'NONE',  ( -0.8000000000000315747, 2.500000000000000000, 0.1000000000000000056 ) ) ;
#110179 = ORIENTED_EDGE ( 'NONE', *, *, #1749, .T. ) ;
#110180 = EDGE_CURVE ( 'NONE', #110134, #105827, #7201, .T. ) ;
#110181 = DIRECTION ( 'NONE',  ( -0.000000000000000000, -1.000000000000000000, -0.000000000000000000 ) ) ;
#110182 = ORIENTED_EDGE ( 'NONE', *, *, #36147, .F. ) ;
#110183 = VERTEX_POINT ( 'NONE', #45221 ) ;
#110184 = VERTEX_POINT ( 'NONE', #105427 ) ;
#110185 = DIRECTION ( 'NONE',  ( -0.000000000000000000, 1.000000000000000000, -0.000000000000000000 ) ) ;
#110186 = ORIENTED_EDGE ( 'NONE', *, *, #39520, .F. ) ;
#110187 = AXIS2_PLACEMENT_3D ( 'NONE', #68446, #89392, #129339 ) ;
#110188 = ORIENTED_EDGE ( 'NONE', *, *, #116064, .F. ) ;
#110190 = LINE ( 'NONE', #876, #84130 ) ;
#110189 = AXIS2_PLACEMENT_3D ( 'NONE', #3415, #42728, #82635 ) ;
#110192 = AXIS2_PLACEMENT_3D ( 'NONE', #60537, #100434, #110886 ) ;
#110191 = DIRECTION ( 'NONE',  ( 0.000000000000000000, 0.000000000000000000, 1.000000000000000000 ) ) ;
#110193 = DIRECTION ( 'NONE',  ( -0.000000000000000000, -1.000000000000000000, -0.000000000000000000 ) ) ;
#110194 = DIRECTION ( 'NONE',  ( -0.000000000000000000, 1.000000000000000000, -0.000000000000000000 ) ) ;
#110195 = CARTESIAN_POINT ( 'NONE',  ( 139.9358549477330200, 2.500000000000000000, -1.098523788719517169 ) ) ;
#110196 = AXIS2_PLACEMENT_3D ( 'NONE', #10171, #100475, #50111 ) ;
#110198 = VECTOR ( 'NONE', #75043, 1000.000000000000000 ) ;
#110197 = CARTESIAN_POINT ( 'NONE',  ( 8.349999999999919709, 2.500000000000000000, 5.702370205355745014 ) ) ;
#110199 = ORIENTED_EDGE ( 'NONE', *, *, #24921, .T. ) ;
#110200 = CARTESIAN_POINT ( 'NONE',  ( 18.45986578164203351, 0.7763536479255011002, 4.045836815165626099 ) ) ;
#110201 = ORIENTED_EDGE ( 'NONE', *, *, #4218, .F. ) ;
#110202 = DIRECTION ( 'NONE',  ( 0.000000000000000000, 0.000000000000000000, 1.000000000000000000 ) ) ;
#110203 = CARTESIAN_POINT ( 'NONE',  ( 185.0000000000000000, 0.000000000000000000, 7.700000000000000178 ) ) ;
#110204 = VERTEX_POINT ( 'NONE', #16997 ) ;
#110205 = DIRECTION ( 'NONE',  ( 0.000000000000000000, 1.000000000000000000, 0.000000000000000000 ) ) ;
#110206 = AXIS2_PLACEMENT_3D ( 'NONE', #76526, #84400, #124334 ) ;
#110207 = DIRECTION ( 'NONE',  ( 0.000000000000000000, -0.9999939076577903929, 0.003490651415223739937 ) ) ;
#110208 = EDGE_LOOP ( 'NONE', ( #122760, #54655 ) ) ;
#110209 = ADVANCED_FACE ( 'NONE', ( #26223 ), #88998, .T. ) ;
#110211 = CIRCLE ( 'NONE', #22495, 0.09999999999999982514 ) ;
#110210 = AXIS2_PLACEMENT_3D ( 'NONE', #81526, #101814, #102455 ) ;
#110212 = CARTESIAN_POINT ( 'NONE',  ( 4.149999999999941735, 12.50000000000000000, -7.122917578226816815 ) ) ;
#110213 = EDGE_CURVE ( 'NONE', #89563, #107837, #56937, .T. ) ;
#110214 = ORIENTED_EDGE ( 'NONE', *, *, #33764, .F. ) ;
#110215 = VERTEX_POINT ( 'NONE', #125686 ) ;
#110216 = DIRECTION ( 'NONE',  ( 0.000000000000000000, 1.000000000000000000, 0.000000000000000000 ) ) ;
#110217 = CARTESIAN_POINT ( 'NONE',  ( 11.69999999999990870, 12.50000000000000000, -4.395220292106239768 ) ) ;
#110218 = CARTESIAN_POINT ( 'NONE',  ( 4.549999999999939426, 12.50000000000000000, -6.495190528383302464 ) ) ;
#110219 = CARTESIAN_POINT ( 'NONE',  ( 1.449999999999950440, 2.500000000000000000, 6.148780366869520009 ) ) ;
#110220 = FACE_OUTER_BOUND ( 'NONE', #115334, .T. ) ;
#110221 = ORIENTED_EDGE ( 'NONE', *, *, #129542, .T. ) ;
#110222 = CARTESIAN_POINT ( 'NONE',  ( -7.499999999999976907, 12.50000000000000000, 4.265033745738159077 ) ) ;
#110223 = CIRCLE ( 'NONE', #20341, 0.06509327318403745899 ) ;
#110224 = ORIENTED_EDGE ( 'NONE', *, *, #76466, .T. ) ;
#110225 = DIRECTION ( 'NONE',  ( 0.000000000000000000, -0.000000000000000000, 1.000000000000000000 ) ) ;
#110226 = DIRECTION ( 'NONE',  ( -0.000000000000000000, -1.000000000000000000, -0.000000000000000000 ) ) ;
#110227 = CARTESIAN_POINT ( 'NONE',  ( 187.2135416670080588, 4.367472073101518859, -7.564683531249999149 ) ) ;
#110228 = DIRECTION ( 'NONE',  ( 0.000000000000000000, -0.9999939076577903929, 0.003490651415223739937 ) ) ;
#110229 = CARTESIAN_POINT ( 'NONE',  ( -1.250000000000001554, 2.500000000000000000, 2.165063509461097713 ) ) ;
#110230 = PLANE ( 'NONE',  #87835 ) ;
#110231 = DIRECTION ( 'NONE',  ( -0.000000000000000000, 1.000000000000000000, -0.000000000000000000 ) ) ;
#110232 = ORIENTED_EDGE ( 'NONE', *, *, #64334, .T. ) ;
#110233 = AXIS2_PLACEMENT_3D ( 'NONE', #119999, #78147, #119340 ) ;
#110234 = CARTESIAN_POINT ( 'NONE',  ( 9.149999999999916866, 2.500000000000000000, -1.372243186433550033 ) ) ;
#110235 = CONICAL_SURFACE ( 'NONE', #112390, 0.09999999999999982514, 0.003490658503988666988 ) ;
#110236 = CARTESIAN_POINT ( 'NONE',  ( 11.44999999999990870, 2.500000000000000000, -1.818653347947326138 ) ) ;
#110237 = DIRECTION ( 'NONE',  ( 0.000000000000000000, 1.000000000000000000, 0.000000000000000000 ) ) ;
#110238 = EDGE_LOOP ( 'NONE', ( #24043, #123382, #109800, #89479 ) ) ;
#110240 = AXIS2_PLACEMENT_3D ( 'NONE', #89617, #107969, #38605 ) ;
#110239 = VECTOR ( 'NONE', #2521, 1000.000000000000000 ) ;
#110241 = DIRECTION ( 'NONE',  ( 0.000000000000000000, 1.000000000000000000, 0.000000000000000000 ) ) ;
#110242 = EDGE_CURVE ( 'NONE', #118390, #42458, #74328, .T. ) ;
#110243 = AXIS2_PLACEMENT_3D ( 'NONE', #17083, #57703, #68144 ) ;
#110244 = ORIENTED_EDGE ( 'NONE', *, *, #23025, .F. ) ;
#110245 = VERTEX_POINT ( 'NONE', #85126 ) ;
#110246 = FACE_OUTER_BOUND ( 'NONE', #14931, .T. ) ;
#110247 = VERTEX_POINT ( 'NONE', #75949 ) ;
#110248 = DIRECTION ( 'NONE',  ( 0.000000000000000000, 0.000000000000000000, 1.000000000000000000 ) ) ;
#110249 = FACE_OUTER_BOUND ( 'NONE', #91521, .T. ) ;
#110250 = EDGE_LOOP ( 'NONE', ( #17842, #26265 ) ) ;
#110251 = AXIS2_PLACEMENT_3D ( 'NONE', #100318, #51865, #70854 ) ;
#110252 = CARTESIAN_POINT ( 'NONE',  ( -4.350000000000023626, 2.500000000000000000, 6.941600689897073018 ) ) ;
#110253 = LINE ( 'NONE', #18642, #39022 ) ;
#110254 = EDGE_CURVE ( 'NONE', #83521, #64553, #111990, .T. ) ;
#110255 = CARTESIAN_POINT ( 'NONE',  ( -10.80000000000000071, 12.50000000000000000, -2.276824562219559311E-15 ) ) ;
#110256 = EDGE_CURVE ( 'NONE', #27784, #103269, #55554, .T. ) ;
#110257 = VERTEX_POINT ( 'NONE', #106066 ) ;
#110258 = AXIS2_PLACEMENT_3D ( 'NONE', #65042, #95174, #123344 ) ;
#110259 = EDGE_LOOP ( 'NONE', ( #95426, #59230, #51533, #63650 ) ) ;
#110260 = ORIENTED_EDGE ( 'NONE', *, *, #78683, .F. ) ;
#110261 = FACE_OUTER_BOUND ( 'NONE', #58955, .T. ) ;
#110262 = DIRECTION ( 'NONE',  ( 0.000000000000000000, 1.000000000000000000, 0.000000000000000000 ) ) ;
#110263 = CARTESIAN_POINT ( 'NONE',  ( 6.449999999999930012, 12.50000000000000000, 6.841600689897072485 ) ) ;
#110264 = EDGE_CURVE ( 'NONE', #70439, #27091, #103674, .T. ) ;
#110265 = FACE_BOUND ( 'NONE', #118830, .T. ) ;
#110266 = ORIENTED_EDGE ( 'NONE', *, *, #77024, .T. ) ;
#110267 = AXIS2_PLACEMENT_3D ( 'NONE', #56840, #7104, #115113 ) ;
#110268 = DIRECTION ( 'NONE',  ( 0.000000000000000000, 1.000000000000000000, 0.000000000000000000 ) ) ;
#110269 = LINE ( 'NONE', #40916, #85781 ) ;
#110270 = VERTEX_POINT ( 'NONE', #96229 ) ;
#110271 = DIRECTION ( 'NONE',  ( 0.000000000000000000, 0.000000000000000000, -1.000000000000000000 ) ) ;
#110272 = DIRECTION ( 'NONE',  ( 0.000000000000000000, 1.000000000000000000, 0.000000000000000000 ) ) ;
#110273 =( GEOMETRIC_REPRESENTATION_CONTEXT ( 3 ) GLOBAL_UNCERTAINTY_ASSIGNED_CONTEXT ( ( #113553 ) ) GLOBAL_UNIT_ASSIGNED_CONTEXT ( ( #87993, #67056, #17311 ) ) REPRESENTATION_CONTEXT ( 'NONE', 'WORKASPACE' ) );
#110274 = DIRECTION ( 'NONE',  ( 0.000000000000000000, 0.000000000000000000, 1.000000000000000000 ) ) ;
#110275 = CARTESIAN_POINT ( 'NONE',  ( 3.349999999999941913, 12.50000000000000000, 6.495190528383297135 ) ) ;
#110276 = LINE ( 'NONE', #72301, #84316 ) ;
#110277 = CARTESIAN_POINT ( 'NONE',  ( 10.39999999999991154, 2.500000000000000000, -4.922947341949753586 ) ) ;
#110278 = AXIS2_PLACEMENT_3D ( 'NONE', #36263, #116095, #126570 ) ;
#110279 = CARTESIAN_POINT ( 'NONE',  ( 1.849999999999949685, 2.500000000000000000, -2.511473670974877948 ) ) ;
#110280 = CIRCLE ( 'NONE', #127016, 0.06509327318403745899 ) ;
#110281 = AXIS2_PLACEMENT_3D ( 'NONE', #65435, #104086, #46437 ) ;
#110282 = ORIENTED_EDGE ( 'NONE', *, *, #93955, .F. ) ;
#110283 = ORIENTED_EDGE ( 'NONE', *, *, #51331, .T. ) ;
#110284 = ORIENTED_EDGE ( 'NONE', *, *, #73148, .F. ) ;
#110285 = VERTEX_POINT ( 'NONE', #6529 ) ;
#110286 = DIRECTION ( 'NONE',  ( 0.000000000000000000, 0.000000000000000000, 1.000000000000000000 ) ) ;
#110287 = CARTESIAN_POINT ( 'NONE',  ( 6.049999999999932321, 2.500000000000000000, -1.718653347947326049 ) ) ;
#110288 = AXIS2_PLACEMENT_3D ( 'NONE', #16128, #126100, #73776 ) ;
#110289 = ORIENTED_EDGE ( 'NONE', *, *, #109079, .F. ) ;
#110290 = FACE_BOUND ( 'NONE', #117399, .T. ) ;
#110291 = CARTESIAN_POINT ( 'NONE',  ( 1.049999999999954969, 2.500000000000000000, -6.841600689897077814 ) ) ;
#110293 = ADVANCED_FACE ( 'NONE', ( #126353 ), #20055, .T. ) ;
#110292 = LINE ( 'NONE', #50728, #3102 ) ;
#110295 = VECTOR ( 'NONE', #68217, 1000.000000000000000 ) ;
#110294 = AXIS2_PLACEMENT_3D ( 'NONE', #121941, #42766, #32303 ) ;
#110296 = DIRECTION ( 'NONE',  ( -0.000000000000000000, 1.000000000000000000, -0.000000000000000000 ) ) ;
#110297 = CARTESIAN_POINT ( 'NONE',  ( 10.84999999999990905, 12.50000000000000000, -5.737276932171712751 ) ) ;
#110298 = CARTESIAN_POINT ( 'NONE',  ( 9.999999999999952038, 2.500000000000000000, 0.09999999999999772959 ) ) ;
#110299 = CARTESIAN_POINT ( 'NONE',  ( 8.949999999999921130, 2.500000000000000000, 1.718653347947321386 ) ) ;
#110300 = CARTESIAN_POINT ( 'NONE',  ( 1.649999999999949729, 2.500000000000000000, 7.188010851410848723 ) ) ;
#110301 = EDGE_CURVE ( 'NONE', #96482, #8842, #119110, .T. ) ;
#110302 = DIRECTION ( 'NONE',  ( 0.000000000000000000, 1.000000000000000000, 0.000000000000000000 ) ) ;
#110303 = ORIENTED_EDGE ( 'NONE', *, *, #15271, .F. ) ;
#110304 = EDGE_CURVE ( 'NONE', #119380, #25933, #90941, .T. ) ;
#110305 = ORIENTED_EDGE ( 'NONE', *, *, #3021, .T. ) ;
#110306 = EDGE_LOOP ( 'NONE', ( #6431, #15898, #45621, #46552 ) ) ;
#110307 = VERTEX_POINT ( 'NONE', #41218 ) ;
#110308 = ORIENTED_EDGE ( 'NONE', *, *, #72742, .F. ) ;
#110309 = ORIENTED_EDGE ( 'NONE', *, *, #87035, .F. ) ;
#110310 = EDGE_CURVE ( 'NONE', #114671, #93896, #50366, .T. ) ;
#110312 = EDGE_CURVE ( 'NONE', #75076, #104576, #119747, .T. ) ;
#110311 = LINE ( 'NONE', #41598, #90255 ) ;
#110314 = EDGE_LOOP ( 'NONE', ( #50436, #59329 ) ) ;
#110313 = ADVANCED_FACE ( 'NONE', ( #109282 ), #60837, .T. ) ;
#110315 = CIRCLE ( 'NONE', #53879, 0.06509327318403745899 ) ;
#110316 = DIRECTION ( 'NONE',  ( -0.000000000000000000, 1.000000000000000000, -0.000000000000000000 ) ) ;
#110318 = EDGE_CURVE ( 'NONE', #97447, #31133, #100740, .T. ) ;
#110317 = DIRECTION ( 'NONE',  ( -0.000000000000000000, -1.000000000000000000, -0.000000000000000000 ) ) ;
#110319 = CARTESIAN_POINT ( 'NONE',  ( 184.2760416670080588, 6.551208109652274736, 3.782341765625001351 ) ) ;
#110320 = DIRECTION ( 'NONE',  ( 0.000000000000000000, 0.000000000000000000, 1.000000000000000000 ) ) ;
#110321 = FACE_OUTER_BOUND ( 'NONE', #8745, .T. ) ;
#110322 = EDGE_LOOP ( 'NONE', ( #53967, #71207 ) ) ;
#110323 = FACE_OUTER_BOUND ( 'NONE', #46064, .T. ) ;
#110324 = EDGE_CURVE ( 'NONE', #1853, #36682, #72283, .T. ) ;
#110325 = AXIS2_PLACEMENT_3D ( 'NONE', #123842, #66215, #6620 ) ;
#110326 = EDGE_LOOP ( 'NONE', ( #106094, #90457 ) ) ;
#110327 = VECTOR ( 'NONE', #33465, 1000.000000000000000 ) ;
#110328 = ORIENTED_EDGE ( 'NONE', *, *, #48962, .T. ) ;
#110329 = DIRECTION ( 'NONE',  ( -0.000000000000000000, -1.000000000000000000, -0.000000000000000000 ) ) ;
#110330 = LINE ( 'NONE', #71693, #124140 ) ;
#110331 = DIRECTION ( 'NONE',  ( 0.000000000000000000, 0.000000000000000000, -1.000000000000000000 ) ) ;
#110332 = ORIENTED_EDGE ( 'NONE', *, *, #126602, .T. ) ;
#110334 = ORIENTED_EDGE ( 'NONE', *, *, #60059, .T. ) ;
#110333 = AXIS2_PLACEMENT_3D ( 'NONE', #23575, #19210, #98414 ) ;
#110335 = CARTESIAN_POINT ( 'NONE',  ( 14.34999999999989662, 2.500000000000000000, 1.718653347947321386 ) ) ;
#110336 = VECTOR ( 'NONE', #81978, 1000.000000000000000 ) ;
#110337 = DIRECTION ( 'NONE',  ( 0.000000000000000000, 1.000000000000000000, 0.000000000000000000 ) ) ;
#110338 = CARTESIAN_POINT ( 'NONE',  ( 10.59999999999990905, 12.50000000000000000, -3.983716857408426293 ) ) ;
#110339 = DIRECTION ( 'NONE',  ( 0.000000000000000000, 0.000000000000000000, 1.000000000000000000 ) ) ;
#110340 = EDGE_LOOP ( 'NONE', ( #107410, #887, #87745, #5962 ) ) ;
#110341 = DIRECTION ( 'NONE',  ( 0.000000000000000000, 0.000000000000000000, -1.000000000000000000 ) ) ;
#110342 = VERTEX_POINT ( 'NONE', #19623 ) ;
#110343 = CARTESIAN_POINT ( 'NONE',  ( 7.049999999999926992, 12.50000000000000000, 2.165063509461097713 ) ) ;
#110344 = ORIENTED_EDGE ( 'NONE', *, *, #112660, .T. ) ;
#110345 = DIRECTION ( 'NONE',  ( 0.000000000000000000, 1.000000000000000000, 0.000000000000000000 ) ) ;
#110346 = CARTESIAN_POINT ( 'NONE',  ( 1.449999999999952660, 12.50000000000000000, -6.841600689897078702 ) ) ;
#110347 = DIRECTION ( 'NONE',  ( 0.000000000000000000, 1.000000000000000000, 0.000000000000000000 ) ) ;
#110348 = AXIS2_PLACEMENT_3D ( 'NONE', #20547, #32963, #898 ) ;
#110349 = DIRECTION ( 'NONE',  ( -4.274815082592931898E-19, -0.9999939076577903929, -0.003490651415223739937 ) ) ;
#110350 = ORIENTED_EDGE ( 'NONE', *, *, #23081, .F. ) ;
#110351 = CARTESIAN_POINT ( 'NONE',  ( -1.650000000000035216, 2.500000000000000000, -5.702370205355749455 ) ) ;
#110352 = EDGE_CURVE ( 'NONE', #71169, #117955, #15826, .T. ) ;
#110353 = CARTESIAN_POINT ( 'NONE',  ( 8.549999999999920774, 12.50000000000000000, 6.148780366869520897 ) ) ;
#110354 = EDGE_LOOP ( 'NONE', ( #76195, #76004, #22901, #128354 ) ) ;
#110355 = ORIENTED_EDGE ( 'NONE', *, *, #81961, .F. ) ;
#110356 = ORIENTED_EDGE ( 'NONE', *, *, #51694, .F. ) ;
#110357 = FACE_OUTER_BOUND ( 'NONE', #41624, .T. ) ;
#110358 = CARTESIAN_POINT ( 'NONE',  ( 4.199999999999938005, 12.50000000000000000, 4.265033745738159077 ) ) ;
#110359 = CARTESIAN_POINT ( 'NONE',  ( 18.70618316910014656, 2.558637580971261816, 2.503050677946378144 ) ) ;
#110360 = LINE ( 'NONE', #1051, #14496 ) ;
#110362 = AXIS2_PLACEMENT_3D ( 'NONE', #110649, #20982, #121114 ) ;
#110361 = DIRECTION ( 'NONE',  ( 0.000000000000000000, 0.000000000000000000, -1.000000000000000000 ) ) ;
#110363 = DIRECTION ( 'NONE',  ( -0.000000000000000000, -1.000000000000000000, -0.000000000000000000 ) ) ;
#110364 = EDGE_CURVE ( 'NONE', #18875, #120364, #86929, .T. ) ;
#110365 = AXIS2_PLACEMENT_3D ( 'NONE', #80795, #71599, #111524 ) ;
#110366 = CARTESIAN_POINT ( 'NONE',  ( -3.749999999999991562, 2.500000000000000000, 6.495190528383297135 ) ) ;
#110367 = DIRECTION ( 'NONE',  ( 0.000000000000000000, 1.000000000000000000, 0.000000000000000000 ) ) ;
#110368 = DIRECTION ( 'NONE',  ( 1.000000000000000000, 0.000000000000000000, 0.000000000000000000 ) ) ;
#110369 = AXIS2_PLACEMENT_3D ( 'NONE', #47363, #97102, #87270 ) ;
#110370 = CIRCLE ( 'NONE', #36938, 0.1000000000000000472 ) ;
#110371 = CONICAL_SURFACE ( 'NONE', #97764, 0.1000000000000002554, 0.003490658503988666988 ) ;
#110372 = ORIENTED_EDGE ( 'NONE', *, *, #22584, .T. ) ;
#110373 = CARTESIAN_POINT ( 'NONE',  ( 11.64999999999990266, 2.500000000000000000, -6.495190528383302464 ) ) ;
#110374 = AXIS2_PLACEMENT_3D ( 'NONE', #32868, #72770, #3379 ) ;
#110375 = DIRECTION ( 'NONE',  ( -1.000000000000000000, -0.000000000000000000, -0.000000000000000000 ) ) ;
#110376 = DIRECTION ( 'NONE',  ( 0.000000000000000000, 0.000000000000000000, 1.000000000000000000 ) ) ;
#110377 = PLANE ( 'NONE',  #47969 ) ;
#110378 = VERTEX_POINT ( 'NONE', #9799 ) ;
#110379 = LINE ( 'NONE', #98607, #67543 ) ;
#110381 = AXIS2_PLACEMENT_3D ( 'NONE', #111348, #32830, #14439 ) ;
#110380 = AXIS2_PLACEMENT_3D ( 'NONE', #124199, #44342, #42429 ) ;
#110382 = FACE_OUTER_BOUND ( 'NONE', #85409, .T. ) ;
#110384 = ORIENTED_EDGE ( 'NONE', *, *, #27680, .F. ) ;
#110383 = FACE_OUTER_BOUND ( 'NONE', #52494, .T. ) ;
#110385 = ORIENTED_EDGE ( 'NONE', *, *, #53673, .T. ) ;
#110386 = DIRECTION ( 'NONE',  ( 0.000000000000000000, 0.000000000000000000, 1.000000000000000000 ) ) ;
#110387 = EDGE_CURVE ( 'NONE', #46747, #48610, #63957, .T. ) ;
#110388 = ORIENTED_EDGE ( 'NONE', *, *, #20352, .F. ) ;
#110389 = ORIENTED_EDGE ( 'NONE', *, *, #117350, .T. ) ;
#110390 = LINE ( 'NONE', #71768, #128206 ) ;
#110391 = DIRECTION ( 'NONE',  ( 0.000000000000000000, 0.000000000000000000, -1.000000000000000000 ) ) ;
#110392 = CARTESIAN_POINT ( 'NONE',  ( -1.322875655532295136, -1.500000000000000222, -5.000000000000004441 ) ) ;
#110393 = DIRECTION ( 'NONE',  ( -0.000000000000000000, 1.000000000000000000, -0.000000000000000000 ) ) ;
#110394 = EDGE_CURVE ( 'NONE', #112569, #71600, #107775, .T. ) ;
#110395 = ORIENTED_EDGE ( 'NONE', *, *, #85496, .T. ) ;
#110396 = VECTOR ( 'NONE', #102728, 1000.000000000000000 ) ;
#110397 = AXIS2_PLACEMENT_3D ( 'NONE', #15650, #5830, #45789 ) ;
#110398 = DIRECTION ( 'NONE',  ( 0.000000000000000000, 0.000000000000000000, 1.000000000000000000 ) ) ;
#110399 = ORIENTED_EDGE ( 'NONE', *, *, #108839, .F. ) ;
#110400 = DIRECTION ( 'NONE',  ( -0.000000000000000000, -1.000000000000000000, -0.000000000000000000 ) ) ;
#110402 = EDGE_CURVE ( 'NONE', #54998, #117091, #80597, .T. ) ;
#110401 = CIRCLE ( 'NONE', #26791, 0.1000000000000002554 ) ;
#110403 = CARTESIAN_POINT ( 'NONE',  ( 17.49999999999999645, 2.500000000000056843, 3.093179327514578691 ) ) ;
#110404 = CARTESIAN_POINT ( 'NONE',  ( -5.400000000000020783, 2.500000000000000000, 5.022947341949748790 ) ) ;
#110405 = EDGE_CURVE ( 'NONE', #94349, #107710, #128299, .T. ) ;
#110406 = ORIENTED_EDGE ( 'NONE', *, *, #110264, .T. ) ;
#110407 = CONICAL_SURFACE ( 'NONE', #58104, 0.1000000000000002554, 0.003490658503988666988 ) ;
#110408 = AXIS2_PLACEMENT_3D ( 'NONE', #53523, #113730, #24059 ) ;
#110409 = ORIENTED_EDGE ( 'NONE', *, *, #20146, .F. ) ;
#110411 = ORIENTED_EDGE ( 'NONE', *, *, #81741, .T. ) ;
#110410 = ADVANCED_FACE ( 'NONE', ( #70651 ), #10440, .T. ) ;
#110412 = VERTEX_POINT ( 'NONE', #79201 ) ;
#110413 = ORIENTED_EDGE ( 'NONE', *, *, #102583, .T. ) ;
#110414 = DIRECTION ( 'NONE',  ( 0.000000000000000000, -0.9999939076577903929, 0.003490651415223739937 ) ) ;
#110415 = CARTESIAN_POINT ( 'NONE',  ( 9.112263991918691630, 2.499999999999745537, 9.392448312006688838 ) ) ;
#110416 = DIRECTION ( 'NONE',  ( 0.000000000000000000, -0.000000000000000000, 1.000000000000000000 ) ) ;
#110417 = EDGE_CURVE ( 'NONE', #86684, #102251, #126657, .T. ) ;
#110418 = FACE_BOUND ( 'NONE', #105231, .T. ) ;
#110419 = CARTESIAN_POINT ( 'NONE',  ( -12.69999999999999396, 12.50000000000000000, 0.3464101615137776813 ) ) ;
#110420 = CARTESIAN_POINT ( 'NONE',  ( 186.0312500006828031, 9.429780353434619030E-16, -7.700000000000000178 ) ) ;
#110421 = AXIS2_PLACEMENT_3D ( 'NONE', #123602, #36544, #33955 ) ;
#110422 = CARTESIAN_POINT ( 'NONE',  ( 12.29999999999990479, 12.50000000000000000, -3.983716857408426293 ) ) ;
#110423 = DIRECTION ( 'NONE',  ( 0.000000000000000000, 0.000000000000000000, 1.000000000000000000 ) ) ;
#110424 = AXIS2_PLACEMENT_3D ( 'NONE', #12994, #33325, #3212 ) ;
#110425 = CARTESIAN_POINT ( 'NONE',  ( -2.700000000000029932, 2.500000000000000000, -0.3464101615137782364 ) ) ;
#110426 = FACE_OUTER_BOUND ( 'NONE', #94376, .T. ) ;
#110427 = DIRECTION ( 'NONE',  ( 0.000000000000000000, 0.000000000000000000, 1.000000000000000000 ) ) ;
#110428 = AXIS2_PLACEMENT_3D ( 'NONE', #96129, #118347, #6426 ) ;
#110429 = DIRECTION ( 'NONE',  ( 0.000000000000000000, 0.000000000000000000, 1.000000000000000000 ) ) ;
#110430 = ORIENTED_EDGE ( 'NONE', *, *, #19875, .F. ) ;
#110431 = ORIENTED_EDGE ( 'NONE', *, *, #63749, .F. ) ;
#110432 = ORIENTED_EDGE ( 'NONE', *, *, #3334, .F. ) ;
#110433 = VERTEX_POINT ( 'NONE', #129602 ) ;
#110434 = AXIS2_PLACEMENT_3D ( 'NONE', #83956, #54500, #15861 ) ;
#110435 = PLANE ( 'NONE',  #114979 ) ;
#110436 = CARTESIAN_POINT ( 'NONE',  ( 5.599999999999933031, 2.500000000000000000, -0.3464101615137783474 ) ) ;
#110437 = FACE_BOUND ( 'NONE', #49793, .T. ) ;
#110438 = CARTESIAN_POINT ( 'NONE',  ( -9.150000000000009237, 2.500000000000000000, -2.165063509461101710 ) ) ;
#110439 = AXIS2_PLACEMENT_3D ( 'NONE', #124860, #44356, #4403 ) ;
#110440 = EDGE_CURVE ( 'NONE', #26624, #123305, #1163, .T. ) ;
#110441 = PRESENTATION_LAYER_ASSIGNMENT (  '', '', ( #102140 ) ) ;
#110442 = ORIENTED_EDGE ( 'NONE', *, *, #78978, .T. ) ;
#110443 = DIRECTION ( 'NONE',  ( 0.000000000000000000, 0.000000000000000000, 1.000000000000000000 ) ) ;
#110444 = DIRECTION ( 'NONE',  ( 0.000000000000000000, 1.000000000000000000, 0.000000000000000000 ) ) ;
#110445 = CARTESIAN_POINT ( 'NONE',  ( 107.5000000000000142, 2.449293598294706414E-16, 2.000000000000000000 ) ) ;
#110446 = DIRECTION ( 'NONE',  ( 0.000000000000000000, 0.000000000000000000, -1.000000000000000000 ) ) ;
#110447 = VERTEX_POINT ( 'NONE', #109945 ) ;
#110448 = VECTOR ( 'NONE', #85694, 1000.000000000000000 ) ;
#110449 = CARTESIAN_POINT ( 'NONE',  ( -11.84999999999999609, 12.50000000000000000, 1.818653347947321475 ) ) ;
#110450 = ADVANCED_FACE ( 'NONE', ( #90270 ), #612, .T. ) ;
#110451 = CIRCLE ( 'NONE', #114653, 0.06509327318403745899 ) ;
#110452 = ORIENTED_EDGE ( 'NONE', *, *, #44552, .T. ) ;
#110453 = ORIENTED_EDGE ( 'NONE', *, *, #36687, .F. ) ;
#110454 = ADVANCED_FACE ( 'NONE', ( #72598 ), #23483, .T. ) ;
#110455 = CARTESIAN_POINT ( 'NONE',  ( 5.599999999999931255, 12.50000000000000000, 4.676537180435972552 ) ) ;
#110456 = CARTESIAN_POINT ( 'NONE',  ( 129.5000000000000000, 0.000000000000000000, 7.700000000000000178 ) ) ;
#110457 = CIRCLE ( 'NONE', #47777, 0.06509327318403741736 ) ;
#110459 = VERTEX_POINT ( 'NONE', #101411 ) ;
#110458 = EDGE_CURVE ( 'NONE', #8336, #22036, #76485, .T. ) ;
#110460 = DIRECTION ( 'NONE',  ( -0.000000000000000000, -1.000000000000000000, -0.000000000000000000 ) ) ;
#110461 = ADVANCED_FACE ( 'NONE', ( #31391 ), #118240, .T. ) ;
#110462 = CARTESIAN_POINT ( 'NONE',  ( -3.300000000000028244, 2.500000000000000000, 4.330127018922196314 ) ) ;
#110463 = DIRECTION ( 'NONE',  ( 0.000000000000000000, 0.000000000000000000, -1.000000000000000000 ) ) ;
#110465 = EDGE_CURVE ( 'NONE', #21250, #55865, #30531, .T. ) ;
#110464 = DIRECTION ( 'NONE',  ( 0.000000000000000000, 1.000000000000000000, 0.000000000000000000 ) ) ;
#110466 = VERTEX_POINT ( 'NONE', #64057 ) ;
#110467 = AXIS2_PLACEMENT_3D ( 'NONE', #43657, #104487, #92750 ) ;
#110468 = FACE_OUTER_BOUND ( 'NONE', #62052, .T. ) ;
#110469 = ORIENTED_EDGE ( 'NONE', *, *, #103214, .F. ) ;
#110470 = FACE_OUTER_BOUND ( 'NONE', #76932, .T. ) ;
#110471 = ADVANCED_FACE ( 'NONE', ( #43795 ), #32589, .T. ) ;
#110474 = ADVANCED_FACE ( 'NONE', ( #11731 ), #84788, .T. ) ;
#110473 = CONICAL_SURFACE ( 'NONE', #87478, 0.09999999999999999167, 0.003490658503988666988 ) ;
#110472 = AXIS2_PLACEMENT_3D ( 'NONE', #94500, #82780, #73567 ) ;
#110475 = EDGE_LOOP ( 'NONE', ( #3029, #20975 ) ) ;
#110476 = DIRECTION ( 'NONE',  ( -0.000000000000000000, 1.000000000000000000, -0.000000000000000000 ) ) ;
#110477 = ORIENTED_EDGE ( 'NONE', *, *, #53586, .F. ) ;
#110478 = FACE_OUTER_BOUND ( 'NONE', #5675, .T. ) ;
#110479 = DIRECTION ( 'NONE',  ( -0.000000000000000000, 1.000000000000000000, -0.000000000000000000 ) ) ;
#110480 = CARTESIAN_POINT ( 'NONE',  ( -11.64999999999999680, 2.500000000000000000, -7.188010851410850499 ) ) ;
#110481 = DIRECTION ( 'NONE',  ( 0.000000000000000000, 1.000000000000000000, 0.000000000000000000 ) ) ;
#110482 = DIRECTION ( 'NONE',  ( 0.000000000000000000, 0.000000000000000000, 1.000000000000000000 ) ) ;
#110483 = ORIENTED_EDGE ( 'NONE', *, *, #117217, .T. ) ;
#110484 = ORIENTED_EDGE ( 'NONE', *, *, #113129, .F. ) ;
#110485 = EDGE_LOOP ( 'NONE', ( #108060, #27811 ) ) ;
#110486 = DIRECTION ( 'NONE',  ( 0.000000000000000000, 0.000000000000000000, 1.000000000000000000 ) ) ;
#110487 = DIRECTION ( 'NONE',  ( 0.000000000000000000, 0.000000000000000000, -1.000000000000000000 ) ) ;
#110488 = FACE_OUTER_BOUND ( 'NONE', #35084, .T. ) ;
#110491 = ORIENTED_EDGE ( 'NONE', *, *, #170, .T. ) ;
#110490 = VERTEX_POINT ( 'NONE', #41855 ) ;
#110489 = AXIS2_PLACEMENT_3D ( 'NONE', #40612, #21581, #61525 ) ;
#110492 = ORIENTED_EDGE ( 'NONE', *, *, #94052, .F. ) ;
#110493 = CARTESIAN_POINT ( 'NONE',  ( -10.65000000000000213, 12.50000000000000000, 1.818653347947321475 ) ) ;
#110494 = ORIENTED_EDGE ( 'NONE', *, *, #20669, .F. ) ;
#110495 = FACE_OUTER_BOUND ( 'NONE', #49791, .T. ) ;
#110496 = AXIS2_PLACEMENT_3D ( 'NONE', #62263, #31500, #41341 ) ;
#110498 = FACE_OUTER_BOUND ( 'NONE', #83806, .T. ) ;
#110497 = CIRCLE ( 'NONE', #108431, 0.1000000000000002554 ) ;
#110499 = CARTESIAN_POINT ( 'NONE',  ( -14.59999999999998366, 12.50000000000000000, -0.06509327318403752838 ) ) ;
#110500 = CIRCLE ( 'NONE', #31102, 0.06509327318403745899 ) ;
#110501 = LINE ( 'NONE', #79126, #115434 ) ;
#110502 = CARTESIAN_POINT ( 'NONE',  ( -12.09999999999999609, 2.500000000000000000, -3.537306695894647302 ) ) ;
#110503 = CARTESIAN_POINT ( 'NONE',  ( -1.450000000000035483, 2.500000000000000000, 1.818653347947321475 ) ) ;
#110504 = PLANE ( 'NONE',  #20721 ) ;
#110505 = CONICAL_SURFACE ( 'NONE', #125081, 0.1000000000000002554, 0.003490658503988666988 ) ;
#110506 = ORIENTED_EDGE ( 'NONE', *, *, #50606, .T. ) ;
#110508 = VERTEX_POINT ( 'NONE', #4457 ) ;
#110507 = VECTOR ( 'NONE', #38733, 1000.000000000000000 ) ;
#110510 = CARTESIAN_POINT ( 'NONE',  ( -12.09999999999999609, 12.50000000000000000, 0.6277270498435161272 ) ) ;
#110509 = CONICAL_SURFACE ( 'NONE', #95929, 0.09999999999999982514, 0.003490658503988666988 ) ;
#110511 = AXIS2_PLACEMENT_3D ( 'NONE', #12575, #62349, #173 ) ;
#110512 = CARTESIAN_POINT ( 'NONE',  ( 13.09999999999990195, 12.50000000000000000, -3.983716857408426293 ) ) ;
#110513 = EDGE_LOOP ( 'NONE', ( #32156, #14280, #2054, #62718 ) ) ;
#110514 = VERTEX_POINT ( 'NONE', #53604 ) ;
#110515 = CARTESIAN_POINT ( 'NONE',  ( 187.3593750003414016, 0.000000000000000000, 7.564683531250000925 ) ) ;
#110516 = CARTESIAN_POINT ( 'NONE',  ( 13.14999999999989733, 12.50000000000000000, -2.511473670974877948 ) ) ;
#110517 = DIRECTION ( 'NONE',  ( 0.000000000000000000, 0.000000000000000000, 1.000000000000000000 ) ) ;
#110518 = DIRECTION ( 'NONE',  ( 0.000000000000000000, -0.9999939076577903929, 0.003490651415223739937 ) ) ;
#110519 = DIRECTION ( 'NONE',  ( 0.000000000000000000, 0.000000000000000000, -1.000000000000000000 ) ) ;
#110520 = EDGE_CURVE ( 'NONE', #12748, #19409, #33958, .T. ) ;
#110521 = CIRCLE ( 'NONE', #129329, 0.1000000000000002554 ) ;
#110522 = DIRECTION ( 'NONE',  ( 0.000000000000000000, -0.9999939076577903929, 0.003490651415223739937 ) ) ;
#110523 = DIRECTION ( 'NONE',  ( 0.000000000000000000, -0.9999939076577903929, 0.003490651415223739937 ) ) ;
#110524 = CARTESIAN_POINT ( 'NONE',  ( -0.4000000000000339950, 12.50000000000000000, 0.6928203230275518099 ) ) ;
#110525 = PLANE ( 'NONE',  #8174 ) ;
#110526 = CONICAL_SURFACE ( 'NONE', #120994, 0.1000000000000000056, 0.003490658503988666988 ) ;
#110527 = ORIENTED_EDGE ( 'NONE', *, *, #118236, .T. ) ;
#110528 = EDGE_LOOP ( 'NONE', ( #15851, #84012, #17949, #76321 ) ) ;
#110529 = ORIENTED_EDGE ( 'NONE', *, *, #3901, .T. ) ;
#110530 = CONICAL_SURFACE ( 'NONE', #102222, 0.09999999999999982514, 0.003490658503988666988 ) ;
#110531 = ORIENTED_EDGE ( 'NONE', *, *, #120792, .F. ) ;
#110532 = EDGE_LOOP ( 'NONE', ( #87916, #105500, #37858, #18076 ) ) ;
#110533 = DIRECTION ( 'NONE',  ( 0.000000000000000000, 0.000000000000000000, 1.000000000000000000 ) ) ;
#110534 = DIRECTION ( 'NONE',  ( 0.000000000000000000, -0.000000000000000000, 1.000000000000000000 ) ) ;
#110535 = EDGE_LOOP ( 'NONE', ( #11396, #3340, #40340, #15253 ) ) ;
#110536 = FACE_OUTER_BOUND ( 'NONE', #60072, .T. ) ;
#110537 = CARTESIAN_POINT ( 'NONE',  ( -7.500000000000015099, 2.500000000000000000, -0.7928203230275542301 ) ) ;
#110538 = AXIS2_PLACEMENT_3D ( 'NONE', #29870, #69793, #107783 ) ;
#110539 = CARTESIAN_POINT ( 'NONE',  ( 4.149999999999941735, 12.50000000000000000, -2.857883832488653741 ) ) ;
#110541 = ORIENTED_EDGE ( 'NONE', *, *, #78736, .F. ) ;
#110540 = DIRECTION ( 'NONE',  ( 0.000000000000000000, -0.9999939076577903929, 0.003490651415223739937 ) ) ;
#110542 = LINE ( 'NONE', #60177, #9789 ) ;
#110543 = AXIS2_PLACEMENT_3D ( 'NONE', #45483, #85388, #99085 ) ;
#110544 = DIRECTION ( 'NONE',  ( -0.000000000000000000, 1.000000000000000000, -0.000000000000000000 ) ) ;
#110545 = EDGE_LOOP ( 'NONE', ( #85912, #101848 ) ) ;
#110546 = AXIS2_PLACEMENT_3D ( 'NONE', #26855, #127629, #107339 ) ;
#110547 = ORIENTED_EDGE ( 'NONE', *, *, #44817, .F. ) ;
#110548 = EDGE_LOOP ( 'NONE', ( #103068, #122476, #64422, #90475 ) ) ;
#110549 = ORIENTED_EDGE ( 'NONE', *, *, #76937, .F. ) ;
#110550 = CARTESIAN_POINT ( 'NONE',  ( -4.200000000000025935, 2.500000000000000000, 4.330127018922196314 ) ) ;
#110551 = CONICAL_SURFACE ( 'NONE', #100099, 0.1000000000000002554, 0.003490658503988666988 ) ;
#110552 = DIRECTION ( 'NONE',  ( 0.000000000000000000, 0.000000000000000000, 1.000000000000000000 ) ) ;
#110553 = DIRECTION ( 'NONE',  ( -0.000000000000000000, -1.000000000000000000, -0.000000000000000000 ) ) ;
#110554 = ADVANCED_FACE ( 'NONE', ( #61496 ), #5362, .T. ) ;
#110556 = AXIS2_PLACEMENT_3D ( 'NONE', #615, #11733, #109286 ) ;
#110555 = AXIS2_PLACEMENT_3D ( 'NONE', #61616, #75755, #72711 ) ;
#110557 = PLANE ( 'NONE',  #55 ) ;
#110558 = EDGE_LOOP ( 'NONE', ( #64532, #40127 ) ) ;
#110559 = DIRECTION ( 'NONE',  ( 0.000000000000000000, 1.000000000000000000, 0.000000000000000000 ) ) ;
#110560 = DIRECTION ( 'NONE',  ( 0.000000000000000000, 0.000000000000000000, 1.000000000000000000 ) ) ;
#110561 = EDGE_CURVE ( 'NONE', #85675, #89168, #61819, .T. ) ;
#110562 = DIRECTION ( 'NONE',  ( 0.000000000000000000, -0.9999939076577903929, 0.003490651415223739937 ) ) ;
#110563 = CARTESIAN_POINT ( 'NONE',  ( 10.59999999999991260, 2.500000000000000000, -0.2464101615137783419 ) ) ;
#110564 = EDGE_CURVE ( 'NONE', #113036, #43893, #99473, .T. ) ;
#110565 = ORIENTED_EDGE ( 'NONE', *, *, #105090, .F. ) ;
#110567 = CIRCLE ( 'NONE', #33321, 0.06509327318403745899 ) ;
#110566 = AXIS2_PLACEMENT_3D ( 'NONE', #44347, #15523, #124206 ) ;
#110568 = ORIENTED_EDGE ( 'NONE', *, *, #90036, .F. ) ;
#110569 = EDGE_CURVE ( 'NONE', #30363, #51458, #70314, .T. ) ;
#110571 = ORIENTED_EDGE ( 'NONE', *, *, #44976, .T. ) ;
#110570 = ADVANCED_FACE ( 'NONE', ( #71284 ), #82429, .T. ) ;
#110572 = CARTESIAN_POINT ( 'NONE',  ( 7.899999999999921307, 2.500000000000000000, 0.09999999999999761857 ) ) ;
#110573 = ADVANCED_FACE ( 'NONE', ( #62140 ), #45186, .T. ) ;
#110574 = CARTESIAN_POINT ( 'NONE',  ( -3.950000000000026379, 2.500000000000000000, -1.818653347947326138 ) ) ;
#110575 = EDGE_CURVE ( 'NONE', #127721, #95822, #80693, .T. ) ;
#110576 = FACE_BOUND ( 'NONE', #101734, .T. ) ;
#110577 = DIRECTION ( 'NONE',  ( -0.000000000000000000, 1.000000000000000000, -0.000000000000000000 ) ) ;
#110578 = DIRECTION ( 'NONE',  ( 0.000000000000000000, 0.000000000000000000, -1.000000000000000000 ) ) ;
#110579 = DIRECTION ( 'NONE',  ( 0.000000000000000000, -0.000000000000000000, 1.000000000000000000 ) ) ;
#110580 = CONICAL_SURFACE ( 'NONE', #8166, 0.09999999999999982514, 0.003490658503988666988 ) ;
#110581 = CARTESIAN_POINT ( 'NONE',  ( 8.349999999999919709, 2.500000000000000000, -2.857883832488653741 ) ) ;
#110582 = CARTESIAN_POINT ( 'NONE',  ( -6.450000000000014388, 2.500000000000000000, 1.718653347947321386 ) ) ;
#110583 = DIRECTION ( 'NONE',  ( 0.000000000000000000, 0.000000000000000000, 1.000000000000000000 ) ) ;
#110584 = EDGE_LOOP ( 'NONE', ( #105518, #2643, #112139, #3740 ) ) ;
#110585 = DIRECTION ( 'NONE',  ( -0.000000000000000000, -1.000000000000000000, -0.000000000000000000 ) ) ;
#110586 = AXIS2_PLACEMENT_3D ( 'NONE', #58874, #28129, #30074 ) ;
#110587 = AXIS2_PLACEMENT_3D ( 'NONE', #58227, #77204, #99436 ) ;
#110588 = LINE ( 'NONE', #100750, #64181 ) ;
#110589 = ORIENTED_EDGE ( 'NONE', *, *, #94180, .F. ) ;
#110590 = EDGE_LOOP ( 'NONE', ( #96907, #115739 ) ) ;
#110591 = PLANE ( 'NONE',  #85845 ) ;
#110592 = FACE_OUTER_BOUND ( 'NONE', #23772, .T. ) ;
#110593 = FACE_BOUND ( 'NONE', #99312, .T. ) ;
#110594 = CARTESIAN_POINT ( 'NONE',  ( 0.8499999999999553468, 2.500000000000000000, 1.572243186433545548 ) ) ;
#110595 = AXIS2_PLACEMENT_3D ( 'NONE', #109872, #30681, #42426 ) ;
#110596 = CIRCLE ( 'NONE', #116843, 0.06509327318403745899 ) ;
#110597 = FACE_OUTER_BOUND ( 'NONE', #24845, .T. ) ;
#110598 = VERTEX_POINT ( 'NONE', #102054 ) ;
#110600 = EDGE_CURVE ( 'NONE', #73675, #81499, #32694, .T. ) ;
#110599 = DIRECTION ( 'NONE',  ( 0.000000000000000000, 0.000000000000000000, 1.000000000000000000 ) ) ;
#110601 = CARTESIAN_POINT ( 'NONE',  ( 185.1666666666666856, -6.668395609140176816, -3.850000000000003642 ) ) ;
#110602 = CIRCLE ( 'NONE', #20728, 0.09999999999999982514 ) ;
#110603 = ORIENTED_EDGE ( 'NONE', *, *, #97307, .F. ) ;
#110604 = CARTESIAN_POINT ( 'NONE',  ( 5.849999999999932143, 12.50000000000000000, 1.472243186433545459 ) ) ;
#110605 = DIRECTION ( 'NONE',  ( -0.000000000000000000, -1.000000000000000000, -0.000000000000000000 ) ) ;
#110606 = CONICAL_SURFACE ( 'NONE', #83438, 0.1000000000000002554, 0.003490658503988666988 ) ;
#110607 = EDGE_CURVE ( 'NONE', #89861, #6770, #105814, .T. ) ;
#110608 = EDGE_CURVE ( 'NONE', #55865, #14057, #65984, .T. ) ;
#110609 = CARTESIAN_POINT ( 'NONE',  ( -4.400000000000028777, 12.50000000000000000, -4.676537180435978769 ) ) ;
#110610 = CYLINDRICAL_SURFACE ( 'NONE', #124139, 4.000000000000000000 ) ;
#110611 = ADVANCED_FACE ( 'NONE', ( #15584 ), #87025, .T. ) ;
#110612 = ORIENTED_EDGE ( 'NONE', *, *, #103502, .T. ) ;
#110613 = CARTESIAN_POINT ( 'NONE',  ( -5.400000000000023448, 12.50000000000000000, -4.395220292106239768 ) ) ;
#110614 = DIRECTION ( 'NONE',  ( 0.000000000000000000, 1.000000000000000000, 0.000000000000000000 ) ) ;
#110615 = DIRECTION ( 'NONE',  ( -0.000000000000000000, 1.000000000000000000, -0.000000000000000000 ) ) ;
#110616 = AXIS2_PLACEMENT_3D ( 'NONE', #99061, #8711, #61054 ) ;
#110617 = EDGE_CURVE ( 'NONE', #38921, #86526, #84977, .T. ) ;
#110618 = ORIENTED_EDGE ( 'NONE', *, *, #126373, .F. ) ;
#110619 = VERTEX_POINT ( 'NONE', #126851 ) ;
#110620 = EDGE_CURVE ( 'NONE', #92178, #29080, #53594, .T. ) ;
#110621 = CARTESIAN_POINT ( 'NONE',  ( 3.000000000000000000, 0.000000000000000000, -5.000000000000004441 ) ) ;
#110623 = ORIENTED_EDGE ( 'NONE', *, *, #82137, .F. ) ;
#110622 = EDGE_CURVE ( 'NONE', #67678, #98580, #1261, .T. ) ;
#110624 = FACE_OUTER_BOUND ( 'NONE', #124944, .T. ) ;
#110625 = DIRECTION ( 'NONE',  ( 0.000000000000000000, 0.000000000000000000, 1.000000000000000000 ) ) ;
#110626 = EDGE_CURVE ( 'NONE', #96049, #72066, #40996, .T. ) ;
#110627 = EDGE_CURVE ( 'NONE', #124289, #91471, #114123, .T. ) ;
#110628 = CARTESIAN_POINT ( 'NONE',  ( 9.149999999999916866, 12.50000000000000000, 5.802370205355744659 ) ) ;
#110629 = ORIENTED_EDGE ( 'NONE', *, *, #113353, .T. ) ;
#110630 = DIRECTION ( 'NONE',  ( 0.000000000000000000, 0.000000000000000000, -1.000000000000000000 ) ) ;
#110631 = DIRECTION ( 'NONE',  ( 0.000000000000000000, 1.000000000000000000, 0.000000000000000000 ) ) ;
#110632 = DIRECTION ( 'NONE',  ( 0.000000000000000000, 0.000000000000000000, -1.000000000000000000 ) ) ;
#110633 = LINE ( 'NONE', #40638, #97746 ) ;
#110634 = DIRECTION ( 'NONE',  ( 0.000000000000000000, 0.000000000000000000, 1.000000000000000000 ) ) ;
#110636 = EDGE_CURVE ( 'NONE', #95428, #65807, #95454, .T. ) ;
#110635 = DIRECTION ( 'NONE',  ( 0.000000000000000000, 1.000000000000000000, 0.000000000000000000 ) ) ;
#110637 = EDGE_LOOP ( 'NONE', ( #19935, #18848 ) ) ;
#110638 = ORIENTED_EDGE ( 'NONE', *, *, #17757, .F. ) ;
#110639 = CARTESIAN_POINT ( 'NONE',  ( -12.94999999999999218, 12.50000000000000000, -2.099970236277062252 ) ) ;
#110640 = ORIENTED_EDGE ( 'NONE', *, *, #100537, .T. ) ;
#110641 = CARTESIAN_POINT ( 'NONE',  ( 103.6920052614127030, 7.269452028459965298, 2.543125990730006336 ) ) ;
#110643 = EDGE_LOOP ( 'NONE', ( #127615, #51944, #61546, #63468 ) ) ;
#110642 = VERTEX_POINT ( 'NONE', #107192 ) ;
#110644 = ORIENTED_EDGE ( 'NONE', *, *, #69607, .F. ) ;
#110645 = AXIS2_PLACEMENT_3D ( 'NONE', #89874, #100355, #29674 ) ;
#110646 = CARTESIAN_POINT ( 'NONE',  ( 17.50000000000000000, -0.8333333333333287074, -3.999999999999996447 ) ) ;
#110647 = EDGE_CURVE ( 'NONE', #112093, #25877, #77102, .T. ) ;
#110648 = PLANE ( 'NONE',  #27648 ) ;
#110649 = CARTESIAN_POINT ( 'NONE',  ( 5.849999999999934808, 12.50000000000000000, -5.802370205355749988 ) ) ;
#110650 = VECTOR ( 'NONE', #41706, 1000.000000000000000 ) ;
#110651 = CARTESIAN_POINT ( 'NONE',  ( 10.64999999999990976, 12.50000000000000000, 2.511473670974873507 ) ) ;
#110652 = DIRECTION ( 'NONE',  ( -0.000000000000000000, 1.000000000000000000, -0.000000000000000000 ) ) ;
#110653 = FACE_OUTER_BOUND ( 'NONE', #83458, .T. ) ;
#110654 = DIRECTION ( 'NONE',  ( 0.000000000000000000, 0.000000000000000000, -1.000000000000000000 ) ) ;
#110655 = CARTESIAN_POINT ( 'NONE',  ( -14.14999999999998792, 12.50000000000000000, 2.792790559304615616 ) ) ;
#110656 = CIRCLE ( 'NONE', #127391, 0.1000000000000002554 ) ;
#110657 = CARTESIAN_POINT ( 'NONE',  ( 4.999999999999935163, 2.500000000000000000, 3.637306695894644726 ) ) ;
#110658 = AXIS2_PLACEMENT_3D ( 'NONE', #116832, #126009, #36374 ) ;
#110659 = EDGE_LOOP ( 'NONE', ( #51627, #67938, #108978, #2047 ) ) ;
#110660 = CARTESIAN_POINT ( 'NONE',  ( 11.64999999999990266, 2.500000000000000000, 2.065063509461097624 ) ) ;
#110661 = ORIENTED_EDGE ( 'NONE', *, *, #45852, .F. ) ;
#110662 = ORIENTED_EDGE ( 'NONE', *, *, #39245, .T. ) ;
#110663 = DIRECTION ( 'NONE',  ( 0.000000000000000000, 0.000000000000000000, -1.000000000000000000 ) ) ;
#110664 = CARTESIAN_POINT ( 'NONE',  ( 11.64999999999990798, 2.500000000000000000, 7.288010851410849256 ) ) ;
#110665 = DIRECTION ( 'NONE',  ( 0.000000000000000000, 0.000000000000000000, -1.000000000000000000 ) ) ;
#110666 = EDGE_CURVE ( 'NONE', #60337, #17483, #74425, .T. ) ;
#110667 = CARTESIAN_POINT ( 'NONE',  ( 2.499999999999983569, 12.50000000000000000, -4.330127018922201643 ) ) ;
#110668 = FACE_OUTER_BOUND ( 'NONE', #81294, .T. ) ;
#110670 = CONICAL_SURFACE ( 'NONE', #8259, 0.1000000000000000472, 0.003490658503988666988 ) ;
#110669 = DIRECTION ( 'NONE',  ( 0.000000000000000000, 1.000000000000000000, 0.000000000000000000 ) ) ;
#110671 = ORIENTED_EDGE ( 'NONE', *, *, #66472, .T. ) ;
#110672 = ORIENTED_EDGE ( 'NONE', *, *, #33794, .F. ) ;
#110674 = FACE_OUTER_BOUND ( 'NONE', #95121, .T. ) ;
#110673 = AXIS2_PLACEMENT_3D ( 'NONE', #75764, #65293, #64027 ) ;
#110675 = VERTEX_POINT ( 'NONE', #64695 ) ;
#110676 = CARTESIAN_POINT ( 'NONE',  ( -13.14999999999999147, 12.50000000000000000, -1.818653347947323917 ) ) ;
#110677 = ORIENTED_EDGE ( 'NONE', *, *, #33389, .F. ) ;
#110678 = EDGE_CURVE ( 'NONE', #99586, #98405, #82848, .T. ) ;
#110679 = VERTEX_POINT ( 'NONE', #6385 ) ;
#110681 = CONICAL_SURFACE ( 'NONE', #29139, 0.1000000000000002554, 0.003490658503988666988 ) ;
#110680 = CARTESIAN_POINT ( 'NONE',  ( 13.74999999999989875, 2.500000000000000000, 1.372243186433545370 ) ) ;
#110682 = DIRECTION ( 'NONE',  ( -0.000000000000000000, -1.000000000000000000, -0.000000000000000000 ) ) ;
#110683 = CONICAL_SURFACE ( 'NONE', #64716, 0.1000000000000002554, 0.003490658503988666988 ) ;
#110684 = CARTESIAN_POINT ( 'NONE',  ( 5.399999999999933742, 12.50000000000000000, 0.06509327318403504425 ) ) ;
#110685 = CARTESIAN_POINT ( 'NONE',  ( -7.700000000000010836, 2.500000000000000000, 3.883716857408421319 ) ) ;
#110686 = DIRECTION ( 'NONE',  ( 0.000000000000000000, 0.000000000000000000, 1.000000000000000000 ) ) ;
#110687 = EDGE_LOOP ( 'NONE', ( #89604, #47756 ) ) ;
#110688 = CARTESIAN_POINT ( 'NONE',  ( -3.550000000000028688, 2.500000000000000000, 6.841600689897072485 ) ) ;
#110689 = DIRECTION ( 'NONE',  ( 0.000000000000000000, 0.000000000000000000, -1.000000000000000000 ) ) ;
#110690 = DIRECTION ( 'NONE',  ( 0.000000000000000000, -0.9999939076577903929, 0.003490651415223739937 ) ) ;
#110691 = CARTESIAN_POINT ( 'NONE',  ( -8.100000000000013856, 12.50000000000000000, 0.3464101615137736845 ) ) ;
#110692 = AXIS2_PLACEMENT_3D ( 'NONE', #32862, #62314, #12540 ) ;
#110693 = CARTESIAN_POINT ( 'NONE',  ( -5.000000000000023093, 2.500000000000000000, 5.122947341949749323 ) ) ;
#110694 = CIRCLE ( 'NONE', #39630, 0.09999999999999982514 ) ;
#110695 = EDGE_LOOP ( 'NONE', ( #128214, #12590, #68149, #62915 ) ) ;
#110696 = VECTOR ( 'NONE', #34929, 1000.000000000000000 ) ;
#110697 = ORIENTED_EDGE ( 'NONE', *, *, #106319, .F. ) ;
#110698 = CARTESIAN_POINT ( 'NONE',  ( 195.0000000000000000, 0.000000000000000000, -3.500000000000000000 ) ) ;
#110699 = VERTEX_POINT ( 'NONE', #75169 ) ;
#110700 = CARTESIAN_POINT ( 'NONE',  ( 6.649999999999931077, 2.500000000000000000, -6.395190528383301931 ) ) ;
#110701 = DIRECTION ( 'NONE',  ( 0.000000000000000000, 0.000000000000000000, -1.000000000000000000 ) ) ;
#110702 = EDGE_CURVE ( 'NONE', #36641, #38962, #103764, .T. ) ;
#110703 = AXIS2_PLACEMENT_3D ( 'NONE', #73448, #102284, #4687 ) ;
#110704 = VERTEX_POINT ( 'NONE', #25397 ) ;
#110705 = CARTESIAN_POINT ( 'NONE',  ( 184.0000000000000000, 0.000000000000000000, 7.700000000000000178 ) ) ;
#110706 = DIRECTION ( 'NONE',  ( 0.000000000000000000, 1.000000000000000000, 0.000000000000000000 ) ) ;
#110707 = CARTESIAN_POINT ( 'NONE',  ( 2.499999999999981792, 2.500000000000000000, 4.230127018922196669 ) ) ;
#110708 = PLANE ( 'NONE',  #116574 ) ;
#110709 = EDGE_CURVE ( 'NONE', #91784, #126895, #65328, .T. ) ;
#110710 = DIRECTION ( 'NONE',  ( -0.000000000000000000, -1.000000000000000000, -0.000000000000000000 ) ) ;
#110711 = ORIENTED_EDGE ( 'NONE', *, *, #60626, .T. ) ;
#110712 = EDGE_CURVE ( 'NONE', #32237, #5152, #126751, .T. ) ;
#110713 = EDGE_CURVE ( 'NONE', #12498, #114933, #26073, .T. ) ;
#110714 = ADVANCED_FACE ( 'NONE', ( #56154 ), #17977, .T. ) ;
#110716 = EDGE_CURVE ( 'NONE', #73698, #110699, #51454, .T. ) ;
#110715 = CARTESIAN_POINT ( 'NONE',  ( 76.45228544977298668, 3.905198701529716487, -5.870122411652127781 ) ) ;
#110717 = EDGE_CURVE ( 'NONE', #43268, #2171, #66622, .T. ) ;
#110718 = CARTESIAN_POINT ( 'NONE',  ( -7.300000000000018474, 2.500000000000000000, -3.883716857408426648 ) ) ;
#110719 = CARTESIAN_POINT ( 'NONE',  ( 1.249999999999950262, 12.50000000000000000, 7.188010851410848723 ) ) ;
#110720 = DIRECTION ( 'NONE',  ( -4.274815082592931898E-19, -0.9999939076577903929, -0.003490651415223739937 ) ) ;
#110721 = ORIENTED_EDGE ( 'NONE', *, *, #44054, .F. ) ;
#110722 = VERTEX_POINT ( 'NONE', #96722 ) ;
#110724 = VECTOR ( 'NONE', #79742, 1000.000000000000000 ) ;
#110723 = CARTESIAN_POINT ( 'NONE',  ( 11.64999999999990266, 2.500000000000000000, -6.595190528383302109 ) ) ;
#110725 = CARTESIAN_POINT ( 'NONE',  ( -3.550000000000028688, 12.50000000000000000, 6.906693963081109722 ) ) ;
#110726 = ADVANCED_FACE ( 'NONE', ( #128138 ), #10293, .T. ) ;
#110727 = CARTESIAN_POINT ( 'NONE',  ( 9.349999999999919709, 2.500000000000000000, -6.841600689897078702 ) ) ;
#110728 = EDGE_LOOP ( 'NONE', ( #42351, #126293 ) ) ;
#110729 = EDGE_CURVE ( 'NONE', #86633, #63267, #120255, .T. ) ;
#110731 = EDGE_CURVE ( 'NONE', #118967, #40079, #84878, .T. ) ;
#110730 = CARTESIAN_POINT ( 'NONE',  ( 7.499999999999961808, 2.500000000000000000, 4.330127018922196314 ) ) ;
#110733 = CIRCLE ( 'NONE', #77288, 5.000000000000004441 ) ;
#110732 = AXIS2_PLACEMENT_3D ( 'NONE', #25871, #63864, #103137 ) ;
#110734 = DIRECTION ( 'NONE',  ( -0.000000000000000000, -1.000000000000000000, -0.000000000000000000 ) ) ;
#110735 = VECTOR ( 'NONE', #85342, 1000.000000000000000 ) ;
#110736 = VERTEX_POINT ( 'NONE', #60061 ) ;
#110737 = LINE ( 'NONE', #11243, #9225 ) ;
#110738 = ORIENTED_EDGE ( 'NONE', *, *, #81302, .T. ) ;
#110739 = CARTESIAN_POINT ( 'NONE',  ( -3.550000000000027356, 12.50000000000000000, -2.511473670974877948 ) ) ;
#110741 = AXIS2_PLACEMENT_3D ( 'NONE', #64200, #5275, #33476 ) ;
#110740 = AXIS2_PLACEMENT_3D ( 'NONE', #46620, #86545, #107482 ) ;
#110742 = VERTEX_POINT ( 'NONE', #9646 ) ;
#110743 = DIRECTION ( 'NONE',  ( -0.000000000000000000, 1.000000000000000000, -0.000000000000000000 ) ) ;
#110744 = FACE_OUTER_BOUND ( 'NONE', #91166, .T. ) ;
#110745 = ORIENTED_EDGE ( 'NONE', *, *, #39063, .F. ) ;
#110746 = ORIENTED_EDGE ( 'NONE', *, *, #82734, .T. ) ;
#110747 = DIRECTION ( 'NONE',  ( -0.000000000000000000, 1.000000000000000000, -0.000000000000000000 ) ) ;
#110748 = CARTESIAN_POINT ( 'NONE',  ( -4.600000000000024514, 12.50000000000000000, 5.022947341949748790 ) ) ;
#110749 = VERTEX_POINT ( 'NONE', #10900 ) ;
#110750 = DIRECTION ( 'NONE',  ( -0.000000000000000000, -1.000000000000000000, -0.000000000000000000 ) ) ;
#110751 = CARTESIAN_POINT ( 'NONE',  ( 185.9010416670080303, -4.367472073101520635, 7.564683531249999149 ) ) ;
#110752 = CARTESIAN_POINT ( 'NONE',  ( -8.150000000000014566, 2.500000000000000000, -6.148780366869520897 ) ) ;
#110753 = DIRECTION ( 'NONE',  ( 0.000000000000000000, 1.000000000000000000, 0.000000000000000000 ) ) ;
#110754 = DIRECTION ( 'NONE',  ( 0.000000000000000000, 0.000000000000000000, 1.000000000000000000 ) ) ;
#110755 = DIRECTION ( 'NONE',  ( -0.000000000000000000, 1.000000000000000000, -0.000000000000000000 ) ) ;
#110756 = DIRECTION ( 'NONE',  ( -0.000000000000000000, -1.000000000000000000, -0.000000000000000000 ) ) ;
#110757 = CONICAL_SURFACE ( 'NONE', #41748, 0.1000000000000000472, 0.003490658503988666988 ) ;
#110758 = VECTOR ( 'NONE', #6134, 1000.000000000000000 ) ;
#110759 = ORIENTED_EDGE ( 'NONE', *, *, #86774, .T. ) ;
#110760 = ORIENTED_EDGE ( 'NONE', *, *, #2090, .F. ) ;
#110761 = DIRECTION ( 'NONE',  ( 0.000000000000000000, 0.000000000000000000, -1.000000000000000000 ) ) ;
#110762 = VERTEX_POINT ( 'NONE', #99966 ) ;
#110763 = DIRECTION ( 'NONE',  ( -0.000000000000000000, -1.000000000000000000, -0.000000000000000000 ) ) ;
#110764 = DIRECTION ( 'NONE',  ( -0.000000000000000000, 1.000000000000000000, -0.000000000000000000 ) ) ;
#110765 = LINE ( 'NONE', #2096, #69966 ) ;
#110767 = VERTEX_POINT ( 'NONE', #37817 ) ;
#110766 = ORIENTED_EDGE ( 'NONE', *, *, #68521, .T. ) ;
#110768 = FACE_BOUND ( 'NONE', #12433, .T. ) ;
#110769 = ORIENTED_EDGE ( 'NONE', *, *, #72402, .T. ) ;
#110770 = ADVANCED_FACE ( 'NONE', ( #30595 ), #32684, .T. ) ;
#110771 = DIRECTION ( 'NONE',  ( 0.000000000000000000, 0.000000000000000000, 1.000000000000000000 ) ) ;
#110772 = CARTESIAN_POINT ( 'NONE',  ( -7.700000000000016165, 12.50000000000000000, 0.3464101615137735735 ) ) ;
#110773 = CONICAL_SURFACE ( 'NONE', #102381, 0.09999999999999982514, 0.003490658503988666988 ) ;
#110774 = EDGE_CURVE ( 'NONE', #12584, #49114, #99570, .T. ) ;
#110775 = CARTESIAN_POINT ( 'NONE',  ( -9.800000000000004263, 2.500000000000000000, -0.2464101615137783419 ) ) ;
#110776 = CARTESIAN_POINT ( 'NONE',  ( 1.449999999999951772, 2.500000000000000000, -6.148780366869526226 ) ) ;
#110777 = LINE ( 'NONE', #80696, #122377 ) ;
#110778 = EDGE_CURVE ( 'NONE', #88035, #87323, #59875, .T. ) ;
#110779 = DIRECTION ( 'NONE',  ( 0.000000000000000000, 0.000000000000000000, -1.000000000000000000 ) ) ;
#110780 = DIRECTION ( 'NONE',  ( 0.000000000000000000, 0.000000000000000000, -1.000000000000000000 ) ) ;
#110781 = DIRECTION ( 'NONE',  ( -0.000000000000000000, 1.000000000000000000, -0.000000000000000000 ) ) ;
#110782 = LINE ( 'NONE', #121900, #24503 ) ;
#110783 = CARTESIAN_POINT ( 'NONE',  ( 0.5999999999999560130, 2.500000000000000000, -3.983716857408426293 ) ) ;
#110784 = CIRCLE ( 'NONE', #12579, 0.06509327318403745899 ) ;
#110786 = EDGE_CURVE ( 'NONE', #47422, #124116, #20136, .T. ) ;
#110785 = CARTESIAN_POINT ( 'NONE',  ( 11.44999999999990692, 12.50000000000000000, 1.753560074763284016 ) ) ;
#110787 = AXIS2_PLACEMENT_3D ( 'NONE', #26365, #47939, #97668 ) ;
#110788 = ORIENTED_EDGE ( 'NONE', *, *, #88736, .T. ) ;
#110789 = VERTEX_POINT ( 'NONE', #39141 ) ;
#110790 = AXIS2_PLACEMENT_3D ( 'NONE', #100275, #62295, #90428 ) ;
#110791 = VERTEX_POINT ( 'NONE', #70495 ) ;
#110792 = ORIENTED_EDGE ( 'NONE', *, *, #104997, .T. ) ;
#110793 = CARTESIAN_POINT ( 'NONE',  ( 7.499999999999927169, 2.500000000000000000, 3.637306695894644726 ) ) ;
#110794 = DIRECTION ( 'NONE',  ( 0.000000000000000000, 0.000000000000000000, -1.000000000000000000 ) ) ;
#110796 = VERTEX_POINT ( 'NONE', #90117 ) ;
#110795 = EDGE_LOOP ( 'NONE', ( #106825, #50052 ) ) ;
#110797 = AXIS2_PLACEMENT_3D ( 'NONE', #97589, #67459, #47865 ) ;
#110798 = VERTEX_POINT ( 'NONE', #129453 ) ;
#110799 = CARTESIAN_POINT ( 'NONE',  ( 3.099999999999944134, 12.50000000000000000, 4.676537180435972552 ) ) ;
#110800 = DIRECTION ( 'NONE',  ( -0.000000000000000000, -1.000000000000000000, -0.000000000000000000 ) ) ;
#110801 =( LENGTH_UNIT ( ) NAMED_UNIT ( * ) SI_UNIT ( .MILLI., .METRE. ) );
#110802 = LINE ( 'NONE', #112108, #50123 ) ;
#110803 = DIRECTION ( 'NONE',  ( -0.000000000000000000, 1.000000000000000000, -0.000000000000000000 ) ) ;
#110804 = DIRECTION ( 'NONE',  ( -0.000000000000000000, 1.000000000000000000, -0.000000000000000000 ) ) ;
#110805 = CARTESIAN_POINT ( 'NONE',  ( 0.3999999999999568345, 12.50000000000000000, -5.022947341949754119 ) ) ;
#110806 = EDGE_CURVE ( 'NONE', #20024, #84209, #36866, .T. ) ;
#110807 = VERTEX_POINT ( 'NONE', #80330 ) ;
#110808 = CARTESIAN_POINT ( 'NONE',  ( -8.749999999999975131, 12.50000000000000000, 2.165063509461097713 ) ) ;
#110809 = ORIENTED_EDGE ( 'NONE', *, *, #23443, .F. ) ;
#110810 = VERTEX_POINT ( 'NONE', #79049 ) ;
#110811 = ORIENTED_EDGE ( 'NONE', *, *, #25160, .F. ) ;
#110812 = CARTESIAN_POINT ( 'NONE',  ( -1.450000000000035483, 2.500000000000000000, 1.718653347947321386 ) ) ;
#110813 = ORIENTED_EDGE ( 'NONE', *, *, #18075, .F. ) ;
#110814 = VERTEX_POINT ( 'NONE', #20755 ) ;
#110815 = ORIENTED_EDGE ( 'NONE', *, *, #112367, .F. ) ;
#110816 = DIRECTION ( 'NONE',  ( 0.000000000000000000, 0.000000000000000000, 1.000000000000000000 ) ) ;
#110817 = CARTESIAN_POINT ( 'NONE',  ( -1.900000000000034106, 2.500000000000000000, -3.983716857408426293 ) ) ;
#110818 = CARTESIAN_POINT ( 'NONE',  ( -8.350000000000012079, 2.500000000000000000, -2.857883832488653741 ) ) ;
#110819 = EDGE_CURVE ( 'NONE', #115252, #90867, #118952, .T. ) ;
#110820 = DIRECTION ( 'NONE',  ( 0.000000000000000000, 0.000000000000000000, 1.000000000000000000 ) ) ;
#110821 = CARTESIAN_POINT ( 'NONE',  ( 6.649999999999929301, 2.500000000000000000, -2.065063509461102065 ) ) ;
#110822 = AXIS2_PLACEMENT_3D ( 'NONE', #61248, #40327, #112286 ) ;
#110823 = LINE ( 'NONE', #61091, #21170 ) ;
#110824 = CARTESIAN_POINT ( 'NONE',  ( -10.85000000000000142, 2.500000000000000000, -2.165063509461097713 ) ) ;
#110825 = ORIENTED_EDGE ( 'NONE', *, *, #79699, .F. ) ;
#110826 = DIRECTION ( 'NONE',  ( 0.000000000000000000, 0.000000000000000000, -1.000000000000000000 ) ) ;
#110828 = CIRCLE ( 'NONE', #54393, 0.06509327318403745899 ) ;
#110827 = CIRCLE ( 'NONE', #54392, 0.1000000000000002554 ) ;
#110829 = ORIENTED_EDGE ( 'NONE', *, *, #69188, .F. ) ;
#110830 = CARTESIAN_POINT ( 'NONE',  ( 1.249999999999986899, 12.50000000000000000, 6.430097255199259010 ) ) ;
#110831 = DIRECTION ( 'NONE',  ( -4.274815082592931898E-19, -0.9999939076577903929, -0.003490651415223739937 ) ) ;
#110832 = EDGE_LOOP ( 'NONE', ( #111867, #52040, #75506, #11700 ) ) ;
#110833 = DIRECTION ( 'NONE',  ( 0.000000000000000000, -0.000000000000000000, 1.000000000000000000 ) ) ;
#110834 = ADVANCED_FACE ( 'NONE', ( #127496 ), #8347, .T. ) ;
#110835 = LINE ( 'NONE', #120672, #39521 ) ;
#110836 = ORIENTED_EDGE ( 'NONE', *, *, #71297, .T. ) ;
#110837 = AXIS2_PLACEMENT_3D ( 'NONE', #115681, #53073, #16179 ) ;
#110838 = CARTESIAN_POINT ( 'NONE',  ( -1.700000000000034817, 12.50000000000000000, -2.385244779468109755E-15 ) ) ;
#110839 = EDGE_LOOP ( 'NONE', ( #59207, #66243, #58520, #53372 ) ) ;
#110840 = VERTEX_POINT ( 'NONE', #98653 ) ;
#110841 = CARTESIAN_POINT ( 'NONE',  ( 127.5000000000000000, -1.500000000000000000, -2.598076211353316900 ) ) ;
#110842 = DIRECTION ( 'NONE',  ( 0.000000000000000000, 1.000000000000000000, 0.000000000000000000 ) ) ;
#110843 = DIRECTION ( 'NONE',  ( -4.274815082592931898E-19, -0.9999939076577903929, -0.003490651415223739937 ) ) ;
#110844 = DIRECTION ( 'NONE',  ( 0.000000000000000000, -0.9999939076577903929, 0.003490651415223739937 ) ) ;
#110845 = DIRECTION ( 'NONE',  ( -4.274815082592931898E-19, -0.9999939076577903929, -0.003490651415223739937 ) ) ;
#110846 = ORIENTED_EDGE ( 'NONE', *, *, #39742, .F. ) ;
#110847 = DIRECTION ( 'NONE',  ( -0.000000000000000000, 1.000000000000000000, -0.000000000000000000 ) ) ;
#110848 = EDGE_LOOP ( 'NONE', ( #38845, #5826 ) ) ;
#110849 = DIRECTION ( 'NONE',  ( 0.000000000000000000, 1.000000000000000000, 0.000000000000000000 ) ) ;
#110850 = CONICAL_SURFACE ( 'NONE', #46036, 0.1000000000000002554, 0.003490658503988666988 ) ;
#110851 = DIRECTION ( 'NONE',  ( 0.000000000000000000, 0.000000000000000000, 1.000000000000000000 ) ) ;
#110852 = CIRCLE ( 'NONE', #96265, 0.1000000000000000056 ) ;
#110853 = EDGE_CURVE ( 'NONE', #120047, #4792, #27999, .T. ) ;
#110854 = CARTESIAN_POINT ( 'NONE',  ( 187.0468750003414300, -8.734944146203032389, -1.604583208406768146E-15 ) ) ;
#110855 = DIRECTION ( 'NONE',  ( -0.000000000000000000, 1.000000000000000000, -0.000000000000000000 ) ) ;
#110856 = FACE_OUTER_BOUND ( 'NONE', #128999, .T. ) ;
#110857 = DIRECTION ( 'NONE',  ( 0.000000000000000000, 0.000000000000000000, 1.000000000000000000 ) ) ;
#110858 = CARTESIAN_POINT ( 'NONE',  ( 4.599999999999940137, 12.50000000000000000, -4.957854068765716882 ) ) ;
#110859 = ORIENTED_EDGE ( 'NONE', *, *, #83225, .F. ) ;
#110860 = CIRCLE ( 'NONE', #117112, 0.1000000000000002554 ) ;
#110861 = EDGE_CURVE ( 'NONE', #51834, #117332, #64047, .T. ) ;
#110862 = DIRECTION ( 'NONE',  ( 0.000000000000000000, 0.000000000000000000, -1.000000000000000000 ) ) ;
#110863 = LINE ( 'NONE', #21206, #85130 ) ;
#110864 = EDGE_CURVE ( 'NONE', #45163, #35141, #95353, .T. ) ;
#110865 = EDGE_CURVE ( 'NONE', #124496, #4260, #64134, .T. ) ;
#110866 = EDGE_CURVE ( 'NONE', #129005, #88166, #87113, .T. ) ;
#110867 = EDGE_CURVE ( 'NONE', #128878, #107859, #103854, .T. ) ;
#110868 = ORIENTED_EDGE ( 'NONE', *, *, #5515, .T. ) ;
#110869 = LINE ( 'NONE', #101064, #107503 ) ;
#110870 = CIRCLE ( 'NONE', #83707, 0.1000000000000000472 ) ;
#110871 = CIRCLE ( 'NONE', #69017, 0.09999999999999982514 ) ;
#110872 = VERTEX_POINT ( 'NONE', #120882 ) ;
#110873 = ORIENTED_EDGE ( 'NONE', *, *, #120967, .T. ) ;
#110874 = CARTESIAN_POINT ( 'NONE',  ( -3.550000000000027356, 2.500000000000000000, 1.818653347947321475 ) ) ;
#110875 = EDGE_CURVE ( 'NONE', #43219, #72747, #16003, .T. ) ;
#110876 = EDGE_CURVE ( 'NONE', #22096, #80261, #57793, .T. ) ;
#110877 = VERTEX_POINT ( 'NONE', #34938 ) ;
#110878 = DIRECTION ( 'NONE',  ( 0.000000000000000000, 0.000000000000000000, 1.000000000000000000 ) ) ;
#110879 = CARTESIAN_POINT ( 'NONE',  ( -3.350000000000028511, 2.500000000000000000, -1.472243186433550122 ) ) ;
#110880 = CARTESIAN_POINT ( 'NONE',  ( 12.89999999999990266, 2.500000000000000000, 3.637306695894644726 ) ) ;
#110881 = ADVANCED_FACE ( 'NONE', ( #114758 ), #7686, .T. ) ;
#110882 = ORIENTED_EDGE ( 'NONE', *, *, #71243, .F. ) ;
#110883 = EDGE_CURVE ( 'NONE', #74144, #1435, #34295, .T. ) ;
#110885 = ADVANCED_FACE ( 'NONE', ( #114122 ), #105906, .T. ) ;
#110884 = CARTESIAN_POINT ( 'NONE',  ( -0.8500000000000382805, 12.50000000000000000, -2.857883832488653741 ) ) ;
#110886 = DIRECTION ( 'NONE',  ( 0.000000000000000000, 0.000000000000000000, -1.000000000000000000 ) ) ;
#110887 = CIRCLE ( 'NONE', #73327, 0.1000000000000002554 ) ;
#110888 = DIRECTION ( 'NONE',  ( 0.000000000000000000, 0.000000000000000000, -1.000000000000000000 ) ) ;
#110889 = EDGE_CURVE ( 'NONE', #10941, #29719, #128920, .T. ) ;
#110890 = ORIENTED_EDGE ( 'NONE', *, *, #40031, .T. ) ;
#110891 = ORIENTED_EDGE ( 'NONE', *, *, #57832, .T. ) ;
#110892 = VERTEX_POINT ( 'NONE', #74851 ) ;
#110893 = CARTESIAN_POINT ( 'NONE',  ( -7.499999999999980460, 2.500000000000000000, -2.276824562219559311E-15 ) ) ;
#110894 = CARTESIAN_POINT ( 'NONE',  ( -5.200000000000020606, 12.50000000000000000, -0.4115034346978156399 ) ) ;
#110895 = LINE ( 'NONE', #120727, #27521 ) ;
#110896 = FACE_BOUND ( 'NONE', #50935, .T. ) ;
#110897 = ORIENTED_EDGE ( 'NONE', *, *, #43099, .T. ) ;
#110898 = PLANE ( 'NONE',  #111827 ) ;
#110899 = CARTESIAN_POINT ( 'NONE',  ( 5.849999999999933920, 2.500000000000000000, 6.395190528383296602 ) ) ;
#110900 = ORIENTED_EDGE ( 'NONE', *, *, #113838, .T. ) ;
#110901 = DIRECTION ( 'NONE',  ( -0.000000000000000000, -1.000000000000000000, -0.000000000000000000 ) ) ;
#110902 = DIRECTION ( 'NONE',  ( 0.000000000000000000, -0.000000000000000000, 1.000000000000000000 ) ) ;
#110904 = DIRECTION ( 'NONE',  ( 0.000000000000000000, 0.000000000000000000, 1.000000000000000000 ) ) ;
#110903 = CONICAL_SURFACE ( 'NONE', #52425, 0.1000000000000000472, 0.003490658503988666988 ) ;
#110905 = CARTESIAN_POINT ( 'NONE',  ( -8.100000000000013856, 2.500000000000000000, -4.083716857408426826 ) ) ;
#110906 = CARTESIAN_POINT ( 'NONE',  ( -5.000000000000023093, 2.500000000000000000, 5.022947341949748790 ) ) ;
#110907 = AXIS2_PLACEMENT_3D ( 'NONE', #53860, #16484, #75416 ) ;
#110908 = AXIS2_PLACEMENT_3D ( 'NONE', #111634, #31785, #42252 ) ;
#110909 = CARTESIAN_POINT ( 'NONE',  ( -10.00000000000000533, 2.500000000000000000, 0.6928203230275494784 ) ) ;
#110910 = LINE ( 'NONE', #22566, #50442 ) ;
#110911 = AXIS2_PLACEMENT_3D ( 'NONE', #98967, #59050, #60968 ) ;
#110912 = VERTEX_POINT ( 'NONE', #80970 ) ;
#110913 = ORIENTED_EDGE ( 'NONE', *, *, #103657, .F. ) ;
#110914 = ORIENTED_EDGE ( 'NONE', *, *, #111580, .F. ) ;
#110915 = EDGE_LOOP ( 'NONE', ( #70826, #39054, #54175, #82493 ) ) ;
#110916 = CARTESIAN_POINT ( 'NONE',  ( -12.49999999999999467, 2.500000000000000000, 0.6928203230275535862 ) ) ;
#110917 = LINE ( 'NONE', #21254, #4912 ) ;
#110918 = ORIENTED_EDGE ( 'NONE', *, *, #121126, .T. ) ;
#110919 = FACE_BOUND ( 'NONE', #22752, .T. ) ;
#110920 = LINE ( 'NONE', #59286, #98040 ) ;
#110921 = ADVANCED_FACE ( 'NONE', ( #105606 ), #65001, .T. ) ;
#110922 = DIRECTION ( 'NONE',  ( 0.000000000000000000, 1.000000000000000000, 0.000000000000000000 ) ) ;
#110923 = CARTESIAN_POINT ( 'NONE',  ( -4.150000000000028777, 12.50000000000000000, -5.737276932171712751 ) ) ;
#110924 = EDGE_CURVE ( 'NONE', #44638, #50039, #122635, .T. ) ;
#110925 = PLANE ( 'NONE',  #63811 ) ;
#110926 = CARTESIAN_POINT ( 'NONE',  ( 184.5000000000000000, -1.234829786877245983, 7.585434706901270197 ) ) ;
#110927 = DIRECTION ( 'NONE',  ( 0.000000000000000000, 1.000000000000000000, 0.000000000000000000 ) ) ;
#110928 = PLANE ( 'NONE',  #28257 ) ;
#110929 = FACE_OUTER_BOUND ( 'NONE', #82842, .T. ) ;
#110930 = ORIENTED_EDGE ( 'NONE', *, *, #77254, .T. ) ;
#110931 = EDGE_CURVE ( 'NONE', #20474, #13562, #25738, .T. ) ;
#110932 = ORIENTED_EDGE ( 'NONE', *, *, #90235, .T. ) ;
#110933 = ORIENTED_EDGE ( 'NONE', *, *, #126289, .F. ) ;
#110934 = ORIENTED_EDGE ( 'NONE', *, *, #124815, .T. ) ;
#110935 = VERTEX_POINT ( 'NONE', #55215 ) ;
#110936 = ORIENTED_EDGE ( 'NONE', *, *, #115442, .T. ) ;
#110937 = FACE_OUTER_BOUND ( 'NONE', #94017, .T. ) ;
#110938 = ORIENTED_EDGE ( 'NONE', *, *, #10809, .T. ) ;
#110939 = AXIS2_PLACEMENT_3D ( 'NONE', #22327, #13762, #43899 ) ;
#110940 = CIRCLE ( 'NONE', #54511, 0.1000000000000000056 ) ;
#110941 = CARTESIAN_POINT ( 'NONE',  ( 11.84999999999990727, 2.500000000000000000, 6.841600689897072485 ) ) ;
#110942 = CARTESIAN_POINT ( 'NONE',  ( 14.66596005923785206, -1.500000000000032641, 7.515560522276935274 ) ) ;
#110943 = CARTESIAN_POINT ( 'NONE',  ( 12.09999999999990195, 2.500000000000000000, -0.6928203230275541413 ) ) ;
#110944 = LINE ( 'NONE', #42237, #84421 ) ;
#110945 = ORIENTED_EDGE ( 'NONE', *, *, #21755, .T. ) ;
#110946 = PLANE ( 'NONE',  #127930 ) ;
#110947 = AXIS2_PLACEMENT_3D ( 'NONE', #8581, #48537, #88441 ) ;
#110948 = ORIENTED_EDGE ( 'NONE', *, *, #94914, .T. ) ;
#110949 = ORIENTED_EDGE ( 'NONE', *, *, #109076, .F. ) ;
#110950 = FACE_OUTER_BOUND ( 'NONE', #59838, .T. ) ;
#110951 = CARTESIAN_POINT ( 'NONE',  ( -12.29999999999999538, 2.500000000000000000, -0.3464101615137741841 ) ) ;
#110952 = CARTESIAN_POINT ( 'NONE',  ( -9.600000000000008527, 2.500000000000000000, -0.1000000000000023925 ) ) ;
#110953 =( BOUNDED_SURFACE ( )  B_SPLINE_SURFACE ( 1, 2, ( 
 ( #80665, #62317, #102235, #70831, #42691, #82600, #94324, #74056, #113986, #123779, #64866, #104782, #72769, #54409, #114615, #23028, #4639, #85797, #102853, #44599, #34141, #83864, #104160, #4014, #112699, #35432, #84520, #15099, #124449, #55062, #5938, #94993, #5301, #23667, #45247, #65517, #34798, #32867, #103522, #43961, #13832, #24311, #125088, #53768, #74702, #64233, #14466, #13181, #53134, #85162, #24954, #75334, #25582, #115230, #3378, #93065, #105456, #15766, #63601, #55697, #33505, #95633, #45892, #62943, #93696, #43325, #83245, #123161, #73401, #113328, #96909, #68093, #68745, #75986, #57647, #16393, #108019, #49131, #86442, #8518, #76638, #7884, #56338, #96254, #9183 ),
 ( #87729, #56974, #115907, #77278, #17023, #106096, #106726, #58934, #116551, #98842, #26893, #37996, #17699, #37372, #117172, #66796, #126384, #36726, #7227, #77913, #97557, #47185, #28185, #26254, #87085, #18355, #125710, #58299, #88365, #6564, #127664, #47836, #127041, #66159, #27511, #46515, #117827, #67422, #107382, #36068, #98201, #48463, #128336, #38670, #78592, #118481, #28837, #108667, #18987, #1928, #20939, #119139, #12396, #101433, #81156, #51697, #110601, #91609, #90969, #29473, #109970, #120430, #60861, #89038, #128987, #32066, #20294, #41883, #9826, #19654, #39323, #79226, #129617, #69382, #41241, #111225, #49777, #31413, #109312, #59605, #51060, #30778, #81774, #99514, #89679 ) ),
 .UNSPECIFIED., .F., .F., .F. ) 
 B_SPLINE_SURFACE_WITH_KNOTS ( ( 2, 2 ),
 ( 3, 2, 2, 2, 2, 2, 2, 2, 2, 2, 2, 2, 2, 2, 2, 2, 2, 2, 2, 2, 2, 2, 2, 2, 2, 2, 2, 2, 2, 2, 2, 2, 2, 2, 2, 2, 2, 2, 2, 2, 2, 2, 3 ),
 ( 0.000000000000000000, 1.000000000000000000 ),
 ( 0.000000000000000000, 0.02380952380952380820, 0.04761904761904761640, 0.07142857142857142461, 0.09523809523809523281, 0.1190476190476190410, 0.1428571428571428492, 0.1666666666666666574, 0.1904761904761904656, 0.2142857142857142738, 0.2380952380952380820, 0.2619047619047619180, 0.2857142857142856984, 0.3095238095238095344, 0.3333333333333333148, 0.3571428571428571508, 0.3809523809523809312, 0.4047619047619047672, 0.4285714285714285476, 0.4523809523809523836, 0.4761904761904761640, 0.5000000000000000000, 0.5238095238095238360, 0.5476190476190476719, 0.5714285714285713969, 0.5952380952380952328, 0.6190476190476190688, 0.6428571428571429047, 0.6666666666666666297, 0.6904761904761904656, 0.7142857142857143016, 0.7380952380952381375, 0.7619047619047618625, 0.7857142857142856984, 0.8095238095238095344, 0.8333333333333333703, 0.8571428571428570953, 0.8809523809523809312, 0.9047619047619047672, 0.9285714285714286031, 0.9523809523809523281, 0.9761904761904761640, 1.000000000000000000 ),
 .UNSPECIFIED. ) 
 GEOMETRIC_REPRESENTATION_ITEM ( )  RATIONAL_B_SPLINE_SURFACE ( (
 ( 1.000000000000000000, 0.8660254037844387076, 1.000000000000000000, 0.8660254037844387076, 1.000000000000000000, 0.8660254037844387076, 1.000000000000000000, 0.8660254037844387076, 1.000000000000000000, 0.8660254037844387076, 1.000000000000000000, 0.8660254037844387076, 1.000000000000000000, 0.8660254037844387076, 1.000000000000000000, 0.8660254037844387076, 1.000000000000000000, 0.8660254037844387076, 1.000000000000000000, 0.8660254037844387076, 1.000000000000000000, 0.8660254037844387076, 1.000000000000000000, 0.8660254037844387076, 1.000000000000000000, 0.8660254037844387076, 1.000000000000000000, 0.8660254037844387076, 1.000000000000000000, 0.8660254037844387076, 1.000000000000000000, 0.8660254037844387076, 1.000000000000000000, 0.8660254037844387076, 1.000000000000000000, 0.8660254037844387076, 1.000000000000000000, 0.8660254037844387076, 1.000000000000000000, 0.8660254037844387076, 1.000000000000000000, 0.8660254037844387076, 1.000000000000000000, 0.8660254037844387076, 1.000000000000000000, 0.8660254037844387076, 1.000000000000000000, 0.8660254037844387076, 1.000000000000000000, 0.8660254037844387076, 1.000000000000000000, 0.8660254037844387076, 1.000000000000000000, 0.8660254037844387076, 1.000000000000000000, 0.8660254037844387076, 1.000000000000000000, 0.8660254037844387076, 1.000000000000000000, 0.8660254037844387076, 1.000000000000000000, 0.8660254037844387076, 1.000000000000000000, 0.8660254037844387076, 1.000000000000000000, 0.8660254037844387076, 1.000000000000000000, 0.8660254037844387076, 1.000000000000000000, 0.8660254037844387076, 1.000000000000000000, 0.8660254037844387076, 1.000000000000000000, 0.8660254037844387076, 1.000000000000000000, 0.8660254037844387076, 1.000000000000000000, 0.8660254037844387076, 1.000000000000000000, 0.8660254037844387076, 1.000000000000000000, 0.8660254037844387076, 1.000000000000000000, 0.8660254037844387076, 1.000000000000000000),
 ( 1.000000000000000000, 0.8660254037844387076, 1.000000000000000000, 0.8660254037844387076, 1.000000000000000000, 0.8660254037844387076, 1.000000000000000000, 0.8660254037844387076, 1.000000000000000000, 0.8660254037844387076, 1.000000000000000000, 0.8660254037844387076, 1.000000000000000000, 0.8660254037844387076, 1.000000000000000000, 0.8660254037844387076, 1.000000000000000000, 0.8660254037844387076, 1.000000000000000000, 0.8660254037844387076, 1.000000000000000000, 0.8660254037844387076, 1.000000000000000000, 0.8660254037844387076, 1.000000000000000000, 0.8660254037844387076, 1.000000000000000000, 0.8660254037844387076, 1.000000000000000000, 0.8660254037844387076, 1.000000000000000000, 0.8660254037844387076, 1.000000000000000000, 0.8660254037844387076, 1.000000000000000000, 0.8660254037844387076, 1.000000000000000000, 0.8660254037844387076, 1.000000000000000000, 0.8660254037844387076, 1.000000000000000000, 0.8660254037844387076, 1.000000000000000000, 0.8660254037844387076, 1.000000000000000000, 0.8660254037844387076, 1.000000000000000000, 0.8660254037844387076, 1.000000000000000000, 0.8660254037844387076, 1.000000000000000000, 0.8660254037844387076, 1.000000000000000000, 0.8660254037844387076, 1.000000000000000000, 0.8660254037844387076, 1.000000000000000000, 0.8660254037844387076, 1.000000000000000000, 0.8660254037844387076, 1.000000000000000000, 0.8660254037844387076, 1.000000000000000000, 0.8660254037844387076, 1.000000000000000000, 0.8660254037844387076, 1.000000000000000000, 0.8660254037844387076, 1.000000000000000000, 0.8660254037844387076, 1.000000000000000000, 0.8660254037844387076, 1.000000000000000000, 0.8660254037844387076, 1.000000000000000000, 0.8660254037844387076, 1.000000000000000000, 0.8660254037844387076, 1.000000000000000000, 0.8660254037844387076, 1.000000000000000000, 0.8660254037844387076, 1.000000000000000000, 0.8660254037844387076, 1.000000000000000000) ) ) 
 REPRESENTATION_ITEM ( '' )  SURFACE ( )  );
#110954 = EDGE_LOOP ( 'NONE', ( #100008, #46485, #14040, #38988 ) ) ;
#110955 = ORIENTED_EDGE ( 'NONE', *, *, #46420, .T. ) ;
#110957 = EDGE_CURVE ( 'NONE', #3765, #109502, #50864, .T. ) ;
#110956 = AXIS2_PLACEMENT_3D ( 'NONE', #102032, #41837, #63394 ) ;
#110958 = PLANE ( 'NONE',  #54796 ) ;
#110959 = AXIS2_PLACEMENT_3D ( 'NONE', #21387, #101243, #124098 ) ;
#110960 = DIRECTION ( 'NONE',  ( 0.000000000000000000, 1.000000000000000000, 0.000000000000000000 ) ) ;
#110961 = CARTESIAN_POINT ( 'NONE',  ( -3.100000000000028511, 2.500000000000000000, -3.883716857408426648 ) ) ;
#110962 = CARTESIAN_POINT ( 'NONE',  ( 6.649999999999931966, 12.50000000000000000, -7.122917578226816815 ) ) ;
#110963 = ORIENTED_EDGE ( 'NONE', *, *, #79658, .F. ) ;
#110964 = DIRECTION ( 'NONE',  ( 0.000000000000000000, 1.000000000000000000, 0.000000000000000000 ) ) ;
#110965 = AXIS2_PLACEMENT_3D ( 'NONE', #107843, #18167, #87548 ) ;
#110966 = ORIENTED_EDGE ( 'NONE', *, *, #39689, .T. ) ;
#110967 = CARTESIAN_POINT ( 'NONE',  ( 15.83209681635537258, -2.500000000000000000, 5.404881881984332281 ) ) ;
#110968 = ORIENTED_EDGE ( 'NONE', *, *, #101403, .F. ) ;
#110969 = CARTESIAN_POINT ( 'NONE',  ( 14.54999999999989591, 12.50000000000000000, 2.165063509461097713 ) ) ;
#110970 = CARTESIAN_POINT ( 'NONE',  ( 1.449999999999950440, 2.500000000000000000, 6.048780366869520364 ) ) ;
#110971 = AXIS2_PLACEMENT_3D ( 'NONE', #89357, #82774, #111568 ) ;
#110972 = DIRECTION ( 'NONE',  ( 0.000000000000000000, 0.000000000000000000, -1.000000000000000000 ) ) ;
#110973 = EDGE_CURVE ( 'NONE', #124496, #18418, #71796, .T. ) ;
#110974 = EDGE_CURVE ( 'NONE', #104656, #60686, #9760, .T. ) ;
#110975 = CARTESIAN_POINT ( 'NONE',  ( -4.600000000000024514, 2.500000000000000000, 0.6928203230275494784 ) ) ;
#110976 = EDGE_LOOP ( 'NONE', ( #25674, #111996, #2831, #21730 ) ) ;
#110977 = DIRECTION ( 'NONE',  ( 0.000000000000000000, 0.000000000000000000, -1.000000000000000000 ) ) ;
#110978 = DIRECTION ( 'NONE',  ( -4.274815082592931898E-19, -0.9999939076577903929, -0.003490651415223739937 ) ) ;
#110979 = EDGE_LOOP ( 'NONE', ( #67585, #99569, #81497, #101639 ) ) ;
#110980 = EDGE_LOOP ( 'NONE', ( #105834, #121746 ) ) ;
#110982 = ORIENTED_EDGE ( 'NONE', *, *, #54766, .T. ) ;
#110981 = EDGE_CURVE ( 'NONE', #94678, #28470, #30715, .T. ) ;
#110983 = CARTESIAN_POINT ( 'NONE',  ( 17.50000000000000000, -2.750000000000000444, 3.432456362931491700 ) ) ;
#110984 = DIRECTION ( 'NONE',  ( 0.000000000000000000, 0.000000000000000000, 1.000000000000000000 ) ) ;
#110985 = DIRECTION ( 'NONE',  ( 0.000000000000000000, -0.9999939076577903929, 0.003490651415223739937 ) ) ;
#110986 = DIRECTION ( 'NONE',  ( 0.000000000000000000, 1.000000000000000000, 0.000000000000000000 ) ) ;
#110987 = DIRECTION ( 'NONE',  ( -0.000000000000000000, 1.000000000000000000, -0.000000000000000000 ) ) ;
#110988 = FACE_OUTER_BOUND ( 'NONE', #104179, .T. ) ;
#110989 = DIRECTION ( 'NONE',  ( -0.000000000000000000, 1.000000000000000000, -0.000000000000000000 ) ) ;
#110990 = CARTESIAN_POINT ( 'NONE',  ( 7.099999999999926814, 2.500000000000000000, -0.7928203230275542301 ) ) ;
#110991 = CARTESIAN_POINT ( 'NONE',  ( 6.249999999999930722, 12.50000000000000000, -1.472243186433550122 ) ) ;
#110992 = CONICAL_SURFACE ( 'NONE', #96413, 0.09999999999999982514, 0.003490658503988666988 ) ;
#110993 = CONICAL_SURFACE ( 'NONE', #23265, 0.1000000000000000472, 0.003490658503988666988 ) ;
#110994 = CIRCLE ( 'NONE', #33743, 0.06509327318403741736 ) ;
#110995 = AXIS2_PLACEMENT_3D ( 'NONE', #37957, #7191, #37330 ) ;
#110996 = EDGE_LOOP ( 'NONE', ( #126667, #88167, #79018, #99554 ) ) ;
#110997 = FACE_OUTER_BOUND ( 'NONE', #49952, .T. ) ;
#110998 = CONICAL_SURFACE ( 'NONE', #21138, 0.09999999999999982514, 0.003490658503988666988 ) ;
#110999 = CARTESIAN_POINT ( 'NONE',  ( 13.14999999999989733, 2.500000000000000000, -1.818653347947325916 ) ) ;
#111000 = FACE_OUTER_BOUND ( 'NONE', #45320, .T. ) ;
#111001 = CARTESIAN_POINT ( 'NONE',  ( -12.29999999999999538, 12.50000000000000000, 4.676537180435972552 ) ) ;
#111002 = ORIENTED_EDGE ( 'NONE', *, *, #56793, .T. ) ;
#111003 = DIRECTION ( 'NONE',  ( 0.000000000000000000, 0.000000000000000000, -1.000000000000000000 ) ) ;
#111004 = ADVANCED_FACE ( 'NONE', ( #101247 ), #101897, .T. ) ;
#111005 = FACE_OUTER_BOUND ( 'NONE', #76411, .T. ) ;
#111007 = ORIENTED_EDGE ( 'NONE', *, *, #63503, .T. ) ;
#111006 = DIRECTION ( 'NONE',  ( 0.000000000000000000, -0.9999939076577903929, 0.003490651415223739937 ) ) ;
#111008 = EDGE_CURVE ( 'NONE', #100170, #36170, #110107, .T. ) ;
#111009 = EDGE_CURVE ( 'NONE', #81664, #89399, #12209, .T. ) ;
#111010 = ORIENTED_EDGE ( 'NONE', *, *, #17607, .F. ) ;
#111011 = DIRECTION ( 'NONE',  ( 0.000000000000000000, 1.000000000000000000, 0.000000000000000000 ) ) ;
#111012 = ORIENTED_EDGE ( 'NONE', *, *, #93307, .T. ) ;
#111013 = ORIENTED_EDGE ( 'NONE', *, *, #58258, .T. ) ;
#111014 = PLANE ( 'NONE',  #99151 ) ;
#111015 = EDGE_CURVE ( 'NONE', #126895, #121003, #68239, .T. ) ;
#111016 = EDGE_CURVE ( 'NONE', #47134, #935, #127187, .T. ) ;
#111017 = ADVANCED_FACE ( 'NONE', ( #58443 ), #24429, .T. ) ;
#111018 = CARTESIAN_POINT ( 'NONE',  ( -6.050000000000018474, 2.500000000000000000, 6.841600689897072485 ) ) ;
#111019 = CARTESIAN_POINT ( 'NONE',  ( 4.799999999999934097, 2.500000000000000000, 4.776537180435972196 ) ) ;
#111020 = CARTESIAN_POINT ( 'NONE',  ( 6.449999999999931788, 12.50000000000000000, -2.511473670974877948 ) ) ;
#111021 = CIRCLE ( 'NONE', #23211, 0.06509327318403745899 ) ;
#111022 = ORIENTED_EDGE ( 'NONE', *, *, #32466, .F. ) ;
#111023 = CONICAL_SURFACE ( 'NONE', #127773, 0.1000000000000000472, 0.003490658503988666988 ) ;
#111024 = EDGE_CURVE ( 'NONE', #19044, #71330, #107529, .T. ) ;
#111025 = DIRECTION ( 'NONE',  ( 0.000000000000000000, 1.000000000000000000, 0.000000000000000000 ) ) ;
#111026 = ORIENTED_EDGE ( 'NONE', *, *, #104227, .T. ) ;
#111027 = DIRECTION ( 'NONE',  ( -0.000000000000000000, 1.000000000000000000, -0.000000000000000000 ) ) ;
#111028 = ADVANCED_FACE ( 'NONE', ( #36223 ), #11810, .T. ) ;
#111029 = FACE_OUTER_BOUND ( 'NONE', #52867, .T. ) ;
#111030 = ADVANCED_FACE ( 'NONE', ( #78066 ), #17851, .T. ) ;
#111031 = ORIENTED_EDGE ( 'NONE', *, *, #70838, .T. ) ;
#111032 = CIRCLE ( 'NONE', #14879, 0.06509327318403745899 ) ;
#111033 = ORIENTED_EDGE ( 'NONE', *, *, #73767, .T. ) ;
#111034 = ORIENTED_EDGE ( 'NONE', *, *, #41304, .F. ) ;
#111035 = EDGE_LOOP ( 'NONE', ( #54427, #110303, #41315, #82687 ) ) ;
#111036 = PLANE ( 'NONE',  #110959 ) ;
#111037 = CARTESIAN_POINT ( 'NONE',  ( 7.180215335589515746, 2.500000000000001332, 8.697219394723591179 ) ) ;
#111038 = DIRECTION ( 'NONE',  ( 0.000000000000000000, -0.000000000000000000, 1.000000000000000000 ) ) ;
#111039 = FACE_BOUND ( 'NONE', #18631, .T. ) ;
#111040 = DIRECTION ( 'NONE',  ( 0.000000000000000000, 1.000000000000000000, 0.000000000000000000 ) ) ;
#111041 = CARTESIAN_POINT ( 'NONE',  ( 187.1927083336747160, 6.551208109652275624, -3.782341765624998686 ) ) ;
#111042 = PLANE ( 'NONE',  #9233 ) ;
#111043 = DIRECTION ( 'NONE',  ( 0.000000000000000000, -0.9999939076577903929, 0.003490651415223739937 ) ) ;
#111044 = AXIS2_PLACEMENT_3D ( 'NONE', #3034, #70475, #31214 ) ;
#111045 = AXIS2_PLACEMENT_3D ( 'NONE', #40910, #80815, #31082 ) ;
#111046 = CIRCLE ( 'NONE', #96478, 0.06509327318403745899 ) ;
#111047 = DIRECTION ( 'NONE',  ( 0.000000000000000000, -0.000000000000000000, 1.000000000000000000 ) ) ;
#111048 = DIRECTION ( 'NONE',  ( -0.000000000000000000, 1.000000000000000000, -0.000000000000000000 ) ) ;
#111049 = DIRECTION ( 'NONE',  ( 0.000000000000000000, -0.9999939076577903929, 0.003490651415223739937 ) ) ;
#111050 = VECTOR ( 'NONE', #112997, 1000.000000000000000 ) ;
#111051 = CARTESIAN_POINT ( 'NONE',  ( -10.60000000000000320, 2.500000000000000000, -3.883716857408422207 ) ) ;
#111052 = ORIENTED_EDGE ( 'NONE', *, *, #9835, .F. ) ;
#111053 = AXIS2_PLACEMENT_3D ( 'NONE', #85952, #124615, #104946 ) ;
#111054 = AXIS2_PLACEMENT_3D ( 'NONE', #77021, #107771, #18094 ) ;
#111055 = ORIENTED_EDGE ( 'NONE', *, *, #56009, .F. ) ;
#111056 = VERTEX_POINT ( 'NONE', #46677 ) ;
#111057 = ORIENTED_EDGE ( 'NONE', *, *, #102843, .T. ) ;
#111058 = VERTEX_POINT ( 'NONE', #76137 ) ;
#111059 = FACE_OUTER_BOUND ( 'NONE', #77213, .T. ) ;
#111060 = CARTESIAN_POINT ( 'NONE',  ( 2.899999999999945732, 2.500000000000000000, -4.230127018922201998 ) ) ;
#111061 = ORIENTED_EDGE ( 'NONE', *, *, #65381, .T. ) ;
#111062 = FACE_BOUND ( 'NONE', #120636, .T. ) ;
#111063 = DIRECTION ( 'NONE',  ( 0.000000000000000000, 0.000000000000000000, -1.000000000000000000 ) ) ;
#111064 = EDGE_CURVE ( 'NONE', #34594, #93338, #1345, .T. ) ;
#111065 = ADVANCED_FACE ( 'NONE', ( #96402 ), #3503, .T. ) ;
#111066 = ORIENTED_EDGE ( 'NONE', *, *, #48262, .T. ) ;
#111067 = DIRECTION ( 'NONE',  ( -4.274815082592931898E-19, -0.9999939076577903929, -0.003490651415223739937 ) ) ;
#111068 = CARTESIAN_POINT ( 'NONE',  ( 4.999999999999938716, 12.50000000000000000, -5.088040615133791356 ) ) ;
#111069 = CARTESIAN_POINT ( 'NONE',  ( 9.399999999999915090, 2.500000000000000000, -4.083716857408426826 ) ) ;
#111070 = CARTESIAN_POINT ( 'NONE',  ( -11.84999999999999609, 12.50000000000000000, 6.841600689897072485 ) ) ;
#111071 = EDGE_LOOP ( 'NONE', ( #127720, #27001 ) ) ;
#111072 = LINE ( 'NONE', #21425, #82665 ) ;
#111073 = VERTEX_POINT ( 'NONE', #57134 ) ;
#111074 = AXIS2_PLACEMENT_3D ( 'NONE', #83710, #73240, #34624 ) ;
#111075 = ORIENTED_EDGE ( 'NONE', *, *, #103771, .T. ) ;
#111076 = CIRCLE ( 'NONE', #54653, 0.1000000000000000472 ) ;
#111077 = DIRECTION ( 'NONE',  ( 0.000000000000000000, 1.000000000000000000, 0.000000000000000000 ) ) ;
#111078 = AXIS2_PLACEMENT_3D ( 'NONE', #117240, #117907, #67501 ) ;
#111079 = CARTESIAN_POINT ( 'NONE',  ( 185.0312500006828031, 9.429780353434619030E-16, -7.700000000000000178 ) ) ;
#111080 = ORIENTED_EDGE ( 'NONE', *, *, #64808, .T. ) ;
#111081 = DIRECTION ( 'NONE',  ( 0.000000000000000000, 0.000000000000000000, 1.000000000000000000 ) ) ;
#111082 = DIRECTION ( 'NONE',  ( 0.000000000000000000, 0.000000000000000000, 1.000000000000000000 ) ) ;
#111083 = VECTOR ( 'NONE', #83054, 1000.000000000000000 ) ;
#111085 = CONICAL_SURFACE ( 'NONE', #115189, 0.1000000000000002554, 0.003490658503988666988 ) ;
#111084 = PLANE ( 'NONE',  #49908 ) ;
#111086 = CARTESIAN_POINT ( 'NONE',  ( 9.799999999999915445, 2.500000000000000000, 3.983716857408420964 ) ) ;
#111087 = PLANE ( 'NONE',  #91481 ) ;
#111088 = EDGE_LOOP ( 'NONE', ( #42759, #41569, #48766, #265 ) ) ;
#111089 = VECTOR ( 'NONE', #17922, 1000.000000000000000 ) ;
#111090 = CARTESIAN_POINT ( 'NONE',  ( 7.499999999999960032, 12.50000000000000000, -0.06509327318403970719 ) ) ;
#111091 = ORIENTED_EDGE ( 'NONE', *, *, #2111, .T. ) ;
#111092 = DIRECTION ( 'NONE',  ( 0.000000000000000000, 0.000000000000000000, 1.000000000000000000 ) ) ;
#111093 = ORIENTED_EDGE ( 'NONE', *, *, #100951, .F. ) ;
#111094 = CARTESIAN_POINT ( 'NONE',  ( -6.249999999999981348, 2.500000000000000000, 6.495190528383297135 ) ) ;
#111095 = ORIENTED_EDGE ( 'NONE', *, *, #49969, .T. ) ;
#111096 = DIRECTION ( 'NONE',  ( 0.000000000000000000, 0.000000000000000000, -1.000000000000000000 ) ) ;
#111097 = CARTESIAN_POINT ( 'NONE',  ( -14.99999999999998401, 2.500000000000000000, 0.7928203230275517877 ) ) ;
#111098 = FACE_OUTER_BOUND ( 'NONE', #4293, .T. ) ;
#111099 = CARTESIAN_POINT ( 'NONE',  ( -14.14999999999998792, 2.500000000000000000, 2.957883832488652942 ) ) ;
#111100 = CARTESIAN_POINT ( 'NONE',  ( 17.17279024593002745, 1.352253750625354245, -5.266180533623050053 ) ) ;
#111101 = ORIENTED_EDGE ( 'NONE', *, *, #36034, .T. ) ;
#111102 = EDGE_LOOP ( 'NONE', ( #23761, #41092 ) ) ;
#111104 = VERTEX_POINT ( 'NONE', #57792 ) ;
#111103 = EDGE_CURVE ( 'NONE', #86078, #90873, #128477, .T. ) ;
#111105 = CARTESIAN_POINT ( 'NONE',  ( 127.5000000000000000, 5.000000000000000000, 2.000000000000001776 ) ) ;
#111106 = DIRECTION ( 'NONE',  ( 0.000000000000000000, 0.000000000000000000, -1.000000000000000000 ) ) ;
#111107 = PLANE ( 'NONE',  #121194 ) ;
#111109 = ORIENTED_EDGE ( 'NONE', *, *, #76254, .F. ) ;
#111108 = ORIENTED_EDGE ( 'NONE', *, *, #104320, .T. ) ;
#111110 = ORIENTED_EDGE ( 'NONE', *, *, #816, .F. ) ;
#111111 = CARTESIAN_POINT ( 'NONE',  ( 184.7812500006828031, 0.000000000000000000, 7.700000000000000178 ) ) ;
#111113 = EDGE_LOOP ( 'NONE', ( #81358, #67636 ) ) ;
#111112 = CIRCLE ( 'NONE', #54677, 0.06509327318403745899 ) ;
#111115 = EDGE_CURVE ( 'NONE', #86595, #93018, #84968, .T. ) ;
#111114 = DIRECTION ( 'NONE',  ( 0.000000000000000000, -0.000000000000000000, 1.000000000000000000 ) ) ;
#111116 = PLANE ( 'NONE',  #76970 ) ;
#111117 = AXIS2_PLACEMENT_3D ( 'NONE', #42106, #2817, #51298 ) ;
#111118 = CARTESIAN_POINT ( 'NONE',  ( -1.050000000000038680, 2.500000000000000000, 6.841600689897072485 ) ) ;
#111119 = DIRECTION ( 'NONE',  ( -0.000000000000000000, 1.000000000000000000, -0.000000000000000000 ) ) ;
#111120 = DIRECTION ( 'NONE',  ( -0.000000000000000000, -1.000000000000000000, -0.000000000000000000 ) ) ;
#111121 = CARTESIAN_POINT ( 'NONE',  ( 14.34999999999989662, 12.50000000000000000, 1.818653347947321475 ) ) ;
#111122 = DIRECTION ( 'NONE',  ( 0.000000000000000000, -0.000000000000000000, 1.000000000000000000 ) ) ;
#111123 = EDGE_CURVE ( 'NONE', #115958, #3256, #34826, .T. ) ;
#111124 = EDGE_CURVE ( 'NONE', #37067, #39039, #76660, .T. ) ;
#111126 = AXIS2_PLACEMENT_3D ( 'NONE', #79814, #128944, #108625 ) ;
#111125 = FACE_OUTER_BOUND ( 'NONE', #94934, .T. ) ;
#111127 = EDGE_LOOP ( 'NONE', ( #102544, #111688, #97644, #6623 ) ) ;
#111128 = AXIS2_PLACEMENT_3D ( 'NONE', #77825, #98114, #119683 ) ;
#111129 = TOROIDAL_SURFACE ( 'NONE', #44538, 9.000000000000001776, 1.000000000000000000 ) ;
#111130 = LINE ( 'NONE', #21485, #101055 ) ;
#111131 = AXIS2_PLACEMENT_3D ( 'NONE', #6344, #46291, #116315 ) ;
#111132 = EDGE_CURVE ( 'NONE', #57912, #40952, #62004, .T. ) ;
#111133 = DIRECTION ( 'NONE',  ( 0.000000000000000000, 0.000000000000000000, -1.000000000000000000 ) ) ;
#111134 = ORIENTED_EDGE ( 'NONE', *, *, #74976, .F. ) ;
#111135 = ORIENTED_EDGE ( 'NONE', *, *, #6706, .F. ) ;
#111136 = ADVANCED_FACE ( 'NONE', ( #66306 ), #95444, .T. ) ;
#111137 = CARTESIAN_POINT ( 'NONE',  ( 184.9010416670080588, -4.367472073101519747, 7.564683531249999149 ) ) ;
#111138 = DIRECTION ( 'NONE',  ( 0.000000000000000000, 1.000000000000000000, 0.000000000000000000 ) ) ;
#111139 = DIRECTION ( 'NONE',  ( 0.000000000000000000, 0.000000000000000000, -1.000000000000000000 ) ) ;
#111140 = CONICAL_SURFACE ( 'NONE', #98614, 0.1000000000000002554, 0.003490658503988666988 ) ;
#111141 = DIRECTION ( 'NONE',  ( 0.000000000000000000, 1.000000000000000000, 0.000000000000000000 ) ) ;
#111142 = DIRECTION ( 'NONE',  ( 0.000000000000000000, 0.000000000000000000, 1.000000000000000000 ) ) ;
#111143 = CARTESIAN_POINT ( 'NONE',  ( 8.949999999999915801, 12.50000000000000000, -1.883746621131363597 ) ) ;
#111144 = FACE_OUTER_BOUND ( 'NONE', #114660, .T. ) ;
#111145 = VECTOR ( 'NONE', #95056, 1000.000000000000000 ) ;
#111146 = CARTESIAN_POINT ( 'NONE',  ( -1.700000000000034817, 12.50000000000000000, -4.330127018922201643 ) ) ;
#111147 = AXIS2_PLACEMENT_3D ( 'NONE', #65866, #3096, #14803 ) ;
#111148 = VECTOR ( 'NONE', #37020, 1000.000000000000000 ) ;
#111149 = DIRECTION ( 'NONE',  ( 0.000000000000000000, -0.000000000000000000, 1.000000000000000000 ) ) ;
#111150 = ORIENTED_EDGE ( 'NONE', *, *, #62068, .F. ) ;
#111151 = ORIENTED_EDGE ( 'NONE', *, *, #117794, .F. ) ;
#111152 = CONICAL_SURFACE ( 'NONE', #21285, 0.1000000000000000472, 0.003490658503988666988 ) ;
#111153 = ORIENTED_EDGE ( 'NONE', *, *, #76617, .T. ) ;
#111154 = ORIENTED_EDGE ( 'NONE', *, *, #102812, .F. ) ;
#111155 = DIRECTION ( 'NONE',  ( 0.000000000000000000, -0.9999939076577903929, 0.003490651415223739937 ) ) ;
#111156 = FACE_OUTER_BOUND ( 'NONE', #63051, .T. ) ;
#111157 = ORIENTED_EDGE ( 'NONE', *, *, #91573, .T. ) ;
#111158 = DIRECTION ( 'NONE',  ( 0.000000000000000000, 0.000000000000000000, -1.000000000000000000 ) ) ;
#111159 = EDGE_CURVE ( 'NONE', #110110, #127840, #13953, .T. ) ;
#111160 = DIRECTION ( 'NONE',  ( -0.000000000000000000, 1.000000000000000000, -0.000000000000000000 ) ) ;
#111161 = FACE_OUTER_BOUND ( 'NONE', #23381, .T. ) ;
#111163 = VERTEX_POINT ( 'NONE', #56478 ) ;
#111162 = CARTESIAN_POINT ( 'NONE',  ( 7.699999999999923794, 2.500000000000000000, -0.3464101615137783474 ) ) ;
#111164 = EDGE_CURVE ( 'NONE', #119116, #66538, #72463, .T. ) ;
#111165 = DIRECTION ( 'NONE',  ( -0.000000000000000000, -1.000000000000000000, -0.000000000000000000 ) ) ;
#111166 = ADVANCED_FACE ( 'NONE', ( #15908 ), #6083, .T. ) ;
#111167 = DIRECTION ( 'NONE',  ( 0.000000000000000000, 0.000000000000000000, 1.000000000000000000 ) ) ;
#111168 = ORIENTED_EDGE ( 'NONE', *, *, #1340, .F. ) ;
#111169 = EDGE_LOOP ( 'NONE', ( #117333, #59069, #34429, #105287 ) ) ;
#111170 = VERTEX_POINT ( 'NONE', #17180 ) ;
#111171 = AXIS2_PLACEMENT_3D ( 'NONE', #43798, #4463, #55539 ) ;
#111172 = VERTEX_POINT ( 'NONE', #97063 ) ;
#111173 = CARTESIAN_POINT ( 'NONE',  ( 6.649999999999930189, 2.500000000000000000, 5.802370205355744659 ) ) ;
#111174 = AXIS2_PLACEMENT_3D ( 'NONE', #22652, #63204, #12791 ) ;
#111175 = ADVANCED_FACE ( 'NONE', ( #47327 ), #76755, .T. ) ;
#111176 = AXIS2_PLACEMENT_3D ( 'NONE', #32138, #39390, #21000 ) ;
#111177 = EDGE_CURVE ( 'NONE', #23570, #44909, #82748, .T. ) ;
#111178 = EDGE_CURVE ( 'NONE', #94583, #45538, #106000, .T. ) ;
#111179 = EDGE_CURVE ( 'NONE', #102327, #65030, #72562, .T. ) ;
#111180 = CARTESIAN_POINT ( 'NONE',  ( -8.100000000000010303, 2.500000000000000000, 4.676537180435972552 ) ) ;
#111181 = DIRECTION ( 'NONE',  ( 0.000000000000000000, 0.000000000000000000, 1.000000000000000000 ) ) ;
#111183 = VERTEX_POINT ( 'NONE', #61663 ) ;
#111182 = AXIS2_PLACEMENT_3D ( 'NONE', #23153, #122649, #102996 ) ;
#111184 = CIRCLE ( 'NONE', #113338, 0.1000000000000002554 ) ;
#111185 = CIRCLE ( 'NONE', #38052, 0.09999999999999982514 ) ;
#111186 = EDGE_CURVE ( 'NONE', #51434, #120113, #49576, .T. ) ;
#111187 = LINE ( 'NONE', #30738, #20990 ) ;
#111188 = VERTEX_POINT ( 'NONE', #101578 ) ;
#111189 = LINE ( 'NONE', #28791, #116396 ) ;
#111190 = DIRECTION ( 'NONE',  ( -4.274815082592931898E-19, -0.9999939076577903929, -0.003490651415223739937 ) ) ;
#111191 = CIRCLE ( 'NONE', #50557, 0.1000000000000002554 ) ;
#111192 = CARTESIAN_POINT ( 'NONE',  ( 10.84999999999991260, 2.500000000000000000, 7.288010851410849256 ) ) ;
#111193 = PLANE ( 'NONE',  #40054 ) ;
#111194 = EDGE_CURVE ( 'NONE', #68417, #115797, #68341, .T. ) ;
#111195 = VECTOR ( 'NONE', #87410, 1000.000000000000000 ) ;
#111196 = ORIENTED_EDGE ( 'NONE', *, *, #82750, .T. ) ;
#111197 = EDGE_CURVE ( 'NONE', #112193, #47787, #49272, .T. ) ;
#111198 = ORIENTED_EDGE ( 'NONE', *, *, #18761, .T. ) ;
#111199 = ORIENTED_EDGE ( 'NONE', *, *, #35223, .T. ) ;
#111200 = DIRECTION ( 'NONE',  ( -0.000000000000000000, -1.000000000000000000, -0.000000000000000000 ) ) ;
#111201 = DIRECTION ( 'NONE',  ( 0.000000000000000000, 1.000000000000000000, 0.000000000000000000 ) ) ;
#111202 = FACE_BOUND ( 'NONE', #117749, .T. ) ;
#111203 = DIRECTION ( 'NONE',  ( 0.000000000000000000, -0.000000000000000000, 1.000000000000000000 ) ) ;
#111204 = DIRECTION ( 'NONE',  ( 0.000000000000000000, -0.9999939076577903929, 0.003490651415223739937 ) ) ;
#111205 = PLANE ( 'NONE',  #129465 ) ;
#111206 = CARTESIAN_POINT ( 'NONE',  ( 0.5999999999999621192, 12.50000000000000000, 0.3464101615137758494 ) ) ;
#111207 = FACE_OUTER_BOUND ( 'NONE', #125047, .T. ) ;
#111208 = CARTESIAN_POINT ( 'NONE',  ( 129.5000000000000000, -1.375000000000000000, 7.634788798650553154 ) ) ;
#111209 = ORIENTED_EDGE ( 'NONE', *, *, #100783, .F. ) ;
#111210 = CONICAL_SURFACE ( 'NONE', #125790, 0.1000000000000002554, 0.003490658503988666988 ) ;
#111211 = CARTESIAN_POINT ( 'NONE',  ( 8.949999999999917577, 12.50000000000000000, -2.511473670974877948 ) ) ;
#111212 = DIRECTION ( 'NONE',  ( 0.000000000000000000, 1.000000000000000000, 0.000000000000000000 ) ) ;
#111213 = ORIENTED_EDGE ( 'NONE', *, *, #73201, .F. ) ;
#111214 = ORIENTED_EDGE ( 'NONE', *, *, #51381, .F. ) ;
#111215 = CARTESIAN_POINT ( 'NONE',  ( 9.599999999999914380, 2.500000000000000000, 4.330127018922196314 ) ) ;
#111216 = CARTESIAN_POINT ( 'NONE',  ( 5.849999999999934808, 12.50000000000000000, -5.802370205355749988 ) ) ;
#111217 = FACE_BOUND ( 'NONE', #126349, .T. ) ;
#111218 = AXIS2_PLACEMENT_3D ( 'NONE', #106539, #75786, #56772 ) ;
#111219 = DIRECTION ( 'NONE',  ( -0.000000000000000000, -1.000000000000000000, -0.000000000000000000 ) ) ;
#111220 = AXIS2_PLACEMENT_3D ( 'NONE', #77372, #117256, #67519 ) ;
#111221 = AXIS2_PLACEMENT_3D ( 'NONE', #35058, #82863, #22654 ) ;
#111222 = ADVANCED_FACE ( 'NONE', ( #133 ), #16086, .T. ) ;
#111223 = ORIENTED_EDGE ( 'NONE', *, *, #104214, .F. ) ;
#111224 = CARTESIAN_POINT ( 'NONE',  ( -10.00000000000000711, 2.500000000000000000, -3.537306695894645969 ) ) ;
#111225 = CARTESIAN_POINT ( 'NONE',  ( 184.3750000000000000, 8.891194145520236347, 5.444286225454521982E-16 ) ) ;
#111226 = ORIENTED_EDGE ( 'NONE', *, *, #60280, .F. ) ;
#111228 = CARTESIAN_POINT ( 'NONE',  ( 11.89999999999990443, 2.500000000000000000, 0.4464101615137736623 ) ) ;
#111227 = AXIS2_PLACEMENT_3D ( 'NONE', #104750, #6530, #47801 ) ;
#111229 = DIRECTION ( 'NONE',  ( 0.000000000000000000, -0.000000000000000000, 1.000000000000000000 ) ) ;
#111230 = VECTOR ( 'NONE', #45243, 1000.000000000000000 ) ;
#111231 = ADVANCED_FACE ( 'NONE', ( #119273 ), #108042, .T. ) ;
#111232 = VECTOR ( 'NONE', #113898, 1000.000000000000000 ) ;
#111233 = CONICAL_SURFACE ( 'NONE', #50617, 0.1000000000000002554, 0.003490658503988666988 ) ;
#111234 = CARTESIAN_POINT ( 'NONE',  ( 0.7999999999999612976, 12.50000000000000000, -1.084202172485504434E-16 ) ) ;
#111235 = CARTESIAN_POINT ( 'NONE',  ( 107.5000000000000142, 2.449293598294706414E-16, 2.000000000000000000 ) ) ;
#111236 = AXIS2_PLACEMENT_3D ( 'NONE', #30125, #54709, #60854 ) ;
#111237 = EDGE_LOOP ( 'NONE', ( #8982, #94172, #77515, #100829 ) ) ;
#111238 = CARTESIAN_POINT ( 'NONE',  ( 2.499999999999948930, 12.50000000000000000, -0.6928203230275541413 ) ) ;
#111239 = DIRECTION ( 'NONE',  ( 0.000000000000000000, 0.000000000000000000, -1.000000000000000000 ) ) ;
#111240 = FACE_OUTER_BOUND ( 'NONE', #75137, .T. ) ;
#111241 = ORIENTED_EDGE ( 'NONE', *, *, #98643, .F. ) ;
#111242 = ORIENTED_EDGE ( 'NONE', *, *, #108108, .F. ) ;
#111243 = PLANE ( 'NONE',  #55540 ) ;
#111244 = ORIENTED_EDGE ( 'NONE', *, *, #17652, .F. ) ;
#111245 = DIRECTION ( 'NONE',  ( -0.000000000000000000, -1.000000000000000000, -0.000000000000000000 ) ) ;
#111246 = DIRECTION ( 'NONE',  ( 0.000000000000000000, 1.000000000000000000, 0.000000000000000000 ) ) ;
#111247 = LINE ( 'NONE', #14816, #21643 ) ;
#111248 = ORIENTED_EDGE ( 'NONE', *, *, #80313, .T. ) ;
#111249 = CARTESIAN_POINT ( 'NONE',  ( 5.399999999999931966, 12.50000000000000000, 4.395220292106234439 ) ) ;
#111250 = DIRECTION ( 'NONE',  ( 0.000000000000000000, -0.9999939076577903929, 0.003490651415223739937 ) ) ;
#111251 = DIRECTION ( 'NONE',  ( -0.000000000000000000, -1.000000000000000000, -0.000000000000000000 ) ) ;
#111252 = FACE_OUTER_BOUND ( 'NONE', #66067, .T. ) ;
#111253 = LINE ( 'NONE', #82482, #61179 ) ;
#111254 = DIRECTION ( 'NONE',  ( 0.000000000000000000, 1.000000000000000000, 0.000000000000000000 ) ) ;
#111255 = ORIENTED_EDGE ( 'NONE', *, *, #91670, .T. ) ;
#111256 = VERTEX_POINT ( 'NONE', #10591 ) ;
#111257 = CARTESIAN_POINT ( 'NONE',  ( 0.5999999999999621192, 2.500000000000000000, 0.4464101615137758272 ) ) ;
#111258 = ORIENTED_EDGE ( 'NONE', *, *, #123193, .F. ) ;
#111259 = VECTOR ( 'NONE', #29945, 1000.000000000000000 ) ;
#111260 = DIRECTION ( 'NONE',  ( 0.000000000000000000, 1.000000000000000000, 0.000000000000000000 ) ) ;
#111261 = AXIS2_PLACEMENT_3D ( 'NONE', #8007, #127161, #7357 ) ;
#111262 = CIRCLE ( 'NONE', #98661, 0.06509327318403745899 ) ;
#111264 = VERTEX_POINT ( 'NONE', #70187 ) ;
#111263 = ORIENTED_EDGE ( 'NONE', *, *, #66266, .T. ) ;
#111265 = VERTEX_POINT ( 'NONE', #19797 ) ;
#111266 = CARTESIAN_POINT ( 'NONE',  ( 2.699999999999945555, 12.50000000000000000, 4.048810130592458201 ) ) ;
#111268 = ADVANCED_FACE ( 'NONE', ( #59745 ), #15817, .T. ) ;
#111267 = CARTESIAN_POINT ( 'NONE',  ( 1.249999999999952038, 2.500000000000000000, 5.902370205355745192 ) ) ;
#111269 = AXIS2_PLACEMENT_3D ( 'NONE', #125631, #83160, #85712 ) ;
#111271 = DIRECTION ( 'NONE',  ( 0.000000000000000000, 1.000000000000000000, 0.000000000000000000 ) ) ;
#111270 = AXIS2_PLACEMENT_3D ( 'NONE', #83030, #103306, #22824 ) ;
#111272 = AXIS2_PLACEMENT_3D ( 'NONE', #1975, #63491, #111953 ) ;
#111273 = PRESENTATION_STYLE_ASSIGNMENT (( #81205 ) ) ;
#111274 = CARTESIAN_POINT ( 'NONE',  ( -1.250000000000001110, 2.500000000000000000, -2.165063509461101710 ) ) ;
#111275 = DIRECTION ( 'NONE',  ( 0.000000000000000000, -0.9999939076577903929, 0.003490651415223739937 ) ) ;
#111276 = CARTESIAN_POINT ( 'NONE',  ( 13.09999999999989839, 2.500000000000000000, -0.2464101615137783419 ) ) ;
#111277 = AXIS2_PLACEMENT_3D ( 'NONE', #60439, #61050, #111430 ) ;
#111278 = DIRECTION ( 'NONE',  ( 0.000000000000000000, 1.000000000000000000, 0.000000000000000000 ) ) ;
#111279 = FACE_OUTER_BOUND ( 'NONE', #61004, .T. ) ;
#111280 = ADVANCED_FACE ( 'NONE', ( #80657 ), #9849, .T. ) ;
#111281 = EDGE_CURVE ( 'NONE', #46427, #9874, #11247, .T. ) ;
#111282 = DIRECTION ( 'NONE',  ( -4.274815082592931898E-19, -0.9999939076577903929, -0.003490651415223739937 ) ) ;
#111283 = AXIS2_PLACEMENT_3D ( 'NONE', #41807, #33893, #83012 ) ;
#111284 = ORIENTED_EDGE ( 'NONE', *, *, #91078, .F. ) ;
#111285 = ADVANCED_FACE ( 'NONE', ( #100291, #1430 ), #91752, .T. ) ;
#111286 = CARTESIAN_POINT ( 'NONE',  ( 4.349999999999939249, 2.500000000000000000, 2.411473670974873862 ) ) ;
#111287 = EDGE_LOOP ( 'NONE', ( #14589, #17477, #104831, #28085 ) ) ;
#111288 = ORIENTED_EDGE ( 'NONE', *, *, #87493, .T. ) ;
#111289 = EDGE_CURVE ( 'NONE', #73490, #93190, #88990, .T. ) ;
#111290 = DIRECTION ( 'NONE',  ( 0.000000000000000000, 1.000000000000000000, 0.000000000000000000 ) ) ;
#111291 = CARTESIAN_POINT ( 'NONE',  ( -10.20000000000000462, 12.50000000000000000, -4.741630453620010677 ) ) ;
#111292 = AXIS2_PLACEMENT_3D ( 'NONE', #111018, #71116, #110391 ) ;
#111293 = DIRECTION ( 'NONE',  ( -0.000000000000000000, -1.000000000000000000, -0.000000000000000000 ) ) ;
#111294 = DIRECTION ( 'NONE',  ( 0.000000000000000000, 0.000000000000000000, 1.000000000000000000 ) ) ;
#111295 = CARTESIAN_POINT ( 'NONE',  ( -2.300000000000032685, 12.50000000000000000, -4.676537180435978769 ) ) ;
#111296 = CARTESIAN_POINT ( 'NONE',  ( 6.899999999999928413, 2.500000000000000000, -4.576537180435977348 ) ) ;
#111297 = ORIENTED_EDGE ( 'NONE', *, *, #32744, .T. ) ;
#111298 = CONICAL_SURFACE ( 'NONE', #54878, 0.1000000000000002554, 0.003490658503988666988 ) ;
#111299 = VERTEX_POINT ( 'NONE', #49918 ) ;
#111300 = CIRCLE ( 'NONE', #8906, 0.06509327318403745899 ) ;
#111301 = ORIENTED_EDGE ( 'NONE', *, *, #11035, .F. ) ;
#111302 = CARTESIAN_POINT ( 'NONE',  ( 5.849999999999932143, 2.500000000000000000, 1.472243186433545459 ) ) ;
#111303 = ORIENTED_EDGE ( 'NONE', *, *, #70974, .F. ) ;
#111304 = VERTEX_POINT ( 'NONE', #50529 ) ;
#111305 = AXIS2_PLACEMENT_3D ( 'NONE', #57295, #8177, #38305 ) ;
#111306 = CARTESIAN_POINT ( 'NONE',  ( 13.94999999999989271, 2.500000000000000000, -1.718653347947326049 ) ) ;
#111307 = DIRECTION ( 'NONE',  ( 0.000000000000000000, 0.000000000000000000, 1.000000000000000000 ) ) ;
#111308 = AXIS2_PLACEMENT_3D ( 'NONE', #127257, #106314, #98409 ) ;
#111309 = CIRCLE ( 'NONE', #77870, 0.1000000000000000056 ) ;
#111310 = DIRECTION ( 'NONE',  ( 0.000000000000000000, 0.000000000000000000, 1.000000000000000000 ) ) ;
#111311 = VECTOR ( 'NONE', #10088, 1000.000000000000000 ) ;
#111312 = CARTESIAN_POINT ( 'NONE',  ( 185.2812500006828031, 0.000000000000000000, 7.700000000000000178 ) ) ;
#111313 = DIRECTION ( 'NONE',  ( 0.000000000000000000, 1.000000000000000000, 0.000000000000000000 ) ) ;
#111314 = EDGE_LOOP ( 'NONE', ( #128072, #122407, #68827, #56968 ) ) ;
#111315 = DIRECTION ( 'NONE',  ( -0.000000000000000000, -1.000000000000000000, -0.000000000000000000 ) ) ;
#111316 = DIRECTION ( 'NONE',  ( -4.274815082592931898E-19, -0.9999939076577903929, -0.003490651415223739937 ) ) ;
#111317 = DIRECTION ( 'NONE',  ( 0.000000000000000000, 0.000000000000000000, 1.000000000000000000 ) ) ;
#111318 = DIRECTION ( 'NONE',  ( 0.000000000000000000, 1.000000000000000000, 0.000000000000000000 ) ) ;
#111319 = AXIS2_PLACEMENT_3D ( 'NONE', #94158, #62782, #22867 ) ;
#111320 = ORIENTED_EDGE ( 'NONE', *, *, #50731, .T. ) ;
#111321 = VECTOR ( 'NONE', #83147, 1000.000000000000000 ) ;
#111322 = CIRCLE ( 'NONE', #54904, 0.06509327318403745899 ) ;
#111323 = VERTEX_POINT ( 'NONE', #121854 ) ;
#111324 = EDGE_LOOP ( 'NONE', ( #121371, #18010, #83464, #6507 ) ) ;
#111325 = EDGE_CURVE ( 'NONE', #51506, #16102, #70819, .T. ) ;
#111326 = CARTESIAN_POINT ( 'NONE',  ( 5.199999999999935341, 12.50000000000000000, -0.3464101615137783474 ) ) ;
#111327 = EDGE_CURVE ( 'NONE', #83416, #48128, #81295, .T. ) ;
#111328 = CONICAL_SURFACE ( 'NONE', #4720, 0.1000000000000002554, 0.003490658503988666988 ) ;
#111329 = ADVANCED_FACE ( 'NONE', ( #32214 ), #66285, .T. ) ;
#111330 = ORIENTED_EDGE ( 'NONE', *, *, #95147, .F. ) ;
#111331 = DIRECTION ( 'NONE',  ( 0.000000000000000000, 0.000000000000000000, 1.000000000000000000 ) ) ;
#111332 = DIRECTION ( 'NONE',  ( 0.000000000000000000, 0.000000000000000000, 1.000000000000000000 ) ) ;
#111333 = VECTOR ( 'NONE', #47684, 1000.000000000000000 ) ;
#111334 = EDGE_CURVE ( 'NONE', #1500, #18199, #26306, .T. ) ;
#111335 = ORIENTED_EDGE ( 'NONE', *, *, #72479, .T. ) ;
#111336 = CARTESIAN_POINT ( 'NONE',  ( 0.5999999999999560130, 2.500000000000000000, -4.083716857408426826 ) ) ;
#111337 = DIRECTION ( 'NONE',  ( -0.000000000000000000, -1.000000000000000000, -0.000000000000000000 ) ) ;
#111338 = CARTESIAN_POINT ( 'NONE',  ( -1.050000000000037348, 12.50000000000000000, -2.511473670974877948 ) ) ;
#111339 = CARTESIAN_POINT ( 'NONE',  ( 8.949999999999917577, 12.50000000000000000, 6.148780366869520009 ) ) ;
#111340 = EDGE_CURVE ( 'NONE', #55154, #99389, #26583, .T. ) ;
#111341 = EDGE_CURVE ( 'NONE', #122246, #22448, #34135, .T. ) ;
#111342 = CARTESIAN_POINT ( 'NONE',  ( 7.499999999999923617, 2.500000000000000000, 0.6928203230275494784 ) ) ;
#111343 = ORIENTED_EDGE ( 'NONE', *, *, #102912, .T. ) ;
#111344 = CONICAL_SURFACE ( 'NONE', #65390, 0.1000000000000000472, 0.003490658503988666988 ) ;
#111345 = ORIENTED_EDGE ( 'NONE', *, *, #83451, .T. ) ;
#111346 = AXIS2_PLACEMENT_3D ( 'NONE', #65449, #43266, #24892 ) ;
#111347 = CARTESIAN_POINT ( 'NONE',  ( 7.299999999999924327, 12.50000000000000000, 0.2813168883297361700 ) ) ;
#111348 = CARTESIAN_POINT ( 'NONE',  ( 1.649999999999951950, 12.50000000000000000, -5.802370205355749988 ) ) ;
#111349 = EDGE_CURVE ( 'NONE', #4289, #32314, #104773, .T. ) ;
#111350 = CARTESIAN_POINT ( 'NONE',  ( 6.849999999999927702, 2.500000000000000000, 2.611473670974873151 ) ) ;
#111351 = DIRECTION ( 'NONE',  ( 0.000000000000000000, -0.9999939076577903929, 0.003490651415223739937 ) ) ;
#111352 = ORIENTED_EDGE ( 'NONE', *, *, #17830, .T. ) ;
#111353 = CIRCLE ( 'NONE', #94639, 0.06509327318403745899 ) ;
#111354 = CIRCLE ( 'NONE', #48598, 0.06509327318403741736 ) ;
#111355 = CIRCLE ( 'NONE', #38238, 0.06509327318403745899 ) ;
#111356 = ORIENTED_EDGE ( 'NONE', *, *, #129164, .F. ) ;
#111357 = DIRECTION ( 'NONE',  ( -0.000000000000000000, -1.000000000000000000, -0.000000000000000000 ) ) ;
#111358 = PLANE ( 'NONE',  #30041 ) ;
#111359 = CARTESIAN_POINT ( 'NONE',  ( 8.749999999999920064, 2.500000000000000000, 5.902370205355745192 ) ) ;
#111360 = PLANE ( 'NONE',  #11238 ) ;
#111361 = VERTEX_POINT ( 'NONE', #82592 ) ;
#111363 = DIRECTION ( 'NONE',  ( 0.000000000000000000, 0.000000000000000000, -1.000000000000000000 ) ) ;
#111362 = CIRCLE ( 'NONE', #23649, 0.1000000000000002554 ) ;
#111364 = CIRCLE ( 'NONE', #25704, 0.06509327318403745899 ) ;
#111365 = CONICAL_SURFACE ( 'NONE', #128118, 0.1000000000000002554, 0.003490658503988666988 ) ;
#111366 = CARTESIAN_POINT ( 'NONE',  ( 8.749999999999923617, 12.50000000000000000, -7.188010851410854052 ) ) ;
#111367 = AXIS2_PLACEMENT_3D ( 'NONE', #112746, #23071, #13227 ) ;
#111368 = VERTEX_POINT ( 'NONE', #93053 ) ;
#111369 = CIRCLE ( 'NONE', #75886, 0.1000000000000002554 ) ;
#111370 = DIRECTION ( 'NONE',  ( 0.000000000000000000, 0.000000000000000000, -1.000000000000000000 ) ) ;
#111371 = ADVANCED_FACE ( 'NONE', ( #64860 ), #124441, .T. ) ;
#111372 = VERTEX_POINT ( 'NONE', #12536 ) ;
#111373 = AXIS2_PLACEMENT_3D ( 'NONE', #20704, #13442, #50810 ) ;
#111374 = DIRECTION ( 'NONE',  ( 0.000000000000000000, 0.000000000000000000, -1.000000000000000000 ) ) ;
#111375 = VERTEX_POINT ( 'NONE', #94316 ) ;
#111376 = ORIENTED_EDGE ( 'NONE', *, *, #116372, .T. ) ;
#111377 = DIRECTION ( 'NONE',  ( 0.000000000000000000, 0.000000000000000000, 1.000000000000000000 ) ) ;
#111378 = DIRECTION ( 'NONE',  ( 0.000000000000000000, 1.000000000000000000, 0.000000000000000000 ) ) ;
#111379 = EDGE_LOOP ( 'NONE', ( #121244, #121804 ) ) ;
#111380 = ORIENTED_EDGE ( 'NONE', *, *, #13493, .F. ) ;
#111381 = DIRECTION ( 'NONE',  ( 0.000000000000000000, -0.000000000000000000, 1.000000000000000000 ) ) ;
#111382 = DIRECTION ( 'NONE',  ( 0.000000000000000000, 1.000000000000000000, 0.000000000000000000 ) ) ;
#111383 = ORIENTED_EDGE ( 'NONE', *, *, #115236, .F. ) ;
#111384 = CIRCLE ( 'NONE', #61241, 0.06509327318403745899 ) ;
#111385 = DIRECTION ( 'NONE',  ( 0.000000000000000000, 0.000000000000000000, 1.000000000000000000 ) ) ;
#111386 = CARTESIAN_POINT ( 'NONE',  ( 184.7343750003414016, 8.734944146203032389, 5.348610694689227483E-16 ) ) ;
#111387 = ADVANCED_FACE ( 'NONE', ( #85150 ), #62309, .T. ) ;
#111388 = CARTESIAN_POINT ( 'NONE',  ( -14.99999999999998224, 12.50000000000000000, -0.6928203230275519209 ) ) ;
#111389 = CARTESIAN_POINT ( 'NONE',  ( 6.049999999999930544, 2.500000000000000000, 2.411473670974873862 ) ) ;
#111390 = CARTESIAN_POINT ( 'NONE',  ( -14.14999999999998614, 2.500000000000000000, 2.265063509461101354 ) ) ;
#111391 = CARTESIAN_POINT ( 'NONE',  ( -1.850000000000033840, 2.500000000000000000, 6.941600689897073018 ) ) ;
#111392 = DIRECTION ( 'NONE',  ( 0.000000000000000000, -0.9999939076577903929, 0.003490651415223739937 ) ) ;
#111393 = AXIS2_PLACEMENT_3D ( 'NONE', #45370, #5418, #49725 ) ;
#111394 = CIRCLE ( 'NONE', #19367, 0.06509327318403745899 ) ;
#111395 = CIRCLE ( 'NONE', #38271, 0.06509327318403745899 ) ;
#111396 = ORIENTED_EDGE ( 'NONE', *, *, #121855, .T. ) ;
#111397 = ORIENTED_EDGE ( 'NONE', *, *, #24558, .T. ) ;
#111398 = CARTESIAN_POINT ( 'NONE',  ( 13.74999999999993072, 12.50000000000000000, -2.165063509461101710 ) ) ;
#111399 = ORIENTED_EDGE ( 'NONE', *, *, #33064, .F. ) ;
#111400 = DIRECTION ( 'NONE',  ( 0.000000000000000000, 1.000000000000000000, 0.000000000000000000 ) ) ;
#111401 = DIRECTION ( 'NONE',  ( -0.000000000000000000, 1.000000000000000000, -0.000000000000000000 ) ) ;
#111402 = DIRECTION ( 'NONE',  ( -0.000000000000000000, 1.000000000000000000, -0.000000000000000000 ) ) ;
#111404 = ORIENTED_EDGE ( 'NONE', *, *, #115747, .F. ) ;
#111403 = ORIENTED_EDGE ( 'NONE', *, *, #122447, .F. ) ;
#111405 = FACE_BOUND ( 'NONE', #39259, .T. ) ;
#111406 = ORIENTED_EDGE ( 'NONE', *, *, #11097, .F. ) ;
#111407 = DIRECTION ( 'NONE',  ( 0.000000000000000000, 0.000000000000000000, 1.000000000000000000 ) ) ;
#111408 = CARTESIAN_POINT ( 'NONE',  ( 7.499999999999960032, 12.50000000000000000, -2.276824562219559311E-15 ) ) ;
#111409 = AXIS2_PLACEMENT_3D ( 'NONE', #74775, #43395, #102933 ) ;
#111411 = LINE ( 'NONE', #21771, #128497 ) ;
#111410 = CIRCLE ( 'NONE', #121892, 0.1000000000000002554 ) ;
#111412 = DIRECTION ( 'NONE',  ( -0.000000000000000000, -1.000000000000000000, -0.000000000000000000 ) ) ;
#111413 = CIRCLE ( 'NONE', #92651, 0.06509327318403745899 ) ;
#111414 = LINE ( 'NONE', #21773, #120411 ) ;
#111415 = CARTESIAN_POINT ( 'NONE',  ( 12.89999999999989733, 2.500000000000000000, -2.385244779468109755E-15 ) ) ;
#111416 = DIRECTION ( 'NONE',  ( -0.000000000000000000, -1.000000000000000000, -0.000000000000000000 ) ) ;
#111417 = CARTESIAN_POINT ( 'NONE',  ( 2.899999999999945732, 2.500000000000000000, -0.1000000000000023925 ) ) ;
#111418 = LINE ( 'NONE', #101630, #105975 ) ;
#111419 = LINE ( 'NONE', #112089, #92478 ) ;
#111420 = CIRCLE ( 'NONE', #54996, 0.1000000000000002554 ) ;
#111421 = CARTESIAN_POINT ( 'NONE',  ( -2.900000000000030109, 2.500000000000000000, 0.6928203230275494784 ) ) ;
#111422 = ORIENTED_EDGE ( 'NONE', *, *, #102356, .F. ) ;
#111423 = ORIENTED_EDGE ( 'NONE', *, *, #99973, .F. ) ;
#111424 = VERTEX_POINT ( 'NONE', #32857 ) ;
#111426 = ORIENTED_EDGE ( 'NONE', *, *, #119909, .F. ) ;
#111425 = AXIS2_PLACEMENT_3D ( 'NONE', #92813, #71218, #3137 ) ;
#111427 = CIRCLE ( 'NONE', #100976, 0.06509327318403745899 ) ;
#111428 = CIRCLE ( 'NONE', #126104, 0.06509327318403745899 ) ;
#111429 = CARTESIAN_POINT ( 'NONE',  ( -6.850000000000013856, 2.500000000000000000, 6.048780366869521252 ) ) ;
#111430 = DIRECTION ( 'NONE',  ( 0.000000000000000000, -0.000000000000000000, 1.000000000000000000 ) ) ;
#111432 = EDGE_LOOP ( 'NONE', ( #25544, #121283, #117762, #116183 ) ) ;
#111431 = ORIENTED_EDGE ( 'NONE', *, *, #98624, .T. ) ;
#111433 = EDGE_LOOP ( 'NONE', ( #73143, #22921 ) ) ;
#111434 = VECTOR ( 'NONE', #36412, 1000.000000000000000 ) ;
#111435 = CARTESIAN_POINT ( 'NONE',  ( -9.550000000000002487, 12.50000000000000000, 6.495190528383297135 ) ) ;
#111436 = EDGE_CURVE ( 'NONE', #60385, #4249, #4633, .T. ) ;
#111437 = DIRECTION ( 'NONE',  ( -0.000000000000000000, 1.000000000000000000, -0.000000000000000000 ) ) ;
#111438 = CIRCLE ( 'NONE', #55006, 0.1000000000000000056 ) ;
#111439 = SURFACE_SIDE_STYLE ('',( #81367 ) ) ;
#111440 = FACE_OUTER_BOUND ( 'NONE', #70771, .T. ) ;
#111441 = LINE ( 'NONE', #91818, #68024 ) ;
#111442 = CARTESIAN_POINT ( 'NONE',  ( -10.85000000000000142, 12.50000000000000000, 2.165063509461097713 ) ) ;
#111443 = CARTESIAN_POINT ( 'NONE',  ( 3.749999999999938716, 2.500000000000000000, 7.188010851410848723 ) ) ;
#111444 = ADVANCED_FACE ( 'NONE', ( #114605 ), #60049, .T. ) ;
#111445 = ORIENTED_EDGE ( 'NONE', *, *, #101596, .F. ) ;
#111446 = EDGE_CURVE ( 'NONE', #25426, #106311, #1429, .T. ) ;
#111447 = CARTESIAN_POINT ( 'NONE',  ( 8.349999999999923261, 2.500000000000000000, 2.757883832488649656 ) ) ;
#111448 = VERTEX_POINT ( 'NONE', #112046 ) ;
#111449 = ORIENTED_EDGE ( 'NONE', *, *, #123420, .T. ) ;
#111450 = ORIENTED_EDGE ( 'NONE', *, *, #109888, .F. ) ;
#111451 = EDGE_CURVE ( 'NONE', #49607, #66867, #32580, .T. ) ;
#111453 = EDGE_CURVE ( 'NONE', #82216, #56145, #112269, .T. ) ;
#111452 = CARTESIAN_POINT ( 'NONE',  ( -6.250000000000021316, 2.500000000000000000, -5.802370205355749988 ) ) ;
#111454 = CIRCLE ( 'NONE', #9048, 0.1000000000000002554 ) ;
#111456 = ORIENTED_EDGE ( 'NONE', *, *, #38060, .F. ) ;
#111455 = ADVANCED_FACE ( 'NONE', ( #52465 ), #78832, .T. ) ;
#111457 = EDGE_LOOP ( 'NONE', ( #117315, #64072, #7826, #28091 ) ) ;
#111458 = EDGE_CURVE ( 'NONE', #40679, #93080, #5628, .T. ) ;
#111460 = ORIENTED_EDGE ( 'NONE', *, *, #39420, .F. ) ;
#111459 = ADVANCED_FACE ( 'NONE', ( #112692 ), #53127, .T. ) ;
#111461 = CARTESIAN_POINT ( 'NONE',  ( 6.649999999999929301, 12.50000000000000000, 6.495190528383297135 ) ) ;
#111463 = FACE_OUTER_BOUND ( 'NONE', #58956, .T. ) ;
#111462 = VECTOR ( 'NONE', #128627, 1000.000000000000000 ) ;
#111464 = PLANE ( 'NONE',  #93920 ) ;
#111466 = DIRECTION ( 'NONE',  ( -0.000000000000000000, 1.000000000000000000, -0.000000000000000000 ) ) ;
#111465 = CONICAL_SURFACE ( 'NONE', #55029, 0.1000000000000002554, 0.003490658503988666988 ) ;
#111467 = DIRECTION ( 'NONE',  ( 0.000000000000000000, 1.000000000000000000, 0.000000000000000000 ) ) ;
#111468 = AXIS2_PLACEMENT_3D ( 'NONE', #39829, #119645, #69917 ) ;
#111469 = AXIS2_PLACEMENT_3D ( 'NONE', #73013, #11511, #51456 ) ;
#111470 = LINE ( 'NONE', #31014, #106838 ) ;
#111471 = ADVANCED_FACE ( 'NONE', ( #33498 ), #93484, .T. ) ;
#111472 = CARTESIAN_POINT ( 'NONE',  ( -3.350000000000028511, 2.500000000000000000, -1.472243186433550122 ) ) ;
#111473 = AXIS2_PLACEMENT_3D ( 'NONE', #11209, #51159, #112648 ) ;
#111475 = ORIENTED_EDGE ( 'NONE', *, *, #42626, .T. ) ;
#111474 = CONICAL_SURFACE ( 'NONE', #98960, 0.1000000000000000472, 0.003490658503988666988 ) ;
#111476 = DIRECTION ( 'NONE',  ( -0.000000000000000000, -1.000000000000000000, -0.000000000000000000 ) ) ;
#111477 = CONICAL_SURFACE ( 'NONE', #105218, 0.09999999999999982514, 0.003490658503988666988 ) ;
#111478 = ORIENTED_EDGE ( 'NONE', *, *, #112042, .F. ) ;
#111479 = DIRECTION ( 'NONE',  ( 0.000000000000000000, 0.000000000000000000, 1.000000000000000000 ) ) ;
#111480 = AXIS2_PLACEMENT_3D ( 'NONE', #120942, #113052, #24047 ) ;
#111481 = EDGE_LOOP ( 'NONE', ( #68592, #101082 ) ) ;
#111482 = CONICAL_SURFACE ( 'NONE', #88488, 0.1000000000000002554, 0.003490658503988666988 ) ;
#111483 = LINE ( 'NONE', #101678, #67702 ) ;
#111484 = ORIENTED_EDGE ( 'NONE', *, *, #56071, .F. ) ;
#111485 = VECTOR ( 'NONE', #8600, 1000.000000000000000 ) ;
#111486 = FACE_OUTER_BOUND ( 'NONE', #63844, .T. ) ;
#111487 = DIRECTION ( 'NONE',  ( 0.000000000000000000, -0.000000000000000000, 1.000000000000000000 ) ) ;
#111488 = ORIENTED_EDGE ( 'NONE', *, *, #80176, .F. ) ;
#111489 = ORIENTED_EDGE ( 'NONE', *, *, #35976, .F. ) ;
#111490 = DIRECTION ( 'NONE',  ( 0.000000000000000000, 0.000000000000000000, -1.000000000000000000 ) ) ;
#111491 = DIRECTION ( 'NONE',  ( -4.274815082592931898E-19, -0.9999939076577903929, -0.003490651415223739937 ) ) ;
#111492 = DIRECTION ( 'NONE',  ( -4.274815082592931898E-19, -0.9999939076577903929, -0.003490651415223739937 ) ) ;
#111493 = CARTESIAN_POINT ( 'NONE',  ( 1.449999999999952216, 2.500000000000000000, 1.818653347947321475 ) ) ;
#111494 = AXIS2_PLACEMENT_3D ( 'NONE', #127173, #27642, #25725 ) ;
#111495 = PLANE ( 'NONE',  #16579 ) ;
#111496 = ORIENTED_EDGE ( 'NONE', *, *, #7593, .T. ) ;
#111497 = DIRECTION ( 'NONE',  ( 0.000000000000000000, 0.000000000000000000, 1.000000000000000000 ) ) ;
#111498 = EDGE_CURVE ( 'NONE', #100972, #113211, #20318, .T. ) ;
#111499 = EDGE_CURVE ( 'NONE', #90496, #36406, #76564, .T. ) ;
#111500 = AXIS2_PLACEMENT_3D ( 'NONE', #122327, #120385, #110552 ) ;
#111501 = ADVANCED_FACE ( 'NONE', ( #6552 ), #32677, .T. ) ;
#111502 = ORIENTED_EDGE ( 'NONE', *, *, #58771, .T. ) ;
#111503 = AXIS2_PLACEMENT_3D ( 'NONE', #82772, #53305, #101102 ) ;
#111504 = DIRECTION ( 'NONE',  ( -0.000000000000000000, -1.000000000000000000, -0.000000000000000000 ) ) ;
#111505 = DIRECTION ( 'NONE',  ( 0.000000000000000000, -0.9999939076577903929, 0.003490651415223739937 ) ) ;
#111506 = AXIS2_PLACEMENT_3D ( 'NONE', #57947, #128639, #107012 ) ;
#111507 = EDGE_CURVE ( 'NONE', #52727, #17050, #36778, .T. ) ;
#111508 = CARTESIAN_POINT ( 'NONE',  ( 186.9218750003414016, 0.000000000000000000, 7.564683531250000925 ) ) ;
#111509 = CARTESIAN_POINT ( 'NONE',  ( -12.09999999999999432, 12.50000000000000000, 3.572213422710607489 ) ) ;
#111510 = CARTESIAN_POINT ( 'NONE',  ( -9.150000000000009237, 12.50000000000000000, 2.922977105672686982 ) ) ;
#111511 = EDGE_CURVE ( 'NONE', #39415, #13047, #30525, .T. ) ;
#111512 = DIRECTION ( 'NONE',  ( 0.000000000000000000, 0.000000000000000000, 1.000000000000000000 ) ) ;
#111513 = AXIS2_PLACEMENT_3D ( 'NONE', #126858, #57475, #105925 ) ;
#111515 = AXIS2_PLACEMENT_3D ( 'NONE', #39066, #129382, #8915 ) ;
#111514 = CARTESIAN_POINT ( 'NONE',  ( -10.40000000000000213, 2.500000000000000000, 4.430127018922196847 ) ) ;
#111516 = EDGE_LOOP ( 'NONE', ( #55261, #57659, #94112, #89405 ) ) ;
#111517 = ADVANCED_FACE ( 'NONE', ( #108013 ), #25574, .T. ) ;
#111518 = VECTOR ( 'NONE', #76356, 1000.000000000000000 ) ;
#111519 = EDGE_CURVE ( 'NONE', #115994, #5036, #101606, .T. ) ;
#111520 = AXIS2_PLACEMENT_3D ( 'NONE', #98616, #18137, #108450 ) ;
#111521 = CARTESIAN_POINT ( 'NONE',  ( 7.049999999999926992, 2.500000000000000000, 2.265063509461097357 ) ) ;
#111522 = EDGE_CURVE ( 'NONE', #54526, #2989, #9659, .T. ) ;
#111523 = CARTESIAN_POINT ( 'NONE',  ( -3.100000000000028511, 2.500000000000000000, -0.2464101615137782308 ) ) ;
#111524 = DIRECTION ( 'NONE',  ( 0.000000000000000000, 0.000000000000000000, 1.000000000000000000 ) ) ;
#111525 = AXIS2_PLACEMENT_3D ( 'NONE', #53488, #3098, #15 ) ;
#111526 = EDGE_LOOP ( 'NONE', ( #68191, #5941, #66069, #8578 ) ) ;
#111527 = EDGE_CURVE ( 'NONE', #91651, #224, #70208, .T. ) ;
#111528 = FACE_OUTER_BOUND ( 'NONE', #10661, .T. ) ;
#111529 = ORIENTED_EDGE ( 'NONE', *, *, #45187, .T. ) ;
#111530 = VECTOR ( 'NONE', #9477, 1000.000000000000000 ) ;
#111532 = ORIENTED_EDGE ( 'NONE', *, *, #39747, .T. ) ;
#111531 = AXIS2_PLACEMENT_3D ( 'NONE', #58540, #17950, #19897 ) ;
#111533 = AXIS2_PLACEMENT_3D ( 'NONE', #84885, #53507, #113051 ) ;
#111534 = DIRECTION ( 'NONE',  ( 0.000000000000000000, 0.000000000000000000, 1.000000000000000000 ) ) ;
#111536 = ORIENTED_EDGE ( 'NONE', *, *, #21602, .T. ) ;
#111535 = AXIS2_PLACEMENT_3D ( 'NONE', #86770, #67104, #37049 ) ;
#111537 = CARTESIAN_POINT ( 'NONE',  ( 18.93069778776242273, -2.571126379696489828, -2.451182541063237075 ) ) ;
#111538 = CARTESIAN_POINT ( 'NONE',  ( 0.4499999999999552136, 2.500000000000000000, 6.495190528383297135 ) ) ;
#111539 = CARTESIAN_POINT ( 'NONE',  ( 20.06694580393655158, 2.635910463901408374, 2.269534205244102321 ) ) ;
#111540 = VECTOR ( 'NONE', #68894, 1000.000000000000000 ) ;
#111541 = EDGE_LOOP ( 'NONE', ( #120696, #128432, #93745, #31304 ) ) ;
#111542 = DIRECTION ( 'NONE',  ( 0.000000000000000000, 1.000000000000000000, 0.000000000000000000 ) ) ;
#111543 = CARTESIAN_POINT ( 'NONE',  ( 5.399999999999935518, 12.50000000000000000, -4.330127018922201643 ) ) ;
#111544 = EDGE_CURVE ( 'NONE', #46534, #3135, #36716, .T. ) ;
#111545 = ORIENTED_EDGE ( 'NONE', *, *, #73933, .T. ) ;
#111546 = ORIENTED_EDGE ( 'NONE', *, *, #34554, .F. ) ;
#111547 = VERTEX_POINT ( 'NONE', #26246 ) ;
#111548 = DIRECTION ( 'NONE',  ( -0.000000000000000000, 1.000000000000000000, -0.000000000000000000 ) ) ;
#111549 = DIRECTION ( 'NONE',  ( 0.000000000000000000, 1.000000000000000000, 0.000000000000000000 ) ) ;
#111551 = CARTESIAN_POINT ( 'NONE',  ( 13.54999999999989946, 12.50000000000000000, 2.511473670974873507 ) ) ;
#111550 = AXIS2_PLACEMENT_3D ( 'NONE', #43724, #4384, #44333 ) ;
#111552 = FACE_BOUND ( 'NONE', #69228, .T. ) ;
#111553 = ORIENTED_EDGE ( 'NONE', *, *, #35668, .F. ) ;
#111554 = CARTESIAN_POINT ( 'NONE',  ( -1.900000000000034550, 2.500000000000000000, 4.776537180435972196 ) ) ;
#111555 = FACE_OUTER_BOUND ( 'NONE', #122859, .T. ) ;
#111556 = EDGE_LOOP ( 'NONE', ( #30171, #94767 ) ) ;
#111557 = DIRECTION ( 'NONE',  ( 0.000000000000000000, 1.000000000000000000, 0.000000000000000000 ) ) ;
#111558 = CARTESIAN_POINT ( 'NONE',  ( 5.399999999999932854, 2.500000000000000000, 5.022947341949748790 ) ) ;
#111559 = AXIS2_PLACEMENT_3D ( 'NONE', #27285, #107131, #97963 ) ;
#111560 = ADVANCED_FACE ( 'NONE', ( #56327 ), #49392, .T. ) ;
#111561 = CONICAL_SURFACE ( 'NONE', #105208, 0.1000000000000000472, 0.003490658503988666988 ) ;
#111562 = CONICAL_SURFACE ( 'NONE', #32169, 0.1000000000000002554, 0.003490658503988666988 ) ;
#111564 = CIRCLE ( 'NONE', #103154, 0.1000000000000002554 ) ;
#111563 = DIRECTION ( 'NONE',  ( 0.000000000000000000, 0.000000000000000000, 1.000000000000000000 ) ) ;
#111565 = DIRECTION ( 'NONE',  ( -4.274815082592931898E-19, -0.9999939076577903929, -0.003490651415223739937 ) ) ;
#111566 = CARTESIAN_POINT ( 'NONE',  ( 12.09999999999990550, 2.500000000000000000, -3.737306695894649700 ) ) ;
#111567 = CARTESIAN_POINT ( 'NONE',  ( -0.4500000000000397571, 2.500000000000000000, -6.495190528383302464 ) ) ;
#111568 = DIRECTION ( 'NONE',  ( 0.000000000000000000, -0.000000000000000000, 1.000000000000000000 ) ) ;
#111569 = CONICAL_SURFACE ( 'NONE', #88588, 0.1000000000000002554, 0.003490658503988666988 ) ;
#111570 = CIRCLE ( 'NONE', #67745, 0.1000000000000002554 ) ;
#111571 = CIRCLE ( 'NONE', #32180, 0.06509327318403745899 ) ;
#111572 = ORIENTED_EDGE ( 'NONE', *, *, #26639, .F. ) ;
#111573 = VERTEX_POINT ( 'NONE', #45886 ) ;
#111574 = ORIENTED_EDGE ( 'NONE', *, *, #41468, .T. ) ;
#111575 = VERTEX_POINT ( 'NONE', #77272 ) ;
#111576 = DIRECTION ( 'NONE',  ( -0.000000000000000000, -1.000000000000000000, -0.000000000000000000 ) ) ;
#111577 = CIRCLE ( 'NONE', #76170, 0.06509327318403745899 ) ;
#111578 = CARTESIAN_POINT ( 'NONE',  ( 5.799999999999931433, 2.500000000000000000, 4.430127018922196847 ) ) ;
#111579 = ORIENTED_EDGE ( 'NONE', *, *, #56745, .T. ) ;
#111580 = EDGE_CURVE ( 'NONE', #125708, #120954, #8510, .T. ) ;
#111581 = FACE_BOUND ( 'NONE', #72039, .T. ) ;
#111582 = DIRECTION ( 'NONE',  ( -1.000000000000000000, 0.000000000000000000, 0.000000000000000000 ) ) ;
#111583 = CARTESIAN_POINT ( 'NONE',  ( 0.4499999999999569344, 12.50000000000000000, -2.165063509461101710 ) ) ;
#111584 = DIRECTION ( 'NONE',  ( -4.274815082592931898E-19, -0.9999939076577903929, -0.003490651415223739937 ) ) ;
#111585 = DIRECTION ( 'NONE',  ( 0.000000000000000000, 0.000000000000000000, 1.000000000000000000 ) ) ;
#111586 = DIRECTION ( 'NONE',  ( -0.000000000000000000, 1.000000000000000000, -0.000000000000000000 ) ) ;
#111587 = LINE ( 'NONE', #118827, #101873 ) ;
#111588 = DIRECTION ( 'NONE',  ( 0.000000000000000000, -0.000000000000000000, 1.000000000000000000 ) ) ;
#111589 = CARTESIAN_POINT ( 'NONE',  ( -11.89999999999999680, 12.50000000000000000, 0.3464101615137776813 ) ) ;
#111590 =( REPRESENTATION_RELATIONSHIP ('NONE','NONE', #102928, #5058 ) REPRESENTATION_RELATIONSHIP_WITH_TRANSFORMATION ( #59502 )SHAPE_REPRESENTATION_RELATIONSHIP( ) );
#111591 = DIRECTION ( 'NONE',  ( 0.000000000000000000, 0.000000000000000000, -1.000000000000000000 ) ) ;
#111592 = EDGE_LOOP ( 'NONE', ( #79483, #64185 ) ) ;
#111593 = AXIS2_PLACEMENT_3D ( 'NONE', #53748, #124429, #42666 ) ;
#111594 = EDGE_LOOP ( 'NONE', ( #77815, #23027 ) ) ;
#111595 = VERTEX_POINT ( 'NONE', #55691 ) ;
#111596 = EDGE_LOOP ( 'NONE', ( #34255, #118721, #68364, #74566 ) ) ;
#111597 = EDGE_LOOP ( 'NONE', ( #78445, #1485 ) ) ;
#111598 = VERTEX_POINT ( 'NONE', #57639 ) ;
#111599 = CARTESIAN_POINT ( 'NONE',  ( 3.349999999999944578, 2.500000000000000000, -1.372243186433550033 ) ) ;
#111600 = EDGE_LOOP ( 'NONE', ( #41498, #7388, #45423, #118198 ) ) ;
#111601 = EDGE_LOOP ( 'NONE', ( #38846, #485, #106599, #68152 ) ) ;
#111602 = CIRCLE ( 'NONE', #86450, 0.06509327318403745899 ) ;
#111603 = AXIS2_PLACEMENT_3D ( 'NONE', #806, #80673, #42031 ) ;
#111604 = AXIS2_PLACEMENT_3D ( 'NONE', #34123, #32204, #53752 ) ;
#111605 = ADVANCED_FACE ( 'NONE', ( #7874 ), #95625, .T. ) ;
#111606 = DIRECTION ( 'NONE',  ( 0.000000000000000000, 0.000000000000000000, 1.000000000000000000 ) ) ;
#111607 = CARTESIAN_POINT ( 'NONE',  ( -11.89999999999999503, 12.50000000000000000, 4.676537180435972552 ) ) ;
#111608 = CARTESIAN_POINT ( 'NONE',  ( 6.649999999999930189, 2.500000000000000000, 5.802370205355744659 ) ) ;
#111609 = DIRECTION ( 'NONE',  ( -0.000000000000000000, -1.000000000000000000, -0.000000000000000000 ) ) ;
#111610 = AXIS2_PLACEMENT_3D ( 'NONE', #41708, #22070, #12217 ) ;
#111611 = ORIENTED_EDGE ( 'NONE', *, *, #14775, .F. ) ;
#111612 = DIRECTION ( 'NONE',  ( 0.000000000000000000, 0.000000000000000000, 1.000000000000000000 ) ) ;
#111613 = AXIS2_PLACEMENT_3D ( 'NONE', #82849, #1676, #62560 ) ;
#111614 = AXIS2_PLACEMENT_3D ( 'NONE', #114191, #55274, #125298 ) ;
#111615 = EDGE_LOOP ( 'NONE', ( #18614, #21918, #75614, #93717 ) ) ;
#111616 = VECTOR ( 'NONE', #101868, 1000.000000000000000 ) ;
#111617 = VERTEX_POINT ( 'NONE', #75978 ) ;
#111618 = DIRECTION ( 'NONE',  ( -4.274815082592931898E-19, -0.9999939076577903929, -0.003490651415223739937 ) ) ;
#111619 = EDGE_CURVE ( 'NONE', #74365, #7606, #66151, .T. ) ;
#111620 = DIRECTION ( 'NONE',  ( 0.000000000000000000, 0.000000000000000000, 1.000000000000000000 ) ) ;
#111622 = EDGE_CURVE ( 'NONE', #88783, #13760, #114118, .T. ) ;
#111621 = FACE_OUTER_BOUND ( 'NONE', #118891, .T. ) ;
#111623 = EDGE_CURVE ( 'NONE', #61624, #83259, #55634, .T. ) ;
#111624 = EDGE_CURVE ( 'NONE', #73740, #16607, #95128, .T. ) ;
#111625 = VERTEX_POINT ( 'NONE', #41237 ) ;
#111626 = ORIENTED_EDGE ( 'NONE', *, *, #34966, .F. ) ;
#111627 = DIRECTION ( 'NONE',  ( -0.000000000000000000, 1.000000000000000000, -0.000000000000000000 ) ) ;
#111630 = EDGE_CURVE ( 'NONE', #62406, #64648, #20047, .T. ) ;
#111629 = CIRCLE ( 'NONE', #51005, 0.09999999999999982514 ) ;
#111628 = DIRECTION ( 'NONE',  ( 0.000000000000000000, 1.000000000000000000, 0.000000000000000000 ) ) ;
#111632 = CIRCLE ( 'NONE', #7052, 0.1000000000000002554 ) ;
#111631 = DIRECTION ( 'NONE',  ( 0.000000000000000000, -0.000000000000000000, 1.000000000000000000 ) ) ;
#111633 = CONICAL_SURFACE ( 'NONE', #13414, 0.1000000000000002554, 0.003490658503988666988 ) ;
#111634 = CARTESIAN_POINT ( 'NONE',  ( 1.649999999999950617, 12.50000000000000000, -2.165063509461101710 ) ) ;
#111635 = PLANE ( 'NONE',  #75312 ) ;
#111636 = CIRCLE ( 'NONE', #46888, 0.09999999999999982514 ) ;
#111637 = EDGE_CURVE ( 'NONE', #75483, #24362, #93203, .T. ) ;
#111638 = ORIENTED_EDGE ( 'NONE', *, *, #115485, .F. ) ;
#111639 = CIRCLE ( 'NONE', #86581, 0.09999999999999982514 ) ;
#111640 = CARTESIAN_POINT ( 'NONE',  ( -14.59999999999998366, 2.500000000000000000, 0.6928203230275518099 ) ) ;
#111641 = EDGE_CURVE ( 'NONE', #101677, #91963, #11710, .T. ) ;
#111642 = EDGE_CURVE ( 'NONE', #84952, #120463, #26399, .T. ) ;
#111643 = EDGE_LOOP ( 'NONE', ( #117549, #78846 ) ) ;
#111644 = CARTESIAN_POINT ( 'NONE',  ( 87.50000000000002842, 4.871203238224194543, -5.733266569811712010 ) ) ;
#111645 = CARTESIAN_POINT ( 'NONE',  ( 2.499999999999947153, 12.50000000000000000, -3.572213422710612374 ) ) ;
#111646 = PLANE ( 'NONE',  #34403 ) ;
#111647 = DIRECTION ( 'NONE',  ( 0.000000000000000000, 0.000000000000000000, -1.000000000000000000 ) ) ;
#111648 = PRODUCT_RELATED_PRODUCT_CATEGORY ( 'part', '', ( #7300 ) ) ;
#111650 = ADVANCED_FACE ( 'NONE', ( #18982 ), #128822, .T. ) ;
#111649 = DIRECTION ( 'NONE',  ( 0.000000000000000000, -0.9999939076577903929, 0.003490651415223739937 ) ) ;
#111651 = EDGE_LOOP ( 'NONE', ( #101377, #18783 ) ) ;
#111652 = DIRECTION ( 'NONE',  ( 0.000000000000000000, 1.000000000000000000, 0.000000000000000000 ) ) ;
#111654 = DIRECTION ( 'NONE',  ( 0.000000000000000000, 0.000000000000000000, 1.000000000000000000 ) ) ;
#111653 = CIRCLE ( 'NONE', #36455, 0.06509327318403745899 ) ;
#111655 = VERTEX_POINT ( 'NONE', #58924 ) ;
#111656 = VERTEX_POINT ( 'NONE', #81150 ) ;
#111657 = AXIS2_PLACEMENT_3D ( 'NONE', #67276, #106591, #107238 ) ;
#111658 = ORIENTED_EDGE ( 'NONE', *, *, #28487, .F. ) ;
#111659 = CARTESIAN_POINT ( 'NONE',  ( 17.50000000000000000, 0.9166666666666682950, 4.000000000000001776 ) ) ;
#111660 = DIRECTION ( 'NONE',  ( -0.000000000000000000, -1.000000000000000000, -0.000000000000000000 ) ) ;
#111661 = DIRECTION ( 'NONE',  ( 0.000000000000000000, 0.000000000000000000, 1.000000000000000000 ) ) ;
#111662 = LINE ( 'NONE', #22009, #63721 ) ;
#111663 = DIRECTION ( 'NONE',  ( -0.000000000000000000, -1.000000000000000000, -0.000000000000000000 ) ) ;
#111664 = VECTOR ( 'NONE', #66923, 1000.000000000000000 ) ;
#111665 = AXIS2_PLACEMENT_3D ( 'NONE', #53392, #12156, #92019 ) ;
#111666 = FACE_OUTER_BOUND ( 'NONE', #117114, .T. ) ;
#111667 = AXIS2_PLACEMENT_3D ( 'NONE', #20564, #81424, #101050 ) ;
#111668 = DIRECTION ( 'NONE',  ( -4.274815082592931898E-19, -0.9999939076577903929, -0.003490651415223739937 ) ) ;
#111670 = CIRCLE ( 'NONE', #46825, 0.06509327318403745899 ) ;
#111669 = CYLINDRICAL_SURFACE ( 'NONE', #111174, 7.699999999999999289 ) ;
#111671 = EDGE_CURVE ( 'NONE', #75028, #34064, #70038, .T. ) ;
#111672 = CONICAL_SURFACE ( 'NONE', #57287, 0.09999999999999982514, 0.003490658503988666988 ) ;
#111673 = AXIS2_PLACEMENT_3D ( 'NONE', #30689, #120983, #41803 ) ;
#111674 = ORIENTED_EDGE ( 'NONE', *, *, #45501, .F. ) ;
#111675 = FACE_OUTER_BOUND ( 'NONE', #88312, .T. ) ;
#111676 = CONICAL_SURFACE ( 'NONE', #97001, 0.09999999999999982514, 0.003490658503988666988 ) ;
#111677 = DIRECTION ( 'NONE',  ( 0.000000000000000000, -0.000000000000000000, 1.000000000000000000 ) ) ;
#111678 = FACE_OUTER_BOUND ( 'NONE', #8161, .T. ) ;
#111679 = DIRECTION ( 'NONE',  ( 0.000000000000000000, 0.000000000000000000, -1.000000000000000000 ) ) ;
#111680 = EDGE_LOOP ( 'NONE', ( #27900, #26726, #111966, #71975 ) ) ;
#111681 = CARTESIAN_POINT ( 'NONE',  ( -13.74999999999998934, 2.500000000000000000, -1.472243186433547901 ) ) ;
#111682 = EDGE_CURVE ( 'NONE', #15887, #109919, #57699, .T. ) ;
#111683 = EDGE_CURVE ( 'NONE', #122356, #36724, #51692, .T. ) ;
#111684 = DIRECTION ( 'NONE',  ( 0.000000000000000000, 0.000000000000000000, 1.000000000000000000 ) ) ;
#111686 = ORIENTED_EDGE ( 'NONE', *, *, #65718, .T. ) ;
#111685 = CARTESIAN_POINT ( 'NONE',  ( 8.299999999999922551, 12.50000000000000000, -4.330127018922201643 ) ) ;
#111687 = CIRCLE ( 'NONE', #128437, 0.06509327318403745899 ) ;
#111688 = ORIENTED_EDGE ( 'NONE', *, *, #42177, .F. ) ;
#111689 = EDGE_CURVE ( 'NONE', #62384, #14824, #24242, .T. ) ;
#111690 = DIRECTION ( 'NONE',  ( 0.000000000000000000, -0.000000000000000000, 1.000000000000000000 ) ) ;
#111691 = ORIENTED_EDGE ( 'NONE', *, *, #112002, .T. ) ;
#111692 = EDGE_LOOP ( 'NONE', ( #110589, #108009, #33941, #94653 ) ) ;
#111693 = DIRECTION ( 'NONE',  ( 0.000000000000000000, 0.000000000000000000, 1.000000000000000000 ) ) ;
#111694 = FACE_OUTER_BOUND ( 'NONE', #121443, .T. ) ;
#111695 = LINE ( 'NONE', #3667, #96471 ) ;
#111696 = AXIS2_PLACEMENT_3D ( 'NONE', #22738, #43032, #113023 ) ;
#111697 = CARTESIAN_POINT ( 'NONE',  ( 13.14999999999989733, 2.500000000000000000, -2.511473670974877948 ) ) ;
#111698 = CONICAL_SURFACE ( 'NONE', #51165, 0.1000000000000000472, 0.003490658503988666988 ) ;
#111699 = EDGE_LOOP ( 'NONE', ( #12533, #9909, #78018, #88770 ) ) ;
#111700 = DIRECTION ( 'NONE',  ( 0.000000000000000000, 1.000000000000000000, 0.000000000000000000 ) ) ;
#111701 = ORIENTED_EDGE ( 'NONE', *, *, #83718, .F. ) ;
#111702 = CARTESIAN_POINT ( 'NONE',  ( -3.950000000000029932, 2.500000000000000000, -6.148780366869526226 ) ) ;
#111703 = FACE_OUTER_BOUND ( 'NONE', #66838, .T. ) ;
#111704 = VERTEX_POINT ( 'NONE', #633 ) ;
#111705 = AXIS2_PLACEMENT_3D ( 'NONE', #41528, #70961, #99139 ) ;
#111706 = EDGE_LOOP ( 'NONE', ( #122200, #81143, #52094, #115989 ) ) ;
#111707 = ORIENTED_EDGE ( 'NONE', *, *, #82069, .T. ) ;
#111708 = ORIENTED_EDGE ( 'NONE', *, *, #104846, .T. ) ;
#111709 = CARTESIAN_POINT ( 'NONE',  ( -1.650000000000035660, 2.500000000000000000, 2.957883832488649389 ) ) ;
#111710 = LINE ( 'NONE', #20110, #35314 ) ;
#111711 = DIRECTION ( 'NONE',  ( 0.000000000000000000, 0.000000000000000000, 1.000000000000000000 ) ) ;
#111712 = FACE_BOUND ( 'NONE', #23293, .T. ) ;
#111713 = ORIENTED_EDGE ( 'NONE', *, *, #43289, .F. ) ;
#111714 = DIRECTION ( 'NONE',  ( 0.000000000000000000, -0.9999939076577903929, 0.003490651415223739937 ) ) ;
#111715 = CARTESIAN_POINT ( 'NONE',  ( 184.6979166673494603, 6.668395609140176816, 3.850000000000000977 ) ) ;
#111716 = CARTESIAN_POINT ( 'NONE',  ( 8.549999999999922551, 12.50000000000000000, -6.213873640053564351 ) ) ;
#111717 = CARTESIAN_POINT ( 'NONE',  ( -1.250000000000001110, 12.50000000000000000, -6.495190528383302464 ) ) ;
#111718 = CIRCLE ( 'NONE', #94998, 0.06509327318403745899 ) ;
#111719 = DIRECTION ( 'NONE',  ( 0.000000000000000000, 0.000000000000000000, 1.000000000000000000 ) ) ;
#111720 = CARTESIAN_POINT ( 'NONE',  ( -11.89999999999999680, 2.500000000000000000, -3.983716857408423628 ) ) ;
#111721 = DIRECTION ( 'NONE',  ( 0.000000000000000000, -0.9999939076577903929, 0.003490651415223739937 ) ) ;
#111722 = CONICAL_SURFACE ( 'NONE', #122198, 0.09999999999999982514, 0.003490658503988666988 ) ;
#111723 = CARTESIAN_POINT ( 'NONE',  ( 11.24999999999991118, 12.50000000000000000, 5.867463478539781896 ) ) ;
#111724 = ORIENTED_EDGE ( 'NONE', *, *, #126904, .T. ) ;
#111725 = ORIENTED_EDGE ( 'NONE', *, *, #105236, .T. ) ;
#111726 = ORIENTED_EDGE ( 'NONE', *, *, #63155, .T. ) ;
#111727 = ORIENTED_EDGE ( 'NONE', *, *, #73991, .F. ) ;
#111729 = ORIENTED_EDGE ( 'NONE', *, *, #22573, .T. ) ;
#111728 = EDGE_CURVE ( 'NONE', #65690, #7809, #99560, .T. ) ;
#111730 = DIRECTION ( 'NONE',  ( 0.000000000000000000, 0.000000000000000000, 1.000000000000000000 ) ) ;
#111731 = FACE_OUTER_BOUND ( 'NONE', #80618, .T. ) ;
#111732 = ORIENTED_EDGE ( 'NONE', *, *, #53993, .T. ) ;
#111733 = EDGE_CURVE ( 'NONE', #20397, #14404, #9821, .T. ) ;
#111734 = FACE_BOUND ( 'NONE', #18432, .T. ) ;
#111735 = CARTESIAN_POINT ( 'NONE',  ( 8.349999999999923261, 2.500000000000000000, -7.188010851410854052 ) ) ;
#111736 = AXIS2_PLACEMENT_3D ( 'NONE', #44508, #43888, #84439 ) ;
#111737 = AXIS2_PLACEMENT_3D ( 'NONE', #29245, #109728, #69798 ) ;
#111738 = VERTEX_POINT ( 'NONE', #10459 ) ;
#111740 = VECTOR ( 'NONE', #89391, 1000.000000000000000 ) ;
#111739 = FACE_OUTER_BOUND ( 'NONE', #125656, .T. ) ;
#111741 = CARTESIAN_POINT ( 'NONE',  ( -12.49999999999999467, 2.500000000000000000, 0.5928203230275536084 ) ) ;
#111742 = EDGE_CURVE ( 'NONE', #56826, #33171, #59868, .T. ) ;
#111743 = DIRECTION ( 'NONE',  ( -0.000000000000000000, 1.000000000000000000, -0.000000000000000000 ) ) ;
#111744 = CARTESIAN_POINT ( 'NONE',  ( -8.350000000000012079, 12.50000000000000000, -2.857883832488653741 ) ) ;
#111745 = ORIENTED_EDGE ( 'NONE', *, *, #56839, .F. ) ;
#111746 = DIRECTION ( 'NONE',  ( 0.000000000000000000, 1.000000000000000000, 0.000000000000000000 ) ) ;
#111747 = VECTOR ( 'NONE', #22788, 1000.000000000000000 ) ;
#111748 = ORIENTED_EDGE ( 'NONE', *, *, #71402, .T. ) ;
#111749 = AXIS2_PLACEMENT_3D ( 'NONE', #86469, #55727, #116570 ) ;
#111750 = VECTOR ( 'NONE', #34263, 1000.000000000000000 ) ;
#111751 = ORIENTED_EDGE ( 'NONE', *, *, #73766, .T. ) ;
#111752 = EDGE_LOOP ( 'NONE', ( #17279, #88034, #113476, #7846 ) ) ;
#111753 = CARTESIAN_POINT ( 'NONE',  ( 2.899999999999945732, 12.50000000000000000, -4.395220292106239768 ) ) ;
#111754 = AXIS2_PLACEMENT_3D ( 'NONE', #126322, #28775, #107318 ) ;
#111755 = DIRECTION ( 'NONE',  ( -0.000000000000000000, 1.000000000000000000, -0.000000000000000000 ) ) ;
#111756 = EDGE_LOOP ( 'NONE', ( #38450, #75014, #48800, #49348 ) ) ;
#111757 = DIRECTION ( 'NONE',  ( -0.000000000000000000, 1.000000000000000000, -0.000000000000000000 ) ) ;
#111758 = AXIS2_PLACEMENT_3D ( 'NONE', #109881, #60154, #82366 ) ;
#111759 = CIRCLE ( 'NONE', #86715, 2.000000000000000000 ) ;
#111760 = CARTESIAN_POINT ( 'NONE',  ( 0.000000000000000000, 12.50000000000000000, 0.000000000000000000 ) ) ;
#111762 = EDGE_CURVE ( 'NONE', #51026, #71846, #11752, .T. ) ;
#111761 = DIRECTION ( 'NONE',  ( 0.000000000000000000, 0.000000000000000000, 1.000000000000000000 ) ) ;
#111763 = DIRECTION ( 'NONE',  ( -0.000000000000000000, -1.000000000000000000, -0.000000000000000000 ) ) ;
#111764 = CARTESIAN_POINT ( 'NONE',  ( 186.8229166673494319, -4.445597072760122614, 7.699999999999998401 ) ) ;
#111766 = VERTEX_POINT ( 'NONE', #39940 ) ;
#111765 = CIRCLE ( 'NONE', #86717, 0.06509327318403745899 ) ;
#111767 = FACE_OUTER_BOUND ( 'NONE', #77885, .T. ) ;
#111768 = ORIENTED_EDGE ( 'NONE', *, *, #63280, .F. ) ;
#111769 = CARTESIAN_POINT ( 'NONE',  ( -4.400000000000025224, 12.50000000000000000, 3.983716857408420076 ) ) ;
#111770 = EDGE_CURVE ( 'NONE', #31773, #120101, #1253, .T. ) ;
#111771 = ORIENTED_EDGE ( 'NONE', *, *, #118745, .F. ) ;
#111772 = CARTESIAN_POINT ( 'NONE',  ( -9.400000000000007461, 2.500000000000000000, 4.576537180435972019 ) ) ;
#111773 = EDGE_LOOP ( 'NONE', ( #14796, #3552 ) ) ;
#111774 = CARTESIAN_POINT ( 'NONE',  ( -8.150000000000012790, 2.500000000000000000, 1.818653347947321475 ) ) ;
#111775 = DIRECTION ( 'NONE',  ( -0.000000000000000000, 1.000000000000000000, -0.000000000000000000 ) ) ;
#111776 = EDGE_CURVE ( 'NONE', #78026, #116101, #78640, .T. ) ;
#111777 = DIRECTION ( 'NONE',  ( 0.000000000000000000, 0.000000000000000000, -1.000000000000000000 ) ) ;
#111779 = ADVANCED_FACE ( 'NONE', ( #100757 ), #24157, .T. ) ;
#111778 = CARTESIAN_POINT ( 'NONE',  ( -5.600000000000023626, 2.500000000000000000, -3.883716857408426648 ) ) ;
#111780 = EDGE_CURVE ( 'NONE', #20674, #97708, #32060, .T. ) ;
#111781 = FACE_OUTER_BOUND ( 'NONE', #120930, .T. ) ;
#111782 = EDGE_CURVE ( 'NONE', #60985, #49812, #22202, .T. ) ;
#111783 = VECTOR ( 'NONE', #59354, 1000.000000000000000 ) ;
#111784 = ORIENTED_EDGE ( 'NONE', *, *, #90940, .F. ) ;
#111785 = ORIENTED_EDGE ( 'NONE', *, *, #102423, .F. ) ;
#111786 = FACE_OUTER_BOUND ( 'NONE', #39182, .T. ) ;
#111787 = CARTESIAN_POINT ( 'NONE',  ( 3.299999999999944755, 12.50000000000000000, -2.385244779468109755E-15 ) ) ;
#111788 = EDGE_CURVE ( 'NONE', #121167, #127574, #71980, .T. ) ;
#111789 = CARTESIAN_POINT ( 'NONE',  ( 6.649999999999930189, 2.500000000000000000, -2.857883832488653741 ) ) ;
#111791 = EDGE_LOOP ( 'NONE', ( #47040, #26100 ) ) ;
#111790 = ORIENTED_EDGE ( 'NONE', *, *, #106328, .F. ) ;
#111792 = ORIENTED_EDGE ( 'NONE', *, *, #101028, .F. ) ;
#111793 = ADVANCED_FACE ( 'NONE', ( #13673 ), #61994, .T. ) ;
#111794 = LINE ( 'NONE', #21472, #93785 ) ;
#111795 = ORIENTED_EDGE ( 'NONE', *, *, #39862, .T. ) ;
#111796 = DIRECTION ( 'NONE',  ( -0.000000000000000000, -1.000000000000000000, -0.000000000000000000 ) ) ;
#111798 = CONICAL_SURFACE ( 'NONE', #88800, 0.1000000000000002554, 0.003490658503988666988 ) ;
#111797 = DIRECTION ( 'NONE',  ( 0.000000000000000000, -0.000000000000000000, 1.000000000000000000 ) ) ;
#111799 = EDGE_CURVE ( 'NONE', #87462, #105143, #89089, .T. ) ;
#111800 = ITEM_DEFINED_TRANSFORMATION ( 'NONE', 'NONE', #79772,  #108296 ) ;
#111801 = EDGE_CURVE ( 'NONE', #114386, #49349, #49485, .T. ) ;
#111802 = CYLINDRICAL_SURFACE ( 'NONE', #53268, 7.700000000000000178 ) ;
#111803 = ORIENTED_EDGE ( 'NONE', *, *, #104290, .T. ) ;
#111804 = CARTESIAN_POINT ( 'NONE',  ( -10.00000000000000533, 2.500000000000000000, -5.122947341949750211 ) ) ;
#111805 = DIRECTION ( 'NONE',  ( 0.000000000000000000, -0.9999939076577903929, 0.003490651415223739937 ) ) ;
#111806 = CARTESIAN_POINT ( 'NONE',  ( -4.550000000000026468, 2.500000000000000000, -6.395190528383301931 ) ) ;
#111807 = CARTESIAN_POINT ( 'NONE',  ( 1.049999999999954969, 2.500000000000000000, -6.941600689897077459 ) ) ;
#111809 = EDGE_CURVE ( 'NONE', #8589, #25026, #2552, .T. ) ;
#111808 = DIRECTION ( 'NONE',  ( 0.000000000000000000, 0.000000000000000000, 1.000000000000000000 ) ) ;
#111810 = EDGE_LOOP ( 'NONE', ( #29747, #27735 ) ) ;
#111811 = AXIS2_PLACEMENT_3D ( 'NONE', #108145, #27634, #67565 ) ;
#111812 = CARTESIAN_POINT ( 'NONE',  ( -1.224646799147353269E-17, 2.500000000000000000, -0.1000000000000000056 ) ) ;
#111814 = CIRCLE ( 'NONE', #80705, 0.06509327318403745899 ) ;
#111813 = CARTESIAN_POINT ( 'NONE',  ( 1.649999999999950617, 12.50000000000000000, 2.099970236277060032 ) ) ;
#111815 = ORIENTED_EDGE ( 'NONE', *, *, #38212, .F. ) ;
#111816 = ORIENTED_EDGE ( 'NONE', *, *, #29479, .F. ) ;
#111817 = CARTESIAN_POINT ( 'NONE',  ( 186.2552083336747444, 6.551208109652275624, -3.782341765624998686 ) ) ;
#111818 = PLANE ( 'NONE',  #34416 ) ;
#111819 = CARTESIAN_POINT ( 'NONE',  ( -7.100000000000017408, 2.500000000000000000, -3.737306695894649700 ) ) ;
#111820 = DIRECTION ( 'NONE',  ( -0.000000000000000000, 1.000000000000000000, -0.000000000000000000 ) ) ;
#111821 = DIRECTION ( 'NONE',  ( -0.000000000000000000, -1.000000000000000000, -0.000000000000000000 ) ) ;
#111822 = CARTESIAN_POINT ( 'NONE',  ( 0.8499999999999553468, 12.50000000000000000, 2.099970236277060032 ) ) ;
#111823 = CONICAL_SURFACE ( 'NONE', #44920, 0.09999999999999982514, 0.003490658503988666988 ) ;
#111824 = DIRECTION ( 'NONE',  ( 0.000000000000000000, 1.000000000000000000, 0.000000000000000000 ) ) ;
#111825 = CARTESIAN_POINT ( 'NONE',  ( -14.59999999999998366, 12.50000000000000000, -1.084202172485504434E-16 ) ) ;
#111826 = CIRCLE ( 'NONE', #34180, 0.06509327318403745899 ) ;
#111827 = AXIS2_PLACEMENT_3D ( 'NONE', #61832, #110268, #81463 ) ;
#111828 = DIRECTION ( 'NONE',  ( 0.000000000000000000, 1.000000000000000000, 0.000000000000000000 ) ) ;
#111829 = ORIENTED_EDGE ( 'NONE', *, *, #84010, .F. ) ;
#111830 = VERTEX_POINT ( 'NONE', #41876 ) ;
#111831 = VERTEX_POINT ( 'NONE', #1922 ) ;
#111832 = ORIENTED_EDGE ( 'NONE', *, *, #16590, .T. ) ;
#111833 = CARTESIAN_POINT ( 'NONE',  ( -6.250000000000015987, 2.500000000000000000, 5.902370205355745192 ) ) ;
#111834 = DIRECTION ( 'NONE',  ( 0.000000000000000000, 1.000000000000000000, 0.000000000000000000 ) ) ;
#111835 = ORIENTED_EDGE ( 'NONE', *, *, #106173, .F. ) ;
#111836 = DIRECTION ( 'NONE',  ( 0.000000000000000000, 1.000000000000000000, 0.000000000000000000 ) ) ;
#111837 = EDGE_CURVE ( 'NONE', #54722, #36055, #64040, .T. ) ;
#111838 = CONICAL_SURFACE ( 'NONE', #76241, 0.09999999999999999167, 0.003490658503988666988 ) ;
#111839 = CIRCLE ( 'NONE', #7353, 2.318304356886072615 ) ;
#111840 = EDGE_CURVE ( 'NONE', #6241, #111738, #112164, .T. ) ;
#111841 = PLANE ( 'NONE',  #9627 ) ;
#111843 = ORIENTED_EDGE ( 'NONE', *, *, #29474, .F. ) ;
#111842 = CARTESIAN_POINT ( 'NONE',  ( 184.5166856079987667, -1.553938115584203139, -7.699999999999964650 ) ) ;
#111844 = AXIS2_PLACEMENT_3D ( 'NONE', #112743, #121908, #74104 ) ;
#111845 = CARTESIAN_POINT ( 'NONE',  ( 0.4499999999999569344, 2.500000000000000000, -2.065063509461102065 ) ) ;
#111846 = CARTESIAN_POINT ( 'NONE',  ( -2.900000000000029221, 2.500000000000000000, -0.1000000000000022815 ) ) ;
#111847 = ORIENTED_EDGE ( 'NONE', *, *, #67135, .F. ) ;
#111848 = AXIS2_PLACEMENT_3D ( 'NONE', #82349, #84250, #74447 ) ;
#111849 = AXIS2_PLACEMENT_3D ( 'NONE', #65384, #14342, #36604 ) ;
#111850 = CIRCLE ( 'NONE', #97174, 0.09999999999999982514 ) ;
#111851 = ORIENTED_EDGE ( 'NONE', *, *, #99977, .T. ) ;
#111852 = ORIENTED_EDGE ( 'NONE', *, *, #74519, .T. ) ;
#111853 = VERTEX_POINT ( 'NONE', #102699 ) ;
#111854 = PLANE ( 'NONE',  #115765 ) ;
#111855 = VECTOR ( 'NONE', #8305, 1000.000000000000000 ) ;
#111856 = CARTESIAN_POINT ( 'NONE',  ( -8.750000000000010658, 2.500000000000000000, -1.472243186433550122 ) ) ;
#111857 = CARTESIAN_POINT ( 'NONE',  ( 7.099999999999928590, 12.50000000000000000, -5.088040615133791356 ) ) ;
#111858 = VECTOR ( 'NONE', #128172, 1000.000000000000000 ) ;
#111859 = ORIENTED_EDGE ( 'NONE', *, *, #11788, .T. ) ;
#111861 = AXIS2_PLACEMENT_3D ( 'NONE', #121463, #71739, #54498 ) ;
#111860 = CARTESIAN_POINT ( 'NONE',  ( -10.60000000000000142, 12.50000000000000000, 0.3464101615137736845 ) ) ;
#111862 = EDGE_LOOP ( 'NONE', ( #81927, #105780 ) ) ;
#111863 = FACE_OUTER_BOUND ( 'NONE', #113619, .T. ) ;
#111864 = CARTESIAN_POINT ( 'NONE',  ( -12.29999999999999716, 12.50000000000000000, 0.3464101615137776813 ) ) ;
#111865 = DIRECTION ( 'NONE',  ( -0.000000000000000000, 1.000000000000000000, -0.000000000000000000 ) ) ;
#111866 = FACE_OUTER_BOUND ( 'NONE', #51982, .T. ) ;
#111867 = ORIENTED_EDGE ( 'NONE', *, *, #28964, .F. ) ;
#111868 = EDGE_LOOP ( 'NONE', ( #103341, #87687, #90345, #68648 ) ) ;
#111869 = ORIENTED_EDGE ( 'NONE', *, *, #74116, .F. ) ;
#111870 = DIRECTION ( 'NONE',  ( 0.000000000000000000, 0.000000000000000000, 1.000000000000000000 ) ) ;
#111871 = CARTESIAN_POINT ( 'NONE',  ( 12.09999999999990550, 12.50000000000000000, -3.572213422710612374 ) ) ;
#111872 = CARTESIAN_POINT ( 'NONE',  ( -4.999999999999990230, 2.500000000000000000, -4.430127018922202176 ) ) ;
#111873 = FACE_BOUND ( 'NONE', #5539, .T. ) ;
#111874 = CARTESIAN_POINT ( 'NONE',  ( 11.64999999999990443, 2.500000000000000000, 1.472243186433545459 ) ) ;
#111875 = CONICAL_SURFACE ( 'NONE', #67942, 0.09999999999999982514, 0.003490658503988666988 ) ;
#111876 = DIRECTION ( 'NONE',  ( 0.000000000000000000, -0.9999939076577903929, 0.003490651415223739937 ) ) ;
#111877 = FACE_OUTER_BOUND ( 'NONE', #47147, .T. ) ;
#111878 = EDGE_CURVE ( 'NONE', #46373, #28259, #116348, .T. ) ;
#111879 = DIRECTION ( 'NONE',  ( 0.000000000000000000, 0.000000000000000000, 1.000000000000000000 ) ) ;
#111880 = AXIS2_PLACEMENT_3D ( 'NONE', #115932, #103552, #63625 ) ;
#111881 = CARTESIAN_POINT ( 'NONE',  ( -1.650000000000034772, 12.50000000000000000, 1.407149913249508000 ) ) ;
#111882 = PLANE ( 'NONE',  #122171 ) ;
#111883 = ORIENTED_EDGE ( 'NONE', *, *, #113560, .F. ) ;
#111884 = AXIS2_PLACEMENT_3D ( 'NONE', #110300, #122066, #101776 ) ;
#111885 = AXIS2_PLACEMENT_3D ( 'NONE', #35115, #114927, #45570 ) ;
#111886 = DIRECTION ( 'NONE',  ( 0.000000000000000000, 0.000000000000000000, 1.000000000000000000 ) ) ;
#111887 = CARTESIAN_POINT ( 'NONE',  ( -4.350000000000023626, 2.500000000000000000, 6.148780366869520897 ) ) ;
#111888 = VERTEX_POINT ( 'NONE', #104005 ) ;
#111889 = ORIENTED_EDGE ( 'NONE', *, *, #87244, .T. ) ;
#111890 = EDGE_CURVE ( 'NONE', #87436, #39393, #103367, .T. ) ;
#111891 = DIRECTION ( 'NONE',  ( 0.000000000000000000, 1.000000000000000000, 0.000000000000000000 ) ) ;
#111893 = ADVANCED_FACE ( 'NONE', ( #4482 ), #66172, .T. ) ;
#111892 = CARTESIAN_POINT ( 'NONE',  ( 11.89999999999990798, 12.50000000000000000, 4.676537180435972552 ) ) ;
#111894 = FACE_BOUND ( 'NONE', #52612, .T. ) ;
#111895 = CARTESIAN_POINT ( 'NONE',  ( 2.499999999999948930, 12.50000000000000000, -5.022947341949754119 ) ) ;
#111896 = VECTOR ( 'NONE', #39446, 1000.000000000000000 ) ;
#111897 = AXIS2_PLACEMENT_3D ( 'NONE', #115090, #54901, #76494 ) ;
#111898 = EDGE_LOOP ( 'NONE', ( #82350, #68451, #106518, #94121 ) ) ;
#111899 = DIRECTION ( 'NONE',  ( -0.000000000000000000, 1.000000000000000000, -0.000000000000000000 ) ) ;
#111900 = ADVANCED_FACE ( 'NONE', ( #74541 ), #43224, .T. ) ;
#111901 = DIRECTION ( 'NONE',  ( 0.000000000000000000, 0.000000000000000000, 1.000000000000000000 ) ) ;
#111902 = EDGE_LOOP ( 'NONE', ( #113609, #112027 ) ) ;
#111903 = LINE ( 'NONE', #71315, #107553 ) ;
#111904 = CARTESIAN_POINT ( 'NONE',  ( 186.6562500006828031, 8.891194145520236347, 5.444286225454521982E-16 ) ) ;
#111905 = AXIS2_PLACEMENT_3D ( 'NONE', #38324, #80827, #109638 ) ;
#111906 = AXIS2_PLACEMENT_3D ( 'NONE', #68272, #108198, #66972 ) ;
#111907 = ORIENTED_EDGE ( 'NONE', *, *, #12285, .F. ) ;
#111908 = DIRECTION ( 'NONE',  ( 0.000000000000000000, -0.9999939076577903929, 0.003490651415223739937 ) ) ;
#111909 = DIRECTION ( 'NONE',  ( 0.000000000000000000, 1.000000000000000000, 0.000000000000000000 ) ) ;
#111910 = ORIENTED_EDGE ( 'NONE', *, *, #19449, .T. ) ;
#111911 = DIRECTION ( 'NONE',  ( 0.000000000000000000, -0.9999939076577903929, 0.003490651415223739937 ) ) ;
#111912 = DIRECTION ( 'NONE',  ( 0.000000000000000000, -0.9999939076577903929, 0.003490651415223739937 ) ) ;
#111913 = AXIS2_PLACEMENT_3D ( 'NONE', #94699, #104520, #62684 ) ;
#111914 = DIRECTION ( 'NONE',  ( -0.000000000000000000, 1.000000000000000000, -0.000000000000000000 ) ) ;
#111915 = ORIENTED_EDGE ( 'NONE', *, *, #13553, .T. ) ;
#111916 = ORIENTED_EDGE ( 'NONE', *, *, #91412, .F. ) ;
#111917 = DIRECTION ( 'NONE',  ( 0.000000000000000000, -0.9999939076577903929, 0.003490651415223739937 ) ) ;
#111918 = CONICAL_SURFACE ( 'NONE', #5289, 0.09999999999999982514, 0.003490658503988666988 ) ;
#111919 = ORIENTED_EDGE ( 'NONE', *, *, #62715, .F. ) ;
#111920 = DIRECTION ( 'NONE',  ( -0.000000000000000000, 1.000000000000000000, -0.000000000000000000 ) ) ;
#111921 = CARTESIAN_POINT ( 'NONE',  ( -7.500000000000001776, 2.500000000000000000, 9.000000000000001776 ) ) ;
#111922 = EDGE_CURVE ( 'NONE', #113276, #29766, #30609, .T. ) ;
#111924 = DIRECTION ( 'NONE',  ( 0.000000000000000000, 0.000000000000000000, -1.000000000000000000 ) ) ;
#111923 = AXIS2_PLACEMENT_3D ( 'NONE', #91299, #121401, #71025 ) ;
#111925 = VERTEX_POINT ( 'NONE', #114457 ) ;
#111926 = AXIS2_PLACEMENT_3D ( 'NONE', #102961, #121973, #12642 ) ;
#111927 = FACE_OUTER_BOUND ( 'NONE', #102922, .T. ) ;
#111928 = DIRECTION ( 'NONE',  ( -0.000000000000000000, 1.000000000000000000, -0.000000000000000000 ) ) ;
#111929 = DIRECTION ( 'NONE',  ( 0.000000000000000000, 1.000000000000000000, 0.000000000000000000 ) ) ;
#111930 = CARTESIAN_POINT ( 'NONE',  ( -11.84999999999999609, 2.500000000000000000, 2.611473670974873151 ) ) ;
#111931 = DIRECTION ( 'NONE',  ( -0.000000000000000000, -1.000000000000000000, -0.000000000000000000 ) ) ;
#111932 = EDGE_CURVE ( 'NONE', #29267, #2432, #18055, .T. ) ;
#111933 = FACE_OUTER_BOUND ( 'NONE', #80749, .T. ) ;
#111934 = EDGE_CURVE ( 'NONE', #64926, #55907, #110022, .T. ) ;
#111935 = CONICAL_SURFACE ( 'NONE', #28309, 0.1000000000000000472, 0.003490658503988666988 ) ;
#111936 = ORIENTED_EDGE ( 'NONE', *, *, #97903, .F. ) ;
#111938 = ORIENTED_EDGE ( 'NONE', *, *, #79445, .F. ) ;
#111937 = AXIS2_PLACEMENT_3D ( 'NONE', #119635, #29995, #69912 ) ;
#111940 = PLANE ( 'NONE',  #45369 ) ;
#111939 = AXIS2_PLACEMENT_3D ( 'NONE', #114063, #64307, #25671 ) ;
#111941 = VERTEX_POINT ( 'NONE', #84361 ) ;
#111942 = LINE ( 'NONE', #32104, #57712 ) ;
#111943 = EDGE_CURVE ( 'NONE', #112113, #64505, #64712, .T. ) ;
#111946 = ORIENTED_EDGE ( 'NONE', *, *, #25908, .T. ) ;
#111945 = ORIENTED_EDGE ( 'NONE', *, *, #23690, .T. ) ;
#111944 = CIRCLE ( 'NONE', #26261, 0.1000000000000002554 ) ;
#111947 = EDGE_CURVE ( 'NONE', #5078, #119339, #99641, .T. ) ;
#111948 = EDGE_LOOP ( 'NONE', ( #90769, #42301, #117292, #83744 ) ) ;
#111949 = EDGE_CURVE ( 'NONE', #96192, #94402, #59959, .T. ) ;
#111950 = CARTESIAN_POINT ( 'NONE',  ( -3.150000000000030109, 2.500000000000000000, -2.511473670974877948 ) ) ;
#111951 = ADVANCED_FACE ( 'NONE', ( #86928 ), #15605, .T. ) ;
#111952 = AXIS2_PLACEMENT_3D ( 'NONE', #100533, #52097, #22645 ) ;
#111954 = CONICAL_SURFACE ( 'NONE', #101486, 0.1000000000000002554, 0.003490658503988666988 ) ;
#111953 = DIRECTION ( 'NONE',  ( 0.000000000000000000, 0.000000000000000000, 1.000000000000000000 ) ) ;
#111955 = FACE_OUTER_BOUND ( 'NONE', #108285, .T. ) ;
#111956 =( NAMED_UNIT ( * ) SI_UNIT ( $, .STERADIAN. ) SOLID_ANGLE_UNIT ( ) );
#111957 = EDGE_CURVE ( 'NONE', #15249, #13248, #126741, .T. ) ;
#111958 = DIRECTION ( 'NONE',  ( -0.000000000000000000, 1.000000000000000000, -0.000000000000000000 ) ) ;
#111959 = CARTESIAN_POINT ( 'NONE',  ( -0.8000000000000381251, 2.500000000000000000, 4.430127018922196847 ) ) ;
#111960 = CARTESIAN_POINT ( 'NONE',  ( 21.25101261094843963, 0.2446824650187501560, 4.189229355218854423 ) ) ;
#111961 = CIRCLE ( 'NONE', #103636, 0.1000000000000000472 ) ;
#111962 = DIRECTION ( 'NONE',  ( 0.000000000000000000, 0.000000000000000000, 1.000000000000000000 ) ) ;
#111963 = DIRECTION ( 'NONE',  ( -0.000000000000000000, -1.000000000000000000, -0.000000000000000000 ) ) ;
#111965 = EDGE_CURVE ( 'NONE', #112226, #70902, #67256, .T. ) ;
#111964 = FACE_OUTER_BOUND ( 'NONE', #17200, .T. ) ;
#111966 = ORIENTED_EDGE ( 'NONE', *, *, #13066, .T. ) ;
#111967 = DIRECTION ( 'NONE',  ( -0.000000000000000000, 1.000000000000000000, -0.000000000000000000 ) ) ;
#111968 = VERTEX_POINT ( 'NONE', #126219 ) ;
#111969 = EDGE_LOOP ( 'NONE', ( #18679, #75357, #109901, #51559 ) ) ;
#111970 = CARTESIAN_POINT ( 'NONE',  ( -10.20000000000000639, 2.500000000000000000, -3.983716857408421852 ) ) ;
#111971 = CARTESIAN_POINT ( 'NONE',  ( -7.950000000000012612, 12.50000000000000000, 2.165063509461097713 ) ) ;
#111972 = AXIS2_PLACEMENT_3D ( 'NONE', #57662, #95646, #76652 ) ;
#111973 = CARTESIAN_POINT ( 'NONE',  ( -3.350000000000028511, 2.500000000000000000, 2.957883832488649389 ) ) ;
#111974 = DIRECTION ( 'NONE',  ( 0.000000000000000000, 1.000000000000000000, 0.000000000000000000 ) ) ;
#111976 = CARTESIAN_POINT ( 'NONE',  ( 4.599999999999940137, 12.50000000000000000, -4.395220292106239768 ) ) ;
#111975 = PRODUCT ( 'coupler', 'coupler', '', ( #76537 ) ) ;
#111977 = CARTESIAN_POINT ( 'NONE',  ( 0.8499999999999536815, 2.500000000000000000, 6.495190528383297135 ) ) ;
#111978 = DIRECTION ( 'NONE',  ( 0.000000000000000000, 0.000000000000000000, 1.000000000000000000 ) ) ;
#111979 = ORIENTED_EDGE ( 'NONE', *, *, #52839, .T. ) ;
#111980 = AXIS2_PLACEMENT_3D ( 'NONE', #18370, #36749, #87748 ) ;
#111981 = AXIS2_PLACEMENT_3D ( 'NONE', #91280, #2910, #3544 ) ;
#111982 = AXIS2_PLACEMENT_3D ( 'NONE', #84830, #26567, #75022 ) ;
#111983 = ORIENTED_EDGE ( 'NONE', *, *, #44435, .T. ) ;
#111984 = ORIENTED_EDGE ( 'NONE', *, *, #152, .F. ) ;
#111985 = AXIS2_PLACEMENT_3D ( 'NONE', #27039, #66938, #106864 ) ;
#111986 = ORIENTED_EDGE ( 'NONE', *, *, #25487, .T. ) ;
#111987 = ORIENTED_EDGE ( 'NONE', *, *, #68372, .T. ) ;
#111988 = FACE_OUTER_BOUND ( 'NONE', #52541, .T. ) ;
#111989 = CARTESIAN_POINT ( 'NONE',  ( -6.650000000000015454, 12.50000000000000000, 2.857883832488649301 ) ) ;
#111990 = CIRCLE ( 'NONE', #91052, 0.1000000000000002554 ) ;
#111991 = FACE_OUTER_BOUND ( 'NONE', #7437, .T. ) ;
#111992 = ADVANCED_FACE ( 'NONE', ( #76484 ), #35279, .T. ) ;
#111993 = DIRECTION ( 'NONE',  ( 0.000000000000000000, 0.000000000000000000, 1.000000000000000000 ) ) ;
#111994 = AXIS2_PLACEMENT_3D ( 'NONE', #10323, #1144, #40449 ) ;
#111995 = DIRECTION ( 'NONE',  ( 0.000000000000000000, -0.9999939076577903929, 0.003490651415223739937 ) ) ;
#111996 = ORIENTED_EDGE ( 'NONE', *, *, #80313, .F. ) ;
#111997 = CARTESIAN_POINT ( 'NONE',  ( 2.099999999999950351, 12.50000000000000000, 0.06509327318403515528 ) ) ;
#111998 = DIRECTION ( 'NONE',  ( 0.000000000000000000, 1.000000000000000000, 0.000000000000000000 ) ) ;
#111999 = DIRECTION ( 'NONE',  ( -0.000000000000000000, 1.000000000000000000, -0.000000000000000000 ) ) ;
#112000 = DIRECTION ( 'NONE',  ( -4.274815082592931898E-19, -0.9999939076577903929, -0.003490651415223739937 ) ) ;
#112002 = EDGE_CURVE ( 'NONE', #76525, #90431, #55711, .T. ) ;
#112001 = DIRECTION ( 'NONE',  ( 0.000000000000000000, 0.000000000000000000, 1.000000000000000000 ) ) ;
#112003 = VERTEX_POINT ( 'NONE', #36571 ) ;
#112004 = AXIS2_PLACEMENT_3D ( 'NONE', #117320, #85319, #85946 ) ;
#112005 = AXIS2_PLACEMENT_3D ( 'NONE', #50569, #112082, #110144 ) ;
#112006 = EDGE_LOOP ( 'NONE', ( #110201, #19151, #8829, #92968 ) ) ;
#112007 = EDGE_LOOP ( 'NONE', ( #79512, #65820, #90799, #13129 ) ) ;
#112008 = DIRECTION ( 'NONE',  ( -0.000000000000000000, -1.000000000000000000, -0.000000000000000000 ) ) ;
#112009 = EDGE_LOOP ( 'NONE', ( #99456, #110350, #75670, #82529 ) ) ;
#112010 = CARTESIAN_POINT ( 'NONE',  ( -5.800000000000018474, 2.500000000000000000, 4.330127018922196314 ) ) ;
#112011 = DIRECTION ( 'NONE',  ( 0.000000000000000000, 1.000000000000000000, 0.000000000000000000 ) ) ;
#112012 = VERTEX_POINT ( 'NONE', #116383 ) ;
#112013 = CARTESIAN_POINT ( 'NONE',  ( 15.39999999999989200, 2.500000000000000000, 0.7928203230275495672 ) ) ;
#112014 = DIRECTION ( 'NONE',  ( 0.000000000000000000, 0.000000000000000000, -1.000000000000000000 ) ) ;
#112015 = CARTESIAN_POINT ( 'NONE',  ( 184.4999999999999716, -6.820224004183075728, 3.418167119943706034 ) ) ;
#112016 = CARTESIAN_POINT ( 'NONE',  ( 9.399999999999915090, 2.500000000000000000, 4.083716857408421497 ) ) ;
#112017 = CIRCLE ( 'NONE', #26247, 0.1000000000000000472 ) ;
#112018 = CARTESIAN_POINT ( 'NONE',  ( 12.09999999999990550, 2.500000000000000000, 4.330127018922196314 ) ) ;
#112019 = CIRCLE ( 'NONE', #15761, 0.06509327318403745899 ) ;
#112020 = ORIENTED_EDGE ( 'NONE', *, *, #111024, .F. ) ;
#112021 = ORIENTED_EDGE ( 'NONE', *, *, #70738, .F. ) ;
#112022 = CARTESIAN_POINT ( 'NONE',  ( 15.39999999999989200, 12.50000000000000000, 0.6928203230275494784 ) ) ;
#112023 = CARTESIAN_POINT ( 'NONE',  ( 4.149999999999939959, 2.500000000000000000, 1.572243186433545548 ) ) ;
#112024 = CARTESIAN_POINT ( 'NONE',  ( -10.85000000000000142, 12.50000000000000000, -7.188010851410850499 ) ) ;
#112025 = CARTESIAN_POINT ( 'NONE',  ( -1.850000000000033840, 12.50000000000000000, 1.753560074763284016 ) ) ;
#112026 = EDGE_CURVE ( 'NONE', #40133, #4247, #47320, .T. ) ;
#112027 = ORIENTED_EDGE ( 'NONE', *, *, #18385, .T. ) ;
#112028 = CIRCLE ( 'NONE', #74371, 0.06509327318403745899 ) ;
#112029 = EDGE_LOOP ( 'NONE', ( #86562, #24768 ) ) ;
#112030 = CARTESIAN_POINT ( 'NONE',  ( -10.85000000000000142, 2.500000000000000000, -1.472243186433546125 ) ) ;
#112031 = DIRECTION ( 'NONE',  ( 0.000000000000000000, 0.000000000000000000, 1.000000000000000000 ) ) ;
#112032 = FACE_OUTER_BOUND ( 'NONE', #53383, .T. ) ;
#112033 = PLANE ( 'NONE',  #61450 ) ;
#112034 = EDGE_LOOP ( 'NONE', ( #53484, #69555, #92841, #21607 ) ) ;
#112035 = CONICAL_SURFACE ( 'NONE', #55597, 0.09999999999999982514, 0.003490658503988666988 ) ;
#112036 = ADVANCED_FACE ( 'NONE', ( #37207 ), #5533, .T. ) ;
#112037 = DIRECTION ( 'NONE',  ( 0.000000000000000000, 0.000000000000000000, -1.000000000000000000 ) ) ;
#112038 = CONICAL_SURFACE ( 'NONE', #32649, 0.1000000000000000472, 0.003490658503988666988 ) ;
#112039 = DIRECTION ( 'NONE',  ( 0.000000000000000000, 0.000000000000000000, 1.000000000000000000 ) ) ;
#112040 = CIRCLE ( 'NONE', #116042, 0.09999999999999982514 ) ;
#112041 = ORIENTED_EDGE ( 'NONE', *, *, #77361, .F. ) ;
#112042 = EDGE_CURVE ( 'NONE', #42690, #62384, #66005, .T. ) ;
#112043 = CARTESIAN_POINT ( 'NONE',  ( 12.29999999999990123, 2.500000000000000000, 0.3464101615137735735 ) ) ;
#112044 = ADVANCED_FACE ( 'NONE', ( #94825 ), #16868, .F. ) ;
#112045 = EDGE_LOOP ( 'NONE', ( #94705, #122406, #94873, #49504 ) ) ;
#112046 = CARTESIAN_POINT ( 'NONE',  ( 9.149999999999918643, 12.50000000000000000, -6.430097255199264339 ) ) ;
#112047 = ORIENTED_EDGE ( 'NONE', *, *, #78371, .F. ) ;
#112048 = FACE_OUTER_BOUND ( 'NONE', #83660, .T. ) ;
#112049 = CARTESIAN_POINT ( 'NONE',  ( 10.84999999999990905, 2.500000000000000000, 2.857883832488649301 ) ) ;
#112050 = EDGE_CURVE ( 'NONE', #104598, #63506, #118412, .T. ) ;
#112051 = ORIENTED_EDGE ( 'NONE', *, *, #46314, .T. ) ;
#112052 = ORIENTED_EDGE ( 'NONE', *, *, #80567, .T. ) ;
#112053 = EDGE_CURVE ( 'NONE', #93285, #79041, #24327, .T. ) ;
#112054 = CARTESIAN_POINT ( 'NONE',  ( 14.34999999999989306, 2.500000000000000000, -1.918653347947326004 ) ) ;
#112055 = CARTESIAN_POINT ( 'NONE',  ( 13.09999999999989839, 2.500000000000000000, -0.4464101615137783252 ) ) ;
#112056 = CIRCLE ( 'NONE', #91121, 0.09999999999999982514 ) ;
#112057 = CARTESIAN_POINT ( 'NONE',  ( -14.14999999999998792, 12.50000000000000000, -1.407149913249510442 ) ) ;
#112058 = CARTESIAN_POINT ( 'NONE',  ( 184.9843750003414016, -8.734944146203032389, -1.604583208406767949E-15 ) ) ;
#112059 = CARTESIAN_POINT ( 'NONE',  ( -6.650000000000018119, 12.50000000000000000, -7.188010851410854052 ) ) ;
#112060 = PLANE ( 'NONE',  #15901 ) ;
#112061 = CARTESIAN_POINT ( 'NONE',  ( -7.050000000000013145, 12.50000000000000000, 2.165063509461097713 ) ) ;
#112062 = LINE ( 'NONE', #22408, #51527 ) ;
#112063 = DIRECTION ( 'NONE',  ( 0.000000000000000000, -0.000000000000000000, 1.000000000000000000 ) ) ;
#112064 = CONICAL_SURFACE ( 'NONE', #72365, 0.1000000000000000472, 0.003490658503988666988 ) ;
#112065 = VECTOR ( 'NONE', #18674, 1000.000000000000000 ) ;
#112066 = ORIENTED_EDGE ( 'NONE', *, *, #100229, .F. ) ;
#112067 = ORIENTED_EDGE ( 'NONE', *, *, #129238, .T. ) ;
#112068 = CARTESIAN_POINT ( 'NONE',  ( 6.049999999999932321, 2.500000000000000000, 6.841600689897072485 ) ) ;
#112069 = ORIENTED_EDGE ( 'NONE', *, *, #27275, .F. ) ;
#112070 = CARTESIAN_POINT ( 'NONE',  ( 9.199999999999915801, 2.500000000000000000, 4.230127018922196669 ) ) ;
#112071 = CARTESIAN_POINT ( 'NONE',  ( -10.20000000000000462, 12.50000000000000000, 0.3464101615137735735 ) ) ;
#112072 = FACE_OUTER_BOUND ( 'NONE', #109106, .T. ) ;
#112074 = ORIENTED_EDGE ( 'NONE', *, *, #29784, .T. ) ;
#112073 = ORIENTED_EDGE ( 'NONE', *, *, #58101, .F. ) ;
#112075 = FACE_BOUND ( 'NONE', #85933, .T. ) ;
#112076 = ORIENTED_EDGE ( 'NONE', *, *, #89472, .F. ) ;
#112077 = CARTESIAN_POINT ( 'NONE',  ( -11.84999999999999609, 2.500000000000000000, 1.818653347947321475 ) ) ;
#112078 = CARTESIAN_POINT ( 'NONE',  ( -6.250000000000019540, 12.50000000000000000, -7.253104124594891289 ) ) ;
#112079 = AXIS2_PLACEMENT_3D ( 'NONE', #5124, #5753, #115066 ) ;
#112080 = CARTESIAN_POINT ( 'NONE',  ( -5.850000000000021849, 2.500000000000000000, -7.088010851410853519 ) ) ;
#112081 = LINE ( 'NONE', #102264, #59784 ) ;
#112082 = DIRECTION ( 'NONE',  ( 0.000000000000000000, 1.000000000000000000, 0.000000000000000000 ) ) ;
#112084 = AXIS2_PLACEMENT_3D ( 'NONE', #97894, #76976, #48163 ) ;
#112083 = VECTOR ( 'NONE', #36618, 1000.000000000000000 ) ;
#112085 = DIRECTION ( 'NONE',  ( 0.000000000000000000, 0.000000000000000000, 1.000000000000000000 ) ) ;
#112086 = LINE ( 'NONE', #72807, #30983 ) ;
#112087 = DIRECTION ( 'NONE',  ( -4.274815082592931898E-19, -0.9999939076577903929, -0.003490651415223739937 ) ) ;
#112088 = DIRECTION ( 'NONE',  ( -0.000000000000000000, -1.000000000000000000, -0.000000000000000000 ) ) ;
#112089 = CARTESIAN_POINT ( 'NONE',  ( 11.84999999999990372, 2.500000000000000000, 1.718653347947321386 ) ) ;
#112090 = DIRECTION ( 'NONE',  ( 0.000000000000000000, -0.9999939076577903929, 0.003490651415223739937 ) ) ;
#112091 = ADVANCED_FACE ( 'NONE', ( #105935 ), #95437, .T. ) ;
#112092 = ORIENTED_EDGE ( 'NONE', *, *, #19555, .T. ) ;
#112093 = VERTEX_POINT ( 'NONE', #6407 ) ;
#112094 = ORIENTED_EDGE ( 'NONE', *, *, #118135, .T. ) ;
#112095 = DIRECTION ( 'NONE',  ( 1.000000000000000000, 0.000000000000000000, -1.776356839400246520E-15 ) ) ;
#112096 = EDGE_LOOP ( 'NONE', ( #123491, #62399 ) ) ;
#112097 = DIRECTION ( 'NONE',  ( 0.000000000000000000, 1.000000000000000000, 0.000000000000000000 ) ) ;
#112098 = ADVANCED_FACE ( 'NONE', ( #47297 ), #106832, .T. ) ;
#112099 = CARTESIAN_POINT ( 'NONE',  ( 6.899999999999928413, 2.500000000000000000, -4.083716857408426826 ) ) ;
#112100 = ADVANCED_FACE ( 'NONE', ( #107499 ), #57787, .T. ) ;
#112102 = VERTEX_POINT ( 'NONE', #56450 ) ;
#112101 = ORIENTED_EDGE ( 'NONE', *, *, #42393, .T. ) ;
#112103 = ORIENTED_EDGE ( 'NONE', *, *, #39930, .T. ) ;
#112104 = ADVANCED_FACE ( 'NONE', ( #7345 ), #34814, .T. ) ;
#112105 = CARTESIAN_POINT ( 'NONE',  ( 1.658312395177699017, -2.500000000000000444, -5.000000000000004441 ) ) ;
#112106 = EDGE_CURVE ( 'NONE', #79005, #10181, #106212, .T. ) ;
#112107 = DIRECTION ( 'NONE',  ( 0.000000000000000000, 1.000000000000000000, 0.000000000000000000 ) ) ;
#112108 = CARTESIAN_POINT ( 'NONE',  ( 2.899999999999944844, 2.500000000000000000, 4.922947341949748257 ) ) ;
#112109 = EDGE_CURVE ( 'NONE', #49224, #18575, #51529, .T. ) ;
#112110 = CARTESIAN_POINT ( 'NONE',  ( 32.27737261621599885, -1.406459146828822782, -4.686451385768223510 ) ) ;
#112111 = CARTESIAN_POINT ( 'NONE',  ( 185.3229166673494888, -4.445597072760063107, 7.700000000000102318 ) ) ;
#112112 = DIRECTION ( 'NONE',  ( 0.000000000000000000, 1.000000000000000000, 0.000000000000000000 ) ) ;
#112113 = VERTEX_POINT ( 'NONE', #57764 ) ;
#112115 = EDGE_CURVE ( 'NONE', #116826, #21551, #68233, .T. ) ;
#112114 = CARTESIAN_POINT ( 'NONE',  ( 6.449999999999931788, 2.500000000000000000, -6.248780366869526759 ) ) ;
#112116 = VERTEX_POINT ( 'NONE', #27624 ) ;
#112117 = EDGE_CURVE ( 'NONE', #16932, #9105, #28951, .T. ) ;
#112119 = EDGE_LOOP ( 'NONE', ( #127808, #127786, #88088, #74271 ) ) ;
#112118 = AXIS2_PLACEMENT_3D ( 'NONE', #32900, #112738, #100970 ) ;
#112120 = VERTEX_POINT ( 'NONE', #67550 ) ;
#112121 = CARTESIAN_POINT ( 'NONE',  ( -11.44999999999999751, 2.500000000000000000, 6.941600689897073018 ) ) ;
#112122 =( BOUNDED_SURFACE ( )  B_SPLINE_SURFACE ( 3, 2, ( 
 ( #8333, #67902, #117622 ),
 ( #27983, #28639, #18153 ),
 ( #111539, #58099, #2212 ),
 ( #109100, #39763, #89482 ),
 ( #9631, #98004, #12675 ),
 ( #38469, #112186, #119571 ),
 ( #98637, #79656, #118939 ),
 ( #8974, #48267, #42158 ),
 ( #71608, #122012, #118295 ),
 ( #82074, #88163, #52611 ),
 ( #21889, #61809, #88833 ),
 ( #48928, #29283, #101728 ),
 ( #49572, #12040, #62457 ),
 ( #128125, #128791, #72275 ) ),
 .UNSPECIFIED., .F., .F., .F. ) 
 B_SPLINE_SURFACE_WITH_KNOTS ( ( 4, 2, 2, 2, 2, 2, 4 ),
 ( 3, 3 ),
 ( 0.000000000000000000, 0.001744612550434158091, 0.002616918825651237245, 0.003489225100868316182, 0.005233837651302474490, 0.006106143926519553428, 0.006978450201736632365 ),
 ( 0.000000000000000000, 1.000000000000000000 ),
 .UNSPECIFIED. ) 
 GEOMETRIC_REPRESENTATION_ITEM ( )  RATIONAL_B_SPLINE_SURFACE ( (
 ( 1.000000000000000000, 0.7318752858502195480, 1.000000000000000000),
 ( 1.000000000000000000, 0.7270130115578816721, 1.000000000000000000),
 ( 1.000000000000000000, 0.7223762446139350146, 1.000000000000000000),
 ( 1.000000000000000000, 0.7156127915551184770, 1.000000000000000000),
 ( 1.000000000000000000, 0.7133893117691979535, 1.000000000000000000),
 ( 1.000000000000000000, 0.7090389252573886525, 1.000000000000000000),
 ( 1.000000000000000000, 0.7069297463491840405, 1.000000000000000000),
 ( 1.000000000000000000, 0.7010696893200119018, 1.000000000000000000),
 ( 1.000000000000000000, 0.6977361265598627238, 1.000000000000000000),
 ( 1.000000000000000000, 0.6948030504688554876, 1.000000000000000000),
 ( 1.000000000000000000, 0.6942033558615359201, 1.000000000000000000),
 ( 1.000000000000000000, 0.6937817651808704245, 1.000000000000000000),
 ( 1.000000000000000000, 0.6939284133496994578, 1.000000000000000000),
 ( 1.000000000000000000, 0.6944177883068215484, 1.000000000000000000) ) ) 
 REPRESENTATION_ITEM ( '' )  SURFACE ( )  );
#112123 = VERTEX_POINT ( 'NONE', #7995 ) ;
#112124 = EDGE_LOOP ( 'NONE', ( #117338, #67662 ) ) ;
#112125 = ORIENTED_EDGE ( 'NONE', *, *, #89059, .F. ) ;
#112126 = CARTESIAN_POINT ( 'NONE',  ( 5.399999999999935518, 2.500000000000000000, -4.330127018922201643 ) ) ;
#112128 = CIRCLE ( 'NONE', #32721, 0.06509327318403745899 ) ;
#112127 = CONICAL_SURFACE ( 'NONE', #128869, 0.09999999999999982514, 0.003490658503988666988 ) ;
#112129 = DIRECTION ( 'NONE',  ( -0.000000000000000000, 1.000000000000000000, -0.000000000000000000 ) ) ;
#112130 = DIRECTION ( 'NONE',  ( 0.000000000000000000, 1.000000000000000000, 0.000000000000000000 ) ) ;
#112131 = CARTESIAN_POINT ( 'NONE',  ( 11.44999999999991047, 2.500000000000000000, -2.411473670974877859 ) ) ;
#112132 = LINE ( 'NONE', #110821, #17732 ) ;
#112133 = DIRECTION ( 'NONE',  ( 0.000000000000000000, 0.000000000000000000, 1.000000000000000000 ) ) ;
#112134 = CARTESIAN_POINT ( 'NONE',  ( -8.300000000000011369, 12.50000000000000000, 0.06509327318403515528 ) ) ;
#112135 = VECTOR ( 'NONE', #68184, 1000.000000000000000 ) ;
#112136 = ORIENTED_EDGE ( 'NONE', *, *, #97152, .T. ) ;
#112137 = CARTESIAN_POINT ( 'NONE',  ( -2.100000000000033396, 12.50000000000000000, -4.957854068765716882 ) ) ;
#112138 = CONICAL_SURFACE ( 'NONE', #3465, 0.09999999999999982514, 0.003490658503988666988 ) ;
#112139 = ORIENTED_EDGE ( 'NONE', *, *, #1527, .T. ) ;
#112140 = FACE_OUTER_BOUND ( 'NONE', #127537, .T. ) ;
#112141 = VERTEX_POINT ( 'NONE', #98966 ) ;
#112142 = LINE ( 'NONE', #891, #73976 ) ;
#112143 = ORIENTED_EDGE ( 'NONE', *, *, #61643, .T. ) ;
#112144 = CARTESIAN_POINT ( 'NONE',  ( 183.9843750003414016, -8.734944146203032389, -1.604583208406768146E-15 ) ) ;
#112145 = CARTESIAN_POINT ( 'NONE',  ( -9.150000000000009237, 2.500000000000000000, 2.165063509461097713 ) ) ;
#112146 = VERTEX_POINT ( 'NONE', #8626 ) ;
#112147 = ORIENTED_EDGE ( 'NONE', *, *, #75856, .T. ) ;
#112148 = FACE_OUTER_BOUND ( 'NONE', #68696, .T. ) ;
#112149 = FACE_OUTER_BOUND ( 'NONE', #116357, .T. ) ;
#112150 = CARTESIAN_POINT ( 'NONE',  ( 6.899999999999928413, 12.50000000000000000, -4.676537180435977881 ) ) ;
#112151 = AXIS2_PLACEMENT_3D ( 'NONE', #9691, #110464, #49636 ) ;
#112152 = DIRECTION ( 'NONE',  ( -0.000000000000000000, -1.000000000000000000, -0.000000000000000000 ) ) ;
#112154 = EDGE_CURVE ( 'NONE', #103978, #74727, #43311, .T. ) ;
#112153 = CARTESIAN_POINT ( 'NONE',  ( -4.350000000000023626, 12.50000000000000000, -1.753560074763288457 ) ) ;
#112155 = VERTEX_POINT ( 'NONE', #108772 ) ;
#112156 = CONICAL_SURFACE ( 'NONE', #49474, 0.1000000000000000056, 0.003490658503988666988 ) ;
#112157 = CARTESIAN_POINT ( 'NONE',  ( 2.500000000000002220, -2.500000000000000000, 9.000000000000001776 ) ) ;
#112158 = AXIS2_PLACEMENT_3D ( 'NONE', #7099, #116410, #126897 ) ;
#112159 = AXIS2_PLACEMENT_3D ( 'NONE', #11912, #13839, #33509 ) ;
#112160 = ORIENTED_EDGE ( 'NONE', *, *, #10204, .T. ) ;
#112161 = AXIS2_PLACEMENT_3D ( 'NONE', #77439, #18517, #17193 ) ;
#112162 = DIRECTION ( 'NONE',  ( -4.274815082592931898E-19, -0.9999939076577903929, -0.003490651415223739937 ) ) ;
#112163 = FACE_OUTER_BOUND ( 'NONE', #52801, .T. ) ;
#112164 = CIRCLE ( 'NONE', #72452, 0.1000000000000002554 ) ;
#112165 = LINE ( 'NONE', #29733, #103997 ) ;
#112166 = CARTESIAN_POINT ( 'NONE',  ( -15.39999999999998082, 12.50000000000000000, 0.6928203230275518099 ) ) ;
#112167 = DIRECTION ( 'NONE',  ( -0.000000000000000000, 1.000000000000000000, -0.000000000000000000 ) ) ;
#112168 = LINE ( 'NONE', #103640, #62815 ) ;
#112169 = CARTESIAN_POINT ( 'NONE',  ( -10.85000000000000142, 12.50000000000000000, -2.857883832488649745 ) ) ;
#112170 = EDGE_LOOP ( 'NONE', ( #16639, #16506 ) ) ;
#112171 = AXIS2_PLACEMENT_3D ( 'NONE', #76785, #97699, #87866 ) ;
#112172 = DIRECTION ( 'NONE',  ( 0.000000000000000000, 0.000000000000000000, 1.000000000000000000 ) ) ;
#112174 = AXIS2_PLACEMENT_3D ( 'NONE', #85188, #125120, #95657 ) ;
#112173 = AXIS2_PLACEMENT_3D ( 'NONE', #60127, #28721, #99393 ) ;
#112175 = LINE ( 'NONE', #32984, #109134 ) ;
#112176 = DIRECTION ( 'NONE',  ( 0.000000000000000000, -0.9999939076577903929, 0.003490651415223739937 ) ) ;
#112177 = EDGE_LOOP ( 'NONE', ( #103918, #23712 ) ) ;
#112178 = ORIENTED_EDGE ( 'NONE', *, *, #36425, .F. ) ;
#112179 = CARTESIAN_POINT ( 'NONE',  ( -7.950000000000012612, 2.500000000000000000, 2.065063509461097624 ) ) ;
#112180 = ORIENTED_EDGE ( 'NONE', *, *, #108255, .F. ) ;
#112181 = ORIENTED_EDGE ( 'NONE', *, *, #78727, .F. ) ;
#112182 = LINE ( 'NONE', #74191, #82331 ) ;
#112183 = VERTEX_POINT ( 'NONE', #87840 ) ;
#112184 = DIRECTION ( 'NONE',  ( 0.000000000000000000, 0.000000000000000000, -1.000000000000000000 ) ) ;
#112185 = DIRECTION ( 'NONE',  ( 0.000000000000000000, -0.9999939076577903929, 0.003490651415223739937 ) ) ;
#112186 = CARTESIAN_POINT ( 'NONE',  ( 18.98912670146768633, 2.543039972612955335, 4.488908218018861973 ) ) ;
#112187 = EDGE_LOOP ( 'NONE', ( #89584, #120688, #127052, #11920 ) ) ;
#112188 = EDGE_CURVE ( 'NONE', #40568, #124666, #129000, .T. ) ;
#112189 = DIRECTION ( 'NONE',  ( 0.000000000000000000, 0.000000000000000000, 1.000000000000000000 ) ) ;
#112190 = LINE ( 'NONE', #93204, #91311 ) ;
#112191 = ADVANCED_FACE ( 'NONE', ( #96366 ), #91319, .T. ) ;
#112192 = ADVANCED_FACE ( 'NONE', ( #58414 ), #78821, .T. ) ;
#112193 = VERTEX_POINT ( 'NONE', #68205 ) ;
#112194 = VECTOR ( 'NONE', #58967, 1000.000000000000000 ) ;
#112195 = ORIENTED_EDGE ( 'NONE', *, *, #28854, .T. ) ;
#112196 = AXIS2_PLACEMENT_3D ( 'NONE', #24896, #115848, #113929 ) ;
#112197 = EDGE_LOOP ( 'NONE', ( #127533, #27554, #35795, #69184 ) ) ;
#112198 = CARTESIAN_POINT ( 'NONE',  ( -0.6500000000000398792, 2.500000000000000000, -6.841600689897078702 ) ) ;
#112199 = LINE ( 'NONE', #52625, #106397 ) ;
#112200 = EDGE_CURVE ( 'NONE', #90179, #39201, #110099, .T. ) ;
#112201 = EDGE_CURVE ( 'NONE', #46879, #71600, #46644, .T. ) ;
#112202 = DIRECTION ( 'NONE',  ( 0.000000000000000000, 0.000000000000000000, 1.000000000000000000 ) ) ;
#112203 = EDGE_CURVE ( 'NONE', #6770, #89861, #126827, .T. ) ;
#112204 = FACE_BOUND ( 'NONE', #43249, .T. ) ;
#112205 = ORIENTED_EDGE ( 'NONE', *, *, #117075, .T. ) ;
#112206 = EDGE_CURVE ( 'NONE', #84673, #20142, #88491, .T. ) ;
#112207 = FACE_OUTER_BOUND ( 'NONE', #24878, .T. ) ;
#112208 = CARTESIAN_POINT ( 'NONE',  ( 129.5000000000000000, -0.6250000000000000000, 7.634788798650553154 ) ) ;
#112209 = VERTEX_POINT ( 'NONE', #9296 ) ;
#112211 = CIRCLE ( 'NONE', #124721, 0.09999999999999982514 ) ;
#112210 = CIRCLE ( 'NONE', #78778, 0.1000000000000002554 ) ;
#112212 = DIRECTION ( 'NONE',  ( 0.000000000000000000, 0.000000000000000000, 1.000000000000000000 ) ) ;
#112213 = FACE_OUTER_BOUND ( 'NONE', #46962, .T. ) ;
#112214 = CARTESIAN_POINT ( 'NONE',  ( 10.84999999999990905, 12.50000000000000000, -7.122917578226816815 ) ) ;
#112215 = DIRECTION ( 'NONE',  ( 0.000000000000000000, 0.000000000000000000, -1.000000000000000000 ) ) ;
#112216 = FACE_OUTER_BOUND ( 'NONE', #119396, .T. ) ;
#112218 = ADVANCED_FACE ( 'NONE', ( #49241 ), #3584, .T. ) ;
#112217 = CIRCLE ( 'NONE', #122673, 0.09999999999999982514 ) ;
#112219 = CARTESIAN_POINT ( 'NONE',  ( -10.65000000000000391, 2.500000000000000000, -1.718653347947322052 ) ) ;
#112220 = FACE_OUTER_BOUND ( 'NONE', #90191, .T. ) ;
#112222 = AXIS2_PLACEMENT_3D ( 'NONE', #2546, #31402, #52317 ) ;
#112221 = AXIS2_PLACEMENT_3D ( 'NONE', #19754, #99602, #59697 ) ;
#112223 = ORIENTED_EDGE ( 'NONE', *, *, #114426, .F. ) ;
#112224 = VERTEX_POINT ( 'NONE', #62275 ) ;
#112225 = VERTEX_POINT ( 'NONE', #121818 ) ;
#112226 = VERTEX_POINT ( 'NONE', #40051 ) ;
#112227 = DIRECTION ( 'NONE',  ( 0.000000000000000000, 0.000000000000000000, -1.000000000000000000 ) ) ;
#112228 = DIRECTION ( 'NONE',  ( -4.274815082592931898E-19, -0.9999939076577903929, -0.003490651415223739937 ) ) ;
#112229 = CARTESIAN_POINT ( 'NONE',  ( -15.19999999999998330, 2.500000000000000000, 0.2464101615137758439 ) ) ;
#112230 = ORIENTED_EDGE ( 'NONE', *, *, #66010, .T. ) ;
#112231 = FACE_BOUND ( 'NONE', #78627, .T. ) ;
#112232 = CARTESIAN_POINT ( 'NONE',  ( 0.8499999999999545697, 2.500000000000000000, 2.857883832488649301 ) ) ;
#112233 = FACE_OUTER_BOUND ( 'NONE', #28108, .T. ) ;
#112234 = CARTESIAN_POINT ( 'NONE',  ( -3.749999999999991118, 2.500000000000000000, 2.065063509461097624 ) ) ;
#112235 = CARTESIAN_POINT ( 'NONE',  ( 13.54999999999990123, 2.500000000000000000, 1.718653347947321386 ) ) ;
#112236 = CARTESIAN_POINT ( 'NONE',  ( -12.49999999999995914, 12.50000000000000000, 1.843143693225357538E-15 ) ) ;
#112237 = CARTESIAN_POINT ( 'NONE',  ( -7.050000000000013145, 2.500000000000000000, 2.065063509461097624 ) ) ;
#112238 = FACE_OUTER_BOUND ( 'NONE', #124432, .T. ) ;
#112239 = CARTESIAN_POINT ( 'NONE',  ( -2.900000000000030109, 2.500000000000000000, -3.637306695894650055 ) ) ;
#112240 = EDGE_CURVE ( 'NONE', #117617, #30567, #39118, .T. ) ;
#112241 = CARTESIAN_POINT ( 'NONE',  ( -5.450000000000023270, 12.50000000000000000, -2.165063509461101710 ) ) ;
#112242 = CIRCLE ( 'NONE', #34896, 0.06509327318403745899 ) ;
#112243 = CIRCLE ( 'NONE', #74871, 0.1000000000000002554 ) ;
#112244 = CIRCLE ( 'NONE', #101782, 0.06509327318403745899 ) ;
#112245 = VERTEX_POINT ( 'NONE', #69491 ) ;
#112246 = ORIENTED_EDGE ( 'NONE', *, *, #34914, .F. ) ;
#112248 = ORIENTED_EDGE ( 'NONE', *, *, #101408, .T. ) ;
#112247 = CIRCLE ( 'NONE', #41247, 0.06509327318403745899 ) ;
#112249 = ORIENTED_EDGE ( 'NONE', *, *, #48374, .T. ) ;
#112250 = VERTEX_POINT ( 'NONE', #70790 ) ;
#112251 = ORIENTED_EDGE ( 'NONE', *, *, #112106, .T. ) ;
#112252 = FACE_OUTER_BOUND ( 'NONE', #38240, .T. ) ;
#112253 = EDGE_CURVE ( 'NONE', #23452, #1757, #24421, .T. ) ;
#112254 = ORIENTED_EDGE ( 'NONE', *, *, #20772, .F. ) ;
#112256 = VERTEX_POINT ( 'NONE', #79343 ) ;
#112255 = CIRCLE ( 'NONE', #30700, 0.06509327318403745899 ) ;
#112257 = EDGE_CURVE ( 'NONE', #68589, #63643, #101795, .T. ) ;
#112258 = AXIS2_PLACEMENT_3D ( 'NONE', #108515, #59447, #30625 ) ;
#112259 = AXIS2_PLACEMENT_3D ( 'NONE', #11860, #9939, #101546 ) ;
#112260 = EDGE_CURVE ( 'NONE', #48344, #129288, #97569, .T. ) ;
#112261 = CARTESIAN_POINT ( 'NONE',  ( -10.20000000000000462, 2.500000000000000000, 4.676537180435972552 ) ) ;
#112262 = CARTESIAN_POINT ( 'NONE',  ( 7.499999999999925393, 12.50000000000000000, 5.022947341949748790 ) ) ;
#112263 = DIRECTION ( 'NONE',  ( -0.000000000000000000, 1.000000000000000000, -0.000000000000000000 ) ) ;
#112264 = DIRECTION ( 'NONE',  ( 0.000000000000000000, -0.9999939076577903929, 0.003490651415223739937 ) ) ;
#112265 = CIRCLE ( 'NONE', #26580, 0.1000000000000000472 ) ;
#112266 = EDGE_CURVE ( 'NONE', #48297, #41599, #39431, .T. ) ;
#112267 = ORIENTED_EDGE ( 'NONE', *, *, #87831, .T. ) ;
#112268 = CARTESIAN_POINT ( 'NONE',  ( 4.199999999999938005, 2.500000000000000000, 4.230127018922196669 ) ) ;
#112269 = CIRCLE ( 'NONE', #85063, 0.06509327318403745899 ) ;
#112270 = EDGE_CURVE ( 'NONE', #71534, #34595, #87100, .T. ) ;
#112271 = EDGE_CURVE ( 'NONE', #47988, #1124, #16076, .T. ) ;
#112272 = ORIENTED_EDGE ( 'NONE', *, *, #109830, .F. ) ;
#112275 = EDGE_CURVE ( 'NONE', #74808, #6403, #95533, .T. ) ;
#112274 = VECTOR ( 'NONE', #54426, 1000.000000000000000 ) ;
#112273 = CIRCLE ( 'NONE', #5630, 0.09999999999999999167 ) ;
#112276 = ORIENTED_EDGE ( 'NONE', *, *, #65210, .F. ) ;
#112277 = CARTESIAN_POINT ( 'NONE',  ( 8.149999999999920419, 12.50000000000000000, -1.818653347947325916 ) ) ;
#112278 = CARTESIAN_POINT ( 'NONE',  ( 6.649999999999927525, 12.50000000000000000, 2.099970236277060032 ) ) ;
#112279 = ORIENTED_EDGE ( 'NONE', *, *, #73455, .T. ) ;
#112280 = EDGE_CURVE ( 'NONE', #56703, #123357, #116440, .T. ) ;
#112281 = EDGE_LOOP ( 'NONE', ( #17902, #123714, #18001, #49206 ) ) ;
#112282 = CARTESIAN_POINT ( 'NONE',  ( -4.350000000000023626, 2.500000000000000000, -1.718653347947325827 ) ) ;
#112283 = DIRECTION ( 'NONE',  ( 0.000000000000000000, 0.000000000000000000, 1.000000000000000000 ) ) ;
#112284 = CARTESIAN_POINT ( 'NONE',  ( -5.450000000000019718, 2.500000000000000000, 2.065063509461097624 ) ) ;
#112285 = CARTESIAN_POINT ( 'NONE',  ( -13.14999999999999147, 12.50000000000000000, -1.883746621131361376 ) ) ;
#112286 = DIRECTION ( 'NONE',  ( 0.000000000000000000, 0.000000000000000000, 1.000000000000000000 ) ) ;
#112287 = CONICAL_SURFACE ( 'NONE', #20246, 0.1000000000000000056, 0.003490658503988666988 ) ;
#112288 = ORIENTED_EDGE ( 'NONE', *, *, #14063, .F. ) ;
#112289 = PLANE ( 'NONE',  #32364 ) ;
#112290 = ORIENTED_EDGE ( 'NONE', *, *, #124411, .F. ) ;
#112291 = CARTESIAN_POINT ( 'NONE',  ( 14.79999999999989235, 2.500000000000000000, 0.2464101615137735679 ) ) ;
#112292 = LINE ( 'NONE', #122113, #18043 ) ;
#112293 = DIRECTION ( 'NONE',  ( -0.000000000000000000, -1.000000000000000000, -0.000000000000000000 ) ) ;
#112294 = DIRECTION ( 'NONE',  ( 0.000000000000000000, 0.000000000000000000, 1.000000000000000000 ) ) ;
#112295 = CARTESIAN_POINT ( 'NONE',  ( 9.149999999999916866, 12.50000000000000000, -1.407149913249512663 ) ) ;
#112296 = ORIENTED_EDGE ( 'NONE', *, *, #124215, .T. ) ;
#112297 = CARTESIAN_POINT ( 'NONE',  ( -1.050000000000037792, 2.500000000000000000, 6.148780366869520009 ) ) ;
#112298 = AXIS2_PLACEMENT_3D ( 'NONE', #116422, #26132, #88240 ) ;
#112299 = AXIS2_PLACEMENT_3D ( 'NONE', #33296, #73204, #23449 ) ;
#112300 = FACE_OUTER_BOUND ( 'NONE', #92838, .T. ) ;
#112301 = ORIENTED_EDGE ( 'NONE', *, *, #27682, .F. ) ;
#112302 = VERTEX_POINT ( 'NONE', #99620 ) ;
#112303 = ORIENTED_EDGE ( 'NONE', *, *, #81101, .F. ) ;
#112304 = DIRECTION ( 'NONE',  ( 0.000000000000000000, 0.000000000000000000, -1.000000000000000000 ) ) ;
#112305 = DIRECTION ( 'NONE',  ( 0.000000000000000000, -0.9999939076577903929, 0.003490651415223739937 ) ) ;
#112306 = CARTESIAN_POINT ( 'NONE',  ( 186.3593750003414016, 0.000000000000000000, 7.564683531250000925 ) ) ;
#112307 = CARTESIAN_POINT ( 'NONE',  ( -6.900000000000019007, 2.500000000000000000, -3.883716857408426648 ) ) ;
#112310 = AXIS2_PLACEMENT_3D ( 'NONE', #20236, #80451, #68035 ) ;
#112309 = CARTESIAN_POINT ( 'NONE',  ( 4.599999999999936584, 2.500000000000000000, 4.430127018922196847 ) ) ;
#112308 = AXIS2_PLACEMENT_3D ( 'NONE', #64043, #54228, #42486 ) ;
#112312 = EDGE_CURVE ( 'NONE', #125598, #51588, #103843, .T. ) ;
#112311 = LINE ( 'NONE', #63852, #32262 ) ;
#112313 = CARTESIAN_POINT ( 'NONE',  ( 21.24754738303277080, -0.7337760880902354232, 4.182111650399362723 ) ) ;
#112315 = CIRCLE ( 'NONE', #55862, 0.1000000000000002554 ) ;
#112314 = AXIS2_PLACEMENT_3D ( 'NONE', #15039, #94925, #115176 ) ;
#112316 = CARTESIAN_POINT ( 'NONE',  ( -2.100000000000034728, 2.500000000000000000, 4.330127018922196314 ) ) ;
#112317 = ORIENTED_EDGE ( 'NONE', *, *, #125392, .T. ) ;
#112318 = DIRECTION ( 'NONE',  ( 0.000000000000000000, 0.000000000000000000, -1.000000000000000000 ) ) ;
#112319 = EDGE_CURVE ( 'NONE', #2580, #9598, #34909, .T. ) ;
#112320 = CARTESIAN_POINT ( 'NONE',  ( 97.50000000000000000, 0.000000000000000000, 0.000000000000000000 ) ) ;
#112321 = DIRECTION ( 'NONE',  ( 0.000000000000000000, 0.000000000000000000, 1.000000000000000000 ) ) ;
#112322 = LINE ( 'NONE', #3648, #81507 ) ;
#112323 = ORIENTED_EDGE ( 'NONE', *, *, #110626, .F. ) ;
#112324 = DIRECTION ( 'NONE',  ( -0.000000000000000000, -1.000000000000000000, -0.000000000000000000 ) ) ;
#112325 = AXIS2_PLACEMENT_3D ( 'NONE', #84049, #84703, #124634 ) ;
#112326 = DIRECTION ( 'NONE',  ( 0.000000000000000000, 0.000000000000000000, 1.000000000000000000 ) ) ;
#112328 = ORIENTED_EDGE ( 'NONE', *, *, #2863, .T. ) ;
#112327 = DIRECTION ( 'NONE',  ( 0.000000000000000000, 0.000000000000000000, -1.000000000000000000 ) ) ;
#112329 = VECTOR ( 'NONE', #80541, 1000.000000000000000 ) ;
#112330 = ORIENTED_EDGE ( 'NONE', *, *, #20926, .T. ) ;
#112331 = AXIS2_PLACEMENT_3D ( 'NONE', #49575, #67225, #98640 ) ;
#112332 = CARTESIAN_POINT ( 'NONE',  ( -11.44999999999999751, 12.50000000000000000, 1.818653347947321475 ) ) ;
#112333 = PRESENTATION_LAYER_ASSIGNMENT (  '', '', ( #89351 ) ) ;
#112334 = ORIENTED_EDGE ( 'NONE', *, *, #103374, .T. ) ;
#112335 = ORIENTED_EDGE ( 'NONE', *, *, #9310, .T. ) ;
#112336 = CARTESIAN_POINT ( 'NONE',  ( 8.349999999999923261, 12.50000000000000000, 1.472243186433545459 ) ) ;
#112337 = CONICAL_SURFACE ( 'NONE', #3664, 0.1000000000000000056, 0.003490658503988666988 ) ;
#112338 = LINE ( 'NONE', #24600, #88615 ) ;
#112339 = FACE_OUTER_BOUND ( 'NONE', #22139, .T. ) ;
#112340 = AXIS2_PLACEMENT_3D ( 'NONE', #34493, #73111, #101282 ) ;
#112341 = DIRECTION ( 'NONE',  ( 0.000000000000000000, 0.000000000000000000, -1.000000000000000000 ) ) ;
#112342 = ORIENTED_EDGE ( 'NONE', *, *, #105907, .T. ) ;
#112343 = AXIS2_PLACEMENT_3D ( 'NONE', #89907, #68979, #108888 ) ;
#112344 = AXIS2_PLACEMENT_3D ( 'NONE', #77865, #127623, #37328 ) ;
#112345 = EDGE_CURVE ( 'NONE', #28931, #58767, #41176, .T. ) ;
#112346 = DIRECTION ( 'NONE',  ( 0.000000000000000000, 0.000000000000000000, 1.000000000000000000 ) ) ;
#112348 = VERTEX_POINT ( 'NONE', #70158 ) ;
#112347 = CARTESIAN_POINT ( 'NONE',  ( 127.5000000000000000, 0.000000000000000000, 0.000000000000000000 ) ) ;
#112349 = CARTESIAN_POINT ( 'NONE',  ( 16.64732342991096203, 0.5906619306577837181, 5.996708608299528009 ) ) ;
#112350 = DIRECTION ( 'NONE',  ( 0.000000000000000000, 1.000000000000000000, 0.000000000000000000 ) ) ;
#112351 = EDGE_CURVE ( 'NONE', #24119, #56014, #26572, .T. ) ;
#112352 = EDGE_LOOP ( 'NONE', ( #128441, #9686 ) ) ;
#112353 = AXIS2_PLACEMENT_3D ( 'NONE', #104504, #56042, #16747 ) ;
#112354 = ORIENTED_EDGE ( 'NONE', *, *, #11245, .F. ) ;
#112355 = VERTEX_POINT ( 'NONE', #12507 ) ;
#112356 = ORIENTED_EDGE ( 'NONE', *, *, #81243, .F. ) ;
#112357 = CARTESIAN_POINT ( 'NONE',  ( 8.099999999999923261, 2.500000000000000000, 3.883716857408420431 ) ) ;
#112358 = CARTESIAN_POINT ( 'NONE',  ( 14.37945523803923287, 1.499999999999936273, 7.667852710426877216 ) ) ;
#112359 = EDGE_CURVE ( 'NONE', #74685, #41154, #41985, .T. ) ;
#112360 = ADVANCED_FACE ( 'NONE', ( #110078 ), #105990, .T. ) ;
#112361 = DIRECTION ( 'NONE',  ( -0.000000000000000000, -1.000000000000000000, -0.000000000000000000 ) ) ;
#112362 = EDGE_CURVE ( 'NONE', #10740, #35393, #10565, .T. ) ;
#112363 = FACE_BOUND ( 'NONE', #92692, .T. ) ;
#112365 = ADVANCED_FACE ( 'NONE', ( #757 ), #7676, .T. ) ;
#112364 = ORIENTED_EDGE ( 'NONE', *, *, #59537, .F. ) ;
#112366 = CARTESIAN_POINT ( 'NONE',  ( 184.1562500006828316, 8.891194145520236347, 5.444286225454521982E-16 ) ) ;
#112367 = EDGE_CURVE ( 'NONE', #18925, #125929, #80866, .T. ) ;
#112368 = DIRECTION ( 'NONE',  ( 0.000000000000000000, 0.000000000000000000, 1.000000000000000000 ) ) ;
#112369 = DIRECTION ( 'NONE',  ( 0.000000000000000000, 0.000000000000000000, 1.000000000000000000 ) ) ;
#112370 = CARTESIAN_POINT ( 'NONE',  ( -1.450000000000036371, 2.500000000000000000, 6.841600689897072485 ) ) ;
#112371 = DIRECTION ( 'NONE',  ( -0.000000000000000000, 1.000000000000000000, -0.000000000000000000 ) ) ;
#112372 = UNCERTAINTY_MEASURE_WITH_UNIT (LENGTH_MEASURE( 1.000000000000000082E-05 ), #104838, 'distance_accuracy_value', 'NONE');
#112374 = EDGE_CURVE ( 'NONE', #119283, #8339, #15053, .T. ) ;
#112373 = AXIS2_PLACEMENT_3D ( 'NONE', #28319, #97055, #68229 ) ;
#112375 = CARTESIAN_POINT ( 'NONE',  ( 2.299999999999949640, 2.500000000000000000, -4.676537180435977881 ) ) ;
#112376 = ADVANCED_FACE ( 'NONE', ( #114567 ), #66274, .T. ) ;
#112377 = EDGE_CURVE ( 'NONE', #90163, #101350, #68331, .T. ) ;
#112378 = LINE ( 'NONE', #114929, #43181 ) ;
#112379 = EDGE_LOOP ( 'NONE', ( #38250, #39422, #61666, #83285 ) ) ;
#112380 = ORIENTED_EDGE ( 'NONE', *, *, #62258, .F. ) ;
#112381 = VERTEX_POINT ( 'NONE', #13138 ) ;
#112382 = ORIENTED_EDGE ( 'NONE', *, *, #55031, .F. ) ;
#112383 = VERTEX_POINT ( 'NONE', #123119 ) ;
#112384 = CARTESIAN_POINT ( 'NONE',  ( 4.599999999999940137, 12.50000000000000000, -5.022947341949754119 ) ) ;
#112385 = CARTESIAN_POINT ( 'NONE',  ( 2.899999999999944844, 12.50000000000000000, 5.022947341949748790 ) ) ;
#112386 = EDGE_LOOP ( 'NONE', ( #83723, #89821, #38318, #49475 ) ) ;
#112387 = FACE_BOUND ( 'NONE', #2006, .T. ) ;
#112388 = DIRECTION ( 'NONE',  ( 0.000000000000000000, -0.9999939076577903929, 0.003490651415223739937 ) ) ;
#112389 = AXIS2_PLACEMENT_3D ( 'NONE', #108867, #108235, #88602 ) ;
#112390 = AXIS2_PLACEMENT_3D ( 'NONE', #63064, #13951, #21868 ) ;
#112391 = ORIENTED_EDGE ( 'NONE', *, *, #63750, .F. ) ;
#112392 = CYLINDRICAL_SURFACE ( 'NONE', #20218, 2.000000000000000000 ) ;
#112393 = DIRECTION ( 'NONE',  ( -0.000000000000000000, -1.000000000000000000, -0.000000000000000000 ) ) ;
#112394 = LINE ( 'NONE', #84202, #91403 ) ;
#112395 = EDGE_LOOP ( 'NONE', ( #48461, #127830 ) ) ;
#112396 = CARTESIAN_POINT ( 'NONE',  ( -1.650000000000034328, 2.500000000000000000, -6.495190528383302464 ) ) ;
#112397 = AXIS2_PLACEMENT_3D ( 'NONE', #108248, #18586, #66391 ) ;
#112398 = ORIENTED_EDGE ( 'NONE', *, *, #98579, .T. ) ;
#112399 = CIRCLE ( 'NONE', #55951, 8.199999999999999289 ) ;
#112400 = VECTOR ( 'NONE', #109942, 1000.000000000000000 ) ;
#112401 = ORIENTED_EDGE ( 'NONE', *, *, #29022, .T. ) ;
#112402 = VERTEX_POINT ( 'NONE', #64828 ) ;
#112403 = CARTESIAN_POINT ( 'NONE',  ( -9.150000000000009237, 2.500000000000000000, 2.265063509461097357 ) ) ;
#112404 = CARTESIAN_POINT ( 'NONE',  ( 1.649999999999950617, 2.500000000000000000, -2.265063509461101798 ) ) ;
#112405 = CARTESIAN_POINT ( 'NONE',  ( -6.850000000000017408, 2.500000000000000000, -2.611473670974877592 ) ) ;
#112406 = ORIENTED_EDGE ( 'NONE', *, *, #80415, .F. ) ;
#112407 = CARTESIAN_POINT ( 'NONE',  ( -13.94999999999998685, 2.500000000000000000, -2.611473670974875372 ) ) ;
#112408 = VECTOR ( 'NONE', #26905, 1000.000000000000000 ) ;
#112409 = CARTESIAN_POINT ( 'NONE',  ( -11.05000000000000249, 2.500000000000000000, -1.818653347947322141 ) ) ;
#112410 = FACE_OUTER_BOUND ( 'NONE', #80144, .T. ) ;
#112411 = DIRECTION ( 'NONE',  ( 0.000000000000000000, 1.000000000000000000, 0.000000000000000000 ) ) ;
#112412 = DIRECTION ( 'NONE',  ( 0.000000000000000000, 0.000000000000000000, 1.000000000000000000 ) ) ;
#112413 = EDGE_LOOP ( 'NONE', ( #57630, #2645 ) ) ;
#112414 = CONICAL_SURFACE ( 'NONE', #7935, 0.09999999999999982514, 0.003490658503988666988 ) ;
#112415 = FACE_OUTER_BOUND ( 'NONE', #4499, .T. ) ;
#112416 = ADVANCED_FACE ( 'NONE', ( #32822 ), #28634, .T. ) ;
#112417 = ORIENTED_EDGE ( 'NONE', *, *, #96325, .T. ) ;
#112418 = CARTESIAN_POINT ( 'NONE',  ( 9.799999999999915445, 12.50000000000000000, 3.918623584224383727 ) ) ;
#112419 = EDGE_CURVE ( 'NONE', #79956, #27779, #43285, .T. ) ;
#112420 = CIRCLE ( 'NONE', #55963, 0.06509327318403745899 ) ;
#112421 = EDGE_LOOP ( 'NONE', ( #11094, #86343 ) ) ;
#112422 = EDGE_CURVE ( 'NONE', #38146, #96104, #11988, .T. ) ;
#112423 = VERTEX_POINT ( 'NONE', #4588 ) ;
#112424 = DIRECTION ( 'NONE',  ( 0.000000000000000000, 1.000000000000000000, 0.000000000000000000 ) ) ;
#112425 = VECTOR ( 'NONE', #25805, 1000.000000000000000 ) ;
#112426 = CARTESIAN_POINT ( 'NONE',  ( 2.899999999999946620, 12.50000000000000000, -4.957854068765716882 ) ) ;
#112427 = CARTESIAN_POINT ( 'NONE',  ( 3.099999999999945022, 2.500000000000000000, -0.3464101615137783474 ) ) ;
#112428 = DIRECTION ( 'NONE',  ( 0.000000000000000000, 1.000000000000000000, 0.000000000000000000 ) ) ;
#112430 = CIRCLE ( 'NONE', #24587, 0.1000000000000000472 ) ;
#112429 = PLANE ( 'NONE',  #14065 ) ;
#112431 = ORIENTED_EDGE ( 'NONE', *, *, #92914, .F. ) ;
#112432 = AXIS2_PLACEMENT_3D ( 'NONE', #70092, #78639, #68794 ) ;
#112433 = ADVANCED_FACE ( 'NONE', ( #112655 ), #97669, .T. ) ;
#112434 = ORIENTED_EDGE ( 'NONE', *, *, #60972, .T. ) ;
#112435 = FACE_OUTER_BOUND ( 'NONE', #114855, .T. ) ;
#112436 = AXIS2_PLACEMENT_3D ( 'NONE', #125843, #123281, #6061 ) ;
#112437 = CARTESIAN_POINT ( 'NONE',  ( 10.84999999999991260, 2.500000000000000000, 5.702370205355745014 ) ) ;
#112438 = CARTESIAN_POINT ( 'NONE',  ( -10.85000000000000142, 2.500000000000000000, -7.188010851410850499 ) ) ;
#112439 = ORIENTED_EDGE ( 'NONE', *, *, #110364, .F. ) ;
#112440 = EDGE_LOOP ( 'NONE', ( #19263, #22943 ) ) ;
#112441 = CARTESIAN_POINT ( 'NONE',  ( -6.050000000000022027, 2.500000000000000000, -6.148780366869526226 ) ) ;
#112442 = AXIS2_PLACEMENT_3D ( 'NONE', #10015, #60428, #91154 ) ;
#112443 = CIRCLE ( 'NONE', #74582, 0.06509327318403745899 ) ;
#112444 = EDGE_LOOP ( 'NONE', ( #11561, #54671 ) ) ;
#112445 = CARTESIAN_POINT ( 'NONE',  ( -6.700000000000019718, 2.500000000000000000, -0.1000000000000023925 ) ) ;
#112446 = CARTESIAN_POINT ( 'NONE',  ( -13.09999999999999254, 2.500000000000000000, -4.576537180435974683 ) ) ;
#112447 = AXIS2_PLACEMENT_3D ( 'NONE', #23471, #94792, #92203 ) ;
#112448 = CARTESIAN_POINT ( 'NONE',  ( 0.3999999999999555023, 2.500000000000000000, 4.230127018922196669 ) ) ;
#112449 = ORIENTED_EDGE ( 'NONE', *, *, #42404, .F. ) ;
#112450 = DIRECTION ( 'NONE',  ( 0.000000000000000000, -0.000000000000000000, 1.000000000000000000 ) ) ;
#112451 = DIRECTION ( 'NONE',  ( 0.000000000000000000, 1.000000000000000000, 0.000000000000000000 ) ) ;
#112452 = PLANE ( 'NONE',  #35780 ) ;
#112453 = CARTESIAN_POINT ( 'NONE',  ( -14.99999999999998224, 2.500000000000000000, -0.7928203230275518987 ) ) ;
#112454 = CONICAL_SURFACE ( 'NONE', #58069, 0.09999999999999982514, 0.003490658503988666988 ) ;
#112455 = ADVANCED_FACE ( 'NONE', ( #15722 ), #60138, .T. ) ;
#112456 = DIRECTION ( 'NONE',  ( 0.000000000000000000, 1.000000000000000000, 0.000000000000000000 ) ) ;
#112457 = VERTEX_POINT ( 'NONE', #123736 ) ;
#112458 = DIRECTION ( 'NONE',  ( 0.000000000000000000, 0.000000000000000000, -1.000000000000000000 ) ) ;
#112460 = CONICAL_SURFACE ( 'NONE', #72737, 0.1000000000000002554, 0.003490658503988666988 ) ;
#112459 = AXIS2_PLACEMENT_3D ( 'NONE', #85233, #6629, #35503 ) ;
#112461 = DIRECTION ( 'NONE',  ( -0.000000000000000000, 1.000000000000000000, -0.000000000000000000 ) ) ;
#112462 = ORIENTED_EDGE ( 'NONE', *, *, #84833, .T. ) ;
#112463 = VERTEX_POINT ( 'NONE', #54369 ) ;
#112464 = CARTESIAN_POINT ( 'NONE',  ( 186.2135416670080872, 4.367472073101518859, -7.564683531249999149 ) ) ;
#112465 = DIRECTION ( 'NONE',  ( 0.000000000000000000, -0.9999939076577903929, 0.003490651415223739937 ) ) ;
#112466 = CARTESIAN_POINT ( 'NONE',  ( 5.199999999999933564, 2.500000000000000000, 3.983716857408420076 ) ) ;
#112467 = CARTESIAN_POINT ( 'NONE',  ( -5.450000000000023270, 2.500000000000000000, -6.495190528383302464 ) ) ;
#112468 = CARTESIAN_POINT ( 'NONE',  ( 4.599999999999936584, 12.50000000000000000, 3.702399969078682407 ) ) ;
#112469 = FACE_OUTER_BOUND ( 'NONE', #110306, .T. ) ;
#112470 = EDGE_CURVE ( 'NONE', #17072, #64922, #37138, .T. ) ;
#112471 = FACE_OUTER_BOUND ( 'NONE', #106658, .T. ) ;
#112472 = CARTESIAN_POINT ( 'NONE',  ( 11.84999999999990727, 2.500000000000000000, 6.048780366869520364 ) ) ;
#112473 = CARTESIAN_POINT ( 'NONE',  ( -0.8500000000000386136, 2.500000000000000000, 2.857883832488649301 ) ) ;
#112474 = EDGE_LOOP ( 'NONE', ( #78308, #100432, #22767 ) ) ;
#112475 = ORIENTED_EDGE ( 'NONE', *, *, #54300, .T. ) ;
#112476 = ORIENTED_EDGE ( 'NONE', *, *, #80475, .F. ) ;
#112477 = VECTOR ( 'NONE', #19498, 1000.000000000000000 ) ;
#112478 = ORIENTED_EDGE ( 'NONE', *, *, #118703, .F. ) ;
#112479 = EDGE_CURVE ( 'NONE', #122530, #78195, #33463, .T. ) ;
#112480 = FACE_OUTER_BOUND ( 'NONE', #76338, .T. ) ;
#112481 = CARTESIAN_POINT ( 'NONE',  ( 5.849999999999935696, 12.50000000000000000, -6.495190528383302464 ) ) ;
#112482 = ORIENTED_EDGE ( 'NONE', *, *, #44667, .T. ) ;
#112483 = PLANE ( 'NONE',  #79990 ) ;
#112484 = CIRCLE ( 'NONE', #127062, 0.1000000000000002554 ) ;
#112485 = DIRECTION ( 'NONE',  ( 0.000000000000000000, 0.000000000000000000, 1.000000000000000000 ) ) ;
#112487 = ORIENTED_EDGE ( 'NONE', *, *, #36152, .T. ) ;
#112486 = DIRECTION ( 'NONE',  ( 0.000000000000000000, 1.000000000000000000, 0.000000000000000000 ) ) ;
#112488 = ADVANCED_FACE ( 'NONE', ( #94955 ), #47505, .T. ) ;
#112489 = DIRECTION ( 'NONE',  ( 0.000000000000000000, 0.000000000000000000, -1.000000000000000000 ) ) ;
#112490 = CIRCLE ( 'NONE', #129143, 0.06509327318403743123 ) ;
#112491 = LINE ( 'NONE', #53567, #62579 ) ;
#112492 = ORIENTED_EDGE ( 'NONE', *, *, #82069, .F. ) ;
#112493 = CONICAL_SURFACE ( 'NONE', #33091, 0.1000000000000000056, 0.003490658503988666988 ) ;
#112494 = ORIENTED_EDGE ( 'NONE', *, *, #122704, .T. ) ;
#112495 = VERTEX_POINT ( 'NONE', #105412 ) ;
#112496 = VERTEX_POINT ( 'NONE', #44557 ) ;
#112497 = DIRECTION ( 'NONE',  ( -0.000000000000000000, -1.000000000000000000, -0.000000000000000000 ) ) ;
#112498 = LINE ( 'NONE', #31366, #82272 ) ;
#112499 = CARTESIAN_POINT ( 'NONE',  ( -2.100000000000033396, 2.500000000000000000, -0.6928203230275542523 ) ) ;
#112500 = CARTESIAN_POINT ( 'NONE',  ( -15.59999999999998010, 2.500000000000000000, -0.3464101615137759604 ) ) ;
#112501 = AXIS2_PLACEMENT_3D ( 'NONE', #29488, #60254, #73269 ) ;
#112502 = ORIENTED_EDGE ( 'NONE', *, *, #75338, .F. ) ;
#112503 = EDGE_CURVE ( 'NONE', #116053, #80727, #3671, .T. ) ;
#112504 = CARTESIAN_POINT ( 'NONE',  ( -0.6500000000000394351, 2.500000000000000000, 2.411473670974873862 ) ) ;
#112505 = ORIENTED_EDGE ( 'NONE', *, *, #16992, .T. ) ;
#112506 = CIRCLE ( 'NONE', #114630, 0.1000000000000002554 ) ;
#112507 = DIRECTION ( 'NONE',  ( -4.274815082592931898E-19, -0.9999939076577903929, -0.003490651415223739937 ) ) ;
#112508 = CARTESIAN_POINT ( 'NONE',  ( 4.912722231824926844, -1.499999999999620082, -9.942384337864403676 ) ) ;
#112509 = DIRECTION ( 'NONE',  ( -0.000000000000000000, -1.000000000000000000, -0.000000000000000000 ) ) ;
#112510 = CARTESIAN_POINT ( 'NONE',  ( 4.599999999999936584, 12.50000000000000000, 4.330127018922196314 ) ) ;
#112511 = ADVANCED_FACE ( 'NONE', ( #23623 ), #24518, .T. ) ;
#112512 = VERTEX_POINT ( 'NONE', #125040 ) ;
#112513 = AXIS2_PLACEMENT_3D ( 'NONE', #66720, #106654, #59524 ) ;
#112514 = ORIENTED_EDGE ( 'NONE', *, *, #24584, .T. ) ;
#112515 = ORIENTED_EDGE ( 'NONE', *, *, #97288, .T. ) ;
#112516 = DIRECTION ( 'NONE',  ( -0.000000000000000000, 1.000000000000000000, -0.000000000000000000 ) ) ;
#112517 = CARTESIAN_POINT ( 'NONE',  ( 6.249999999999930722, 12.50000000000000000, -1.537336459617587581 ) ) ;
#112518 = EDGE_CURVE ( 'NONE', #76477, #80752, #114387, .T. ) ;
#112519 = EDGE_CURVE ( 'NONE', #67433, #112003, #106082, .T. ) ;
#112520 = DIRECTION ( 'NONE',  ( -0.000000000000000000, 1.000000000000000000, -0.000000000000000000 ) ) ;
#112521 = EDGE_CURVE ( 'NONE', #54360, #1523, #87194, .T. ) ;
#112522 = FACE_BOUND ( 'NONE', #50819, .T. ) ;
#112523 = AXIS2_PLACEMENT_3D ( 'NONE', #111094, #21450, #106928 ) ;
#112524 = ADVANCED_FACE ( 'NONE', ( #86397 ), #17661, .T. ) ;
#112525 = CARTESIAN_POINT ( 'NONE',  ( 12.94999999999989981, 2.500000000000000000, -2.165063509461101710 ) ) ;
#112526 = CARTESIAN_POINT ( 'NONE',  ( 8.949999999999921130, 12.50000000000000000, 1.818653347947321475 ) ) ;
#112527 = AXIS2_PLACEMENT_3D ( 'NONE', #12124, #52075, #120801 ) ;
#112528 = DIRECTION ( 'NONE',  ( 0.000000000000000000, 0.000000000000000000, 1.000000000000000000 ) ) ;
#112529 = AXIS2_PLACEMENT_3D ( 'NONE', #119900, #71423, #60973 ) ;
#112530 = EDGE_CURVE ( 'NONE', #126433, #54302, #18942, .T. ) ;
#112531 = CARTESIAN_POINT ( 'NONE',  ( -12.89999999999999325, 12.50000000000000000, -3.572213422710609709 ) ) ;
#112532 = ADVANCED_FACE ( 'NONE', ( #128286 ), #85754, .T. ) ;
#112534 = CARTESIAN_POINT ( 'NONE',  ( -8.350000000000010303, 2.500000000000000000, 6.595190528383296780 ) ) ;
#112533 = AXIS2_PLACEMENT_3D ( 'NONE', #86476, #56371, #126413 ) ;
#112535 = EDGE_CURVE ( 'NONE', #75419, #30036, #89360, .T. ) ;
#112536 = DIRECTION ( 'NONE',  ( 0.000000000000000000, -0.9999939076577903929, 0.003490651415223739937 ) ) ;
#112537 = EDGE_LOOP ( 'NONE', ( #93124, #79744 ) ) ;
#112538 = EDGE_CURVE ( 'NONE', #12633, #81499, #76846, .T. ) ;
#112539 = EDGE_CURVE ( 'NONE', #8359, #16632, #91406, .T. ) ;
#112540 = DIRECTION ( 'NONE',  ( 0.000000000000000000, 0.000000000000000000, -1.000000000000000000 ) ) ;
#112541 = VERTEX_POINT ( 'NONE', #46473 ) ;
#112542 = ORIENTED_EDGE ( 'NONE', *, *, #117045, .T. ) ;
#112543 = CARTESIAN_POINT ( 'NONE',  ( -8.550000000000009592, 12.50000000000000000, 6.841600689897072485 ) ) ;
#112544 = CIRCLE ( 'NONE', #116720, 0.1000000000000002554 ) ;
#112545 = DIRECTION ( 'NONE',  ( 0.000000000000000000, 0.000000000000000000, 1.000000000000000000 ) ) ;
#112546 = FACE_BOUND ( 'NONE', #108906, .T. ) ;
#112547 = ADVANCED_FACE ( 'NONE', ( #125673 ), #49669, .T. ) ;
#112548 = DIRECTION ( 'NONE',  ( 0.000000000000000000, 0.000000000000000000, 1.000000000000000000 ) ) ;
#112550 = AXIS2_PLACEMENT_3D ( 'NONE', #83832, #83212, #123748 ) ;
#112549 = TOROIDAL_SURFACE ( 'NONE', #120849, 4.000000000000000000, 1.000000000000000000 ) ;
#112551 = ORIENTED_EDGE ( 'NONE', *, *, #114870, .T. ) ;
#112552 = DIRECTION ( 'NONE',  ( 1.000000000000000000, -0.000000000000000000, -0.000000000000000000 ) ) ;
#112553 = DIRECTION ( 'NONE',  ( -0.000000000000000000, 1.000000000000000000, -0.000000000000000000 ) ) ;
#112554 = ORIENTED_EDGE ( 'NONE', *, *, #54866, .T. ) ;
#112555 = FACE_OUTER_BOUND ( 'NONE', #72357, .T. ) ;
#112556 = CARTESIAN_POINT ( 'NONE',  ( 8.349999999999923261, 2.500000000000000000, -5.802370205355749988 ) ) ;
#112557 = VERTEX_POINT ( 'NONE', #76591 ) ;
#112558 = AXIS2_PLACEMENT_3D ( 'NONE', #30133, #102080, #62167 ) ;
#112559 = LINE ( 'NONE', #109975, #38114 ) ;
#112560 = CARTESIAN_POINT ( 'NONE',  ( 13.74999999999993072, 2.500000000000000000, -2.165063509461101710 ) ) ;
#112561 = ORIENTED_EDGE ( 'NONE', *, *, #98279, .F. ) ;
#112562 = CONICAL_SURFACE ( 'NONE', #79122, 0.1000000000000002554, 0.003490658503988666988 ) ;
#112563 = DIRECTION ( 'NONE',  ( -4.274815082592931898E-19, -0.9999939076577903929, -0.003490651415223739937 ) ) ;
#112564 = CIRCLE ( 'NONE', #50161, 0.06509327318403745899 ) ;
#112565 = CARTESIAN_POINT ( 'NONE',  ( 186.9895833340161744, -4.445597072760123503, -7.699999999999989519 ) ) ;
#112566 = AXIS2_PLACEMENT_3D ( 'NONE', #12280, #41782, #50949 ) ;
#112567 = CARTESIAN_POINT ( 'NONE',  ( 11.44999999999990870, 2.500000000000000000, 6.941600689897073018 ) ) ;
#112568 = ORIENTED_EDGE ( 'NONE', *, *, #49195, .F. ) ;
#112569 = VERTEX_POINT ( 'NONE', #57606 ) ;
#112570 = DIRECTION ( 'NONE',  ( 0.000000000000000000, 0.000000000000000000, 1.000000000000000000 ) ) ;
#112572 = VERTEX_POINT ( 'NONE', #97513 ) ;
#112571 = AXIS2_PLACEMENT_3D ( 'NONE', #31767, #120778, #101796 ) ;
#112573 = DIRECTION ( 'NONE',  ( 0.000000000000000000, 0.000000000000000000, -1.000000000000000000 ) ) ;
#112574 = DIRECTION ( 'NONE',  ( 0.000000000000000000, 0.000000000000000000, 1.000000000000000000 ) ) ;
#112575 = ADVANCED_FACE ( 'NONE', ( #45847 ), #1518, .T. ) ;
#112576 = CONICAL_SURFACE ( 'NONE', #22698, 0.1000000000000002554, 0.003490658503988666988 ) ;
#112577 = ORIENTED_EDGE ( 'NONE', *, *, #2709, .F. ) ;
#112579 = EDGE_CURVE ( 'NONE', #93656, #83109, #115868, .T. ) ;
#112578 = DIRECTION ( 'NONE',  ( 0.000000000000000000, 0.000000000000000000, 1.000000000000000000 ) ) ;
#112580 = DIRECTION ( 'NONE',  ( 0.000000000000000000, 0.000000000000000000, -1.000000000000000000 ) ) ;
#112581 = FACE_OUTER_BOUND ( 'NONE', #44750, .T. ) ;
#112582 = DIRECTION ( 'NONE',  ( 0.000000000000000000, 1.000000000000000000, 0.000000000000000000 ) ) ;
#112583 = CARTESIAN_POINT ( 'NONE',  ( -6.650000000000014566, 2.500000000000000000, 2.065063509461097624 ) ) ;
#112584 = CONICAL_SURFACE ( 'NONE', #56123, 0.1000000000000000472, 0.003490658503988666988 ) ;
#112585 = EDGE_CURVE ( 'NONE', #70628, #73131, #16351, .T. ) ;
#112586 = ORIENTED_EDGE ( 'NONE', *, *, #126262, .T. ) ;
#112588 = EDGE_LOOP ( 'NONE', ( #41438, #82057, #25684, #56199 ) ) ;
#112587 = CONICAL_SURFACE ( 'NONE', #1750, 0.1000000000000002554, 0.003490658503988666988 ) ;
#112589 = CARTESIAN_POINT ( 'NONE',  ( -1.250000000000001554, 2.500000000000000000, 2.165063509461097713 ) ) ;
#112590 = VERTEX_POINT ( 'NONE', #7838 ) ;
#112591 = DIRECTION ( 'NONE',  ( 0.000000000000000000, -0.9999939076577903929, 0.003490651415223739937 ) ) ;
#112593 = VERTEX_POINT ( 'NONE', #7190 ) ;
#112592 = ORIENTED_EDGE ( 'NONE', *, *, #26689, .T. ) ;
#112594 = EDGE_LOOP ( 'NONE', ( #23026, #41196 ) ) ;
#112595 = DIRECTION ( 'NONE',  ( 0.000000000000000000, 1.000000000000000000, 0.000000000000000000 ) ) ;
#112596 = CARTESIAN_POINT ( 'NONE',  ( 12.89999999999989910, 12.50000000000000000, 0.6928203230275494784 ) ) ;
#112597 = DIRECTION ( 'NONE',  ( 0.000000000000000000, 0.000000000000000000, -1.000000000000000000 ) ) ;
#112598 = CARTESIAN_POINT ( 'NONE',  ( 105.5000000000000142, 0.000000000000000000, 0.000000000000000000 ) ) ;
#112599 = CARTESIAN_POINT ( 'NONE',  ( 184.8645833340161175, -6.668395609140180369, 3.849999999999994760 ) ) ;
#112600 = CLOSED_SHELL ( 'NONE', ( #95031, #60816, #8391, #56639, #34746, #48698, #120796, #16030, #56171, #43089 ) ) ;
#112601 = LINE ( 'NONE', #13077, #25555 ) ;
#112602 = PLANE ( 'NONE',  #103511 ) ;
#112603 = CIRCLE ( 'NONE', #77085, 0.1000000000000002554 ) ;
#112604 = DIRECTION ( 'NONE',  ( -0.000000000000000000, -1.000000000000000000, -0.000000000000000000 ) ) ;
#112605 = LINE ( 'NONE', #31466, #24739 ) ;
#112606 = AXIS2_PLACEMENT_3D ( 'NONE', #64642, #35203, #13599 ) ;
#112607 = ORIENTED_EDGE ( 'NONE', *, *, #65260, .T. ) ;
#112608 = DIRECTION ( 'NONE',  ( 0.000000000000000000, 1.000000000000000000, 0.000000000000000000 ) ) ;
#112609 = VERTEX_POINT ( 'NONE', #78548 ) ;
#112610 = ORIENTED_EDGE ( 'NONE', *, *, #78276, .T. ) ;
#112611 = DIRECTION ( 'NONE',  ( 0.000000000000000000, 0.000000000000000000, 1.000000000000000000 ) ) ;
#112612 = CARTESIAN_POINT ( 'NONE',  ( 8.299999999999922551, 12.50000000000000000, -4.330127018922201643 ) ) ;
#112613 = CONICAL_SURFACE ( 'NONE', #100090, 0.09999999999999982514, 0.003490658503988666988 ) ;
#112614 = DIRECTION ( 'NONE',  ( 0.000000000000000000, 0.000000000000000000, 1.000000000000000000 ) ) ;
#112615 = EDGE_CURVE ( 'NONE', #45445, #29934, #53755, .T. ) ;
#112617 = AXIS2_PLACEMENT_3D ( 'NONE', #112347, #122809, #63886 ) ;
#112616 = DIRECTION ( 'NONE',  ( 0.000000000000000000, 0.000000000000000000, -1.000000000000000000 ) ) ;
#112618 = DIRECTION ( 'NONE',  ( 0.000000000000000000, 1.000000000000000000, 0.000000000000000000 ) ) ;
#112619 = LINE ( 'NONE', #54333, #15575 ) ;
#112620 = CARTESIAN_POINT ( 'NONE',  ( 11.64999999999990798, 2.500000000000000000, -2.957883832488653830 ) ) ;
#112621 = EDGE_LOOP ( 'NONE', ( #126171, #4920, #117869, #8468 ) ) ;
#112622 = AXIS2_PLACEMENT_3D ( 'NONE', #73425, #113355, #81960 ) ;
#112623 = ORIENTED_EDGE ( 'NONE', *, *, #40594, .T. ) ;
#112624 = VERTEX_POINT ( 'NONE', #126986 ) ;
#112625 = CIRCLE ( 'NONE', #56166, 0.1000000000000002554 ) ;
#112626 = EDGE_LOOP ( 'NONE', ( #56828, #90343 ) ) ;
#112627 = EDGE_CURVE ( 'NONE', #115877, #71057, #116535, .T. ) ;
#112628 = VECTOR ( 'NONE', #10313, 1000.000000000000000 ) ;
#112630 = ORIENTED_EDGE ( 'NONE', *, *, #77646, .F. ) ;
#112629 = ADVANCED_FACE ( 'NONE', ( #87044 ), #55900, .T. ) ;
#112631 = DIRECTION ( 'NONE',  ( 0.000000000000000000, 1.000000000000000000, 0.000000000000000000 ) ) ;
#112632 = FACE_OUTER_BOUND ( 'NONE', #90889, .T. ) ;
#112634 = CIRCLE ( 'NONE', #41542, 0.09999999999999999167 ) ;
#112633 = AXIS2_PLACEMENT_3D ( 'NONE', #100060, #69959, #39870 ) ;
#112635 = DIRECTION ( 'NONE',  ( 0.000000000000000000, 0.000000000000000000, 1.000000000000000000 ) ) ;
#112636 = FACE_OUTER_BOUND ( 'NONE', #41380, .T. ) ;
#112637 = CARTESIAN_POINT ( 'NONE',  ( 9.199999999999919353, 2.500000000000000000, -2.276824562219559311E-15 ) ) ;
#112638 = ORIENTED_EDGE ( 'NONE', *, *, #30277, .F. ) ;
#112639 = CARTESIAN_POINT ( 'NONE',  ( 7.499999999999925393, 12.50000000000000000, 5.022947341949748790 ) ) ;
#112640 = EDGE_CURVE ( 'NONE', #8229, #38593, #18246, .T. ) ;
#112641 = CARTESIAN_POINT ( 'NONE',  ( -10.00000000000000711, 12.50000000000000000, -3.637306695894645614 ) ) ;
#112642 = CARTESIAN_POINT ( 'NONE',  ( 14.99999999999989342, 12.50000000000000000, -0.7579135962115916003 ) ) ;
#112643 = DIRECTION ( 'NONE',  ( 1.000000000000000000, 0.000000000000000000, 0.000000000000000000 ) ) ;
#112644 = ORIENTED_EDGE ( 'NONE', *, *, #116075, .F. ) ;
#112645 = VERTEX_POINT ( 'NONE', #117778 ) ;
#112646 = VERTEX_POINT ( 'NONE', #68054 ) ;
#112647 = AXIS2_PLACEMENT_3D ( 'NONE', #87577, #15610, #98049 ) ;
#112648 = DIRECTION ( 'NONE',  ( 0.000000000000000000, -0.000000000000000000, 1.000000000000000000 ) ) ;
#112649 = CARTESIAN_POINT ( 'NONE',  ( -1.050000000000038680, 2.500000000000000000, 2.611473670974873151 ) ) ;
#112650 = LINE ( 'NONE', #62903, #37734 ) ;
#112651 = CONICAL_SURFACE ( 'NONE', #49979, 0.1000000000000002554, 0.003490658503988666988 ) ;
#112652 = AXIS2_PLACEMENT_3D ( 'NONE', #99750, #100385, #231 ) ;
#112653 = ORIENTED_EDGE ( 'NONE', *, *, #62863, .F. ) ;
#112654 = CARTESIAN_POINT ( 'NONE',  ( -6.650000000000014566, 2.500000000000000000, 6.395190528383296602 ) ) ;
#112655 = FACE_OUTER_BOUND ( 'NONE', #4025, .T. ) ;
#112656 = LINE ( 'NONE', #63562, #6514 ) ;
#112657 = CARTESIAN_POINT ( 'NONE',  ( -2.499999999999996447, 12.50000000000000000, 4.265033745738159077 ) ) ;
#112658 = AXIS2_PLACEMENT_3D ( 'NONE', #40192, #90567, #80115 ) ;
#112659 = AXIS2_PLACEMENT_3D ( 'NONE', #86995, #7786, #98738 ) ;
#112660 = EDGE_CURVE ( 'NONE', #10182, #18164, #58255, .T. ) ;
#112661 = AXIS2_PLACEMENT_3D ( 'NONE', #46259, #96632, #35806 ) ;
#112662 = CARTESIAN_POINT ( 'NONE',  ( 4.399999999999940847, 12.50000000000000000, -4.676537180435977881 ) ) ;
#112663 = ORIENTED_EDGE ( 'NONE', *, *, #107782, .F. ) ;
#112664 = ORIENTED_EDGE ( 'NONE', *, *, #117003, .F. ) ;
#112665 = EDGE_CURVE ( 'NONE', #66158, #62754, #81117, .T. ) ;
#112666 = CARTESIAN_POINT ( 'NONE',  ( 187.2083333333333712, -4.445597072760123503, -7.699999999999989519 ) ) ;
#112667 = DIRECTION ( 'NONE',  ( 0.000000000000000000, -0.9999939076577903929, 0.003490651415223739937 ) ) ;
#112669 = EDGE_CURVE ( 'NONE', #51184, #37790, #124868, .T. ) ;
#112668 = CIRCLE ( 'NONE', #120986, 0.1000000000000002554 ) ;
#112670 = CARTESIAN_POINT ( 'NONE',  ( -12.04999999999999538, 2.500000000000000000, 2.265063509461097357 ) ) ;
#112671 = DIRECTION ( 'NONE',  ( 0.000000000000000000, -0.9999939076577903929, 0.003490651415223739937 ) ) ;
#112672 = CIRCLE ( 'NONE', #56219, 0.06509327318403745899 ) ;
#112673 = ORIENTED_EDGE ( 'NONE', *, *, #109998, .F. ) ;
#112674 = ADVANCED_FACE ( 'NONE', ( #61485 ), #79187, .T. ) ;
#112675 = ADVANCED_FACE ( 'NONE', ( #91569 ), #45462, .T. ) ;
#112676 = VERTEX_POINT ( 'NONE', #60195 ) ;
#112677 = DIRECTION ( 'NONE',  ( 0.000000000000000000, -0.000000000000000000, 1.000000000000000000 ) ) ;
#112678 = CARTESIAN_POINT ( 'NONE',  ( 2.949999999999946887, 12.50000000000000000, -6.495190528383302464 ) ) ;
#112679 = EDGE_CURVE ( 'NONE', #93582, #59583, #62181, .T. ) ;
#112680 = CARTESIAN_POINT ( 'NONE',  ( 3.349999999999945466, 2.500000000000000000, -2.165063509461101710 ) ) ;
#112681 = DIRECTION ( 'NONE',  ( 0.000000000000000000, 0.000000000000000000, -1.000000000000000000 ) ) ;
#112682 = ORIENTED_EDGE ( 'NONE', *, *, #74352, .F. ) ;
#112683 = AXIS2_PLACEMENT_3D ( 'NONE', #57846, #10026, #66988 ) ;
#112684 = DIRECTION ( 'NONE',  ( 0.000000000000000000, 1.000000000000000000, 0.000000000000000000 ) ) ;
#112685 = ADVANCED_FACE ( 'NONE', ( #29435 ), #99832, .T. ) ;
#112686 = PLANE ( 'NONE',  #82890 ) ;
#112687 = AXIS2_PLACEMENT_3D ( 'NONE', #105872, #55486, #85582 ) ;
#112688 = VERTEX_POINT ( 'NONE', #99469 ) ;
#112689 = CARTESIAN_POINT ( 'NONE',  ( 4.149999999999938183, 12.50000000000000000, 7.253104124594885960 ) ) ;
#112690 = EDGE_LOOP ( 'NONE', ( #55160, #27250 ) ) ;
#112691 = EDGE_CURVE ( 'NONE', #34777, #9531, #83105, .T. ) ;
#112692 = FACE_OUTER_BOUND ( 'NONE', #88170, .T. ) ;
#112693 = ORIENTED_EDGE ( 'NONE', *, *, #42513, .T. ) ;
#112694 = CONICAL_SURFACE ( 'NONE', #56248, 0.09999999999999982514, 0.003490658503988666988 ) ;
#112695 = DIRECTION ( 'NONE',  ( 0.000000000000000000, 0.000000000000000000, -1.000000000000000000 ) ) ;
#112696 = CARTESIAN_POINT ( 'NONE',  ( 1.649999999999951505, 2.500000000000000000, 2.957883832488649389 ) ) ;
#112697 = ORIENTED_EDGE ( 'NONE', *, *, #69353, .T. ) ;
#112698 = ORIENTED_EDGE ( 'NONE', *, *, #50755, .T. ) ;
#112699 = CARTESIAN_POINT ( 'NONE',  ( 186.4218750003414016, 0.000000000000000000, 7.564683531250000925 ) ) ;
#112700 = FACE_OUTER_BOUND ( 'NONE', #58418, .T. ) ;
#112701 = CONICAL_SURFACE ( 'NONE', #56156, 0.1000000000000002554, 0.003490658503988666988 ) ;
#112702 = CARTESIAN_POINT ( 'NONE',  ( 6.849999999999929479, 2.500000000000000000, 6.148780366869520009 ) ) ;
#112703 = CARTESIAN_POINT ( 'NONE',  ( 183.8593750003413732, 0.000000000000000000, 7.564683531250000925 ) ) ;
#112704 = VECTOR ( 'NONE', #70011, 1000.000000000000000 ) ;
#112705 = DIRECTION ( 'NONE',  ( 0.000000000000000000, 0.000000000000000000, 1.000000000000000000 ) ) ;
#112706 = FACE_OUTER_BOUND ( 'NONE', #127096, .T. ) ;
#112707 = CARTESIAN_POINT ( 'NONE',  ( 2.499999999999948930, 12.50000000000000000, -4.957854068765716882 ) ) ;
#112708 = CARTESIAN_POINT ( 'NONE',  ( 6.649999999999929301, 12.50000000000000000, 6.495190528383297135 ) ) ;
#112709 = CARTESIAN_POINT ( 'NONE',  ( 14.39999999999989555, 2.500000000000000000, 0.3464101615137736845 ) ) ;
#112710 = AXIS2_PLACEMENT_3D ( 'NONE', #111608, #103733, #45465 ) ;
#112711 = ORIENTED_EDGE ( 'NONE', *, *, #42330, .F. ) ;
#112712 = ORIENTED_EDGE ( 'NONE', *, *, #5829, .T. ) ;
#112713 = CARTESIAN_POINT ( 'NONE',  ( 6.449999999999931788, 12.50000000000000000, -2.511473670974877948 ) ) ;
#112715 = AXIS2_PLACEMENT_3D ( 'NONE', #40581, #51677, #19626 ) ;
#112714 = CONICAL_SURFACE ( 'NONE', #93838, 0.09999999999999999167, 0.003490658503988666988 ) ;
#112716 = EDGE_LOOP ( 'NONE', ( #4411, #51713 ) ) ;
#112717 = CARTESIAN_POINT ( 'NONE',  ( 187.4583333333333428, 4.445597072760117285, 7.700000000000001066 ) ) ;
#112718 = DIRECTION ( 'NONE',  ( 0.000000000000000000, 1.000000000000000000, 0.000000000000000000 ) ) ;
#112719 = FACE_OUTER_BOUND ( 'NONE', #8701, .T. ) ;
#112720 = AXIS2_PLACEMENT_3D ( 'NONE', #21259, #9518, #981 ) ;
#112722 = ORIENTED_EDGE ( 'NONE', *, *, #88239, .T. ) ;
#112721 = ORIENTED_EDGE ( 'NONE', *, *, #109089, .F. ) ;
#112723 = FACE_BOUND ( 'NONE', #45534, .T. ) ;
#112724 = ORIENTED_EDGE ( 'NONE', *, *, #4997, .F. ) ;
#112725 = DIRECTION ( 'NONE',  ( -0.000000000000000000, 1.000000000000000000, -0.000000000000000000 ) ) ;
#112726 = CARTESIAN_POINT ( 'NONE',  ( -7.300000000000013145, 12.50000000000000000, 3.983716857408420076 ) ) ;
#112727 = CARTESIAN_POINT ( 'NONE',  ( -3.150000000000029221, 12.50000000000000000, 2.511473670974873507 ) ) ;
#112730 = CARTESIAN_POINT ( 'NONE',  ( -0.8500000000000395017, 2.500000000000000000, 2.165063509461097713 ) ) ;
#112729 = CONICAL_SURFACE ( 'NONE', #56275, 0.1000000000000002554, 0.003490658503988666988 ) ;
#112728 = CIRCLE ( 'NONE', #77124, 0.09999999999999982514 ) ;
#112731 = EDGE_CURVE ( 'NONE', #33136, #19384, #114478, .T. ) ;
#112732 = DIRECTION ( 'NONE',  ( 0.000000000000000000, 0.000000000000000000, 1.000000000000000000 ) ) ;
#112733 = DIRECTION ( 'NONE',  ( 0.000000000000000000, 0.000000000000000000, 1.000000000000000000 ) ) ;
#112734 = DIRECTION ( 'NONE',  ( -0.000000000000000000, -1.000000000000000000, -0.000000000000000000 ) ) ;
#112735 = CARTESIAN_POINT ( 'NONE',  ( -15.19999999999998153, 2.500000000000000000, -0.2464101615137759549 ) ) ;
#112736 = DIRECTION ( 'NONE',  ( -0.000000000000000000, -1.000000000000000000, -0.000000000000000000 ) ) ;
#112737 = LINE ( 'NONE', #121259, #127893 ) ;
#112738 = DIRECTION ( 'NONE',  ( -0.000000000000000000, -1.000000000000000000, -0.000000000000000000 ) ) ;
#112739 = EDGE_CURVE ( 'NONE', #30668, #119878, #82374, .T. ) ;
#112740 = ORIENTED_EDGE ( 'NONE', *, *, #119028, .T. ) ;
#112741 = EDGE_LOOP ( 'NONE', ( #16903, #81301 ) ) ;
#112742 = VERTEX_POINT ( 'NONE', #79811 ) ;
#112743 = CARTESIAN_POINT ( 'NONE',  ( 10.84999999999991260, 2.500000000000000000, 5.802370205355744659 ) ) ;
#112744 = ORIENTED_EDGE ( 'NONE', *, *, #102174, .T. ) ;
#112745 = CONICAL_SURFACE ( 'NONE', #29127, 0.1000000000000002554, 0.003490658503988666988 ) ;
#112746 = CARTESIAN_POINT ( 'NONE',  ( -0.4000000000000392131, 2.500000000000000000, -5.022947341949754119 ) ) ;
#112748 = EDGE_LOOP ( 'NONE', ( #61449, #59925 ) ) ;
#112747 = EDGE_LOOP ( 'NONE', ( #81672, #104213 ) ) ;
#112749 = ORIENTED_EDGE ( 'NONE', *, *, #52360, .T. ) ;
#112750 = FACE_OUTER_BOUND ( 'NONE', #67468, .T. ) ;
#112751 = CONICAL_SURFACE ( 'NONE', #110673, 0.09999999999999982514, 0.003490658503988666988 ) ;
#112752 = AXIS2_PLACEMENT_3D ( 'NONE', #128909, #126953, #88283 ) ;
#112753 = DIRECTION ( 'NONE',  ( 0.000000000000000000, -0.000000000000000000, 1.000000000000000000 ) ) ;
#112754 = CARTESIAN_POINT ( 'NONE',  ( 13.74999999999989875, 2.500000000000000000, 1.472243186433545459 ) ) ;
#112755 = DIRECTION ( 'NONE',  ( -0.000000000000000000, 1.000000000000000000, -0.000000000000000000 ) ) ;
#112756 = LINE ( 'NONE', #2143, #30846 ) ;
#112757 = ORIENTED_EDGE ( 'NONE', *, *, #51665, .F. ) ;
#112758 = VECTOR ( 'NONE', #82032, 1000.000000000000000 ) ;
#112760 = CARTESIAN_POINT ( 'NONE',  ( 13.94999999999989626, 12.50000000000000000, 2.446380397790835826 ) ) ;
#112759 = CONICAL_SURFACE ( 'NONE', #52118, 0.09999999999999982514, 0.003490658503988666988 ) ;
#112761 = ORIENTED_EDGE ( 'NONE', *, *, #99411, .F. ) ;
#112762 = VECTOR ( 'NONE', #78635, 1000.000000000000000 ) ;
#112763 = EDGE_LOOP ( 'NONE', ( #28853, #78456 ) ) ;
#112764 = ORIENTED_EDGE ( 'NONE', *, *, #119597, .F. ) ;
#112765 = DIRECTION ( 'NONE',  ( -0.000000000000000000, 1.000000000000000000, -0.000000000000000000 ) ) ;
#112766 = ORIENTED_EDGE ( 'NONE', *, *, #18952, .T. ) ;
#112767 = EDGE_LOOP ( 'NONE', ( #6297, #28633, #8022, #96027 ) ) ;
#112768 = ORIENTED_EDGE ( 'NONE', *, *, #126486, .T. ) ;
#112769 = AXIS2_PLACEMENT_3D ( 'NONE', #38151, #97704, #37519 ) ;
#112770 = CARTESIAN_POINT ( 'NONE',  ( -5.200000000000022382, 2.500000000000000000, 4.776537180435972196 ) ) ;
#112772 = ADVANCED_FACE ( 'NONE', ( #98796 ), #51020, .T. ) ;
#112771 = CONICAL_SURFACE ( 'NONE', #83525, 0.09999999999999982514, 0.003490658503988666988 ) ;
#112773 = DIRECTION ( 'NONE',  ( 0.000000000000000000, -0.9999939076577903929, 0.003490651415223739937 ) ) ;
#112774 = DIRECTION ( 'NONE',  ( 0.000000000000000000, 0.000000000000000000, -1.000000000000000000 ) ) ;
#112775 = CIRCLE ( 'NONE', #56312, 0.06509327318403745899 ) ;
#112776 = LINE ( 'NONE', #34873, #94457 ) ;
#112777 = LINE ( 'NONE', #35508, #82249 ) ;
#112778 = DIRECTION ( 'NONE',  ( 0.000000000000000000, -0.9999939076577903929, 0.003490651415223739937 ) ) ;
#112779 = EDGE_CURVE ( 'NONE', #21147, #92182, #70575, .T. ) ;
#112780 = EDGE_LOOP ( 'NONE', ( #107964, #78214 ) ) ;
#112781 = DIRECTION ( 'NONE',  ( 0.000000000000000000, 0.000000000000000000, 1.000000000000000000 ) ) ;
#112782 = VERTEX_POINT ( 'NONE', #119728 ) ;
#112783 = CARTESIAN_POINT ( 'NONE',  ( 5.799999999999931433, 2.500000000000000000, 4.230127018922196669 ) ) ;
#112784 = AXIS2_PLACEMENT_3D ( 'NONE', #28608, #128759, #27954 ) ;
#112785 = VERTEX_POINT ( 'NONE', #30094 ) ;
#112787 = ADVANCED_FACE ( 'NONE', ( #100729 ), #109931, .T. ) ;
#112786 = CARTESIAN_POINT ( 'NONE',  ( -6.450000000000016165, 12.50000000000000000, 2.511473670974873507 ) ) ;
#112788 = EDGE_CURVE ( 'NONE', #7747, #80502, #18335, .T. ) ;
#112789 = ORIENTED_EDGE ( 'NONE', *, *, #51523, .T. ) ;
#112790 = CARTESIAN_POINT ( 'NONE',  ( 183.9427083336747160, -6.551208109652278289, 3.782341765624995134 ) ) ;
#112791 = EDGE_CURVE ( 'NONE', #7975, #112855, #1257, .T. ) ;
#112792 = FACE_OUTER_BOUND ( 'NONE', #95615, .T. ) ;
#112793 = ORIENTED_EDGE ( 'NONE', *, *, #72879, .F. ) ;
#112794 = ORIENTED_EDGE ( 'NONE', *, *, #81648, .T. ) ;
#112795 = CARTESIAN_POINT ( 'NONE',  ( 15.19999999999989093, 2.500000000000000000, 0.4464101615137735513 ) ) ;
#112796 = DIRECTION ( 'NONE',  ( 0.000000000000000000, 0.000000000000000000, 1.000000000000000000 ) ) ;
#112797 = EDGE_CURVE ( 'NONE', #38962, #118209, #63402, .T. ) ;
#112798 = DIRECTION ( 'NONE',  ( -0.000000000000000000, 1.000000000000000000, -0.000000000000000000 ) ) ;
#112800 = CIRCLE ( 'NONE', #8224, 0.06509327318403745899 ) ;
#112799 = DIRECTION ( 'NONE',  ( 0.000000000000000000, -0.9999939076577903929, 0.003490651415223739937 ) ) ;
#112801 = DIRECTION ( 'NONE',  ( 0.000000000000000000, 0.000000000000000000, 1.000000000000000000 ) ) ;
#112802 = EDGE_LOOP ( 'NONE', ( #13975, #45873 ) ) ;
#112803 = CARTESIAN_POINT ( 'NONE',  ( -4.150000000000028777, 12.50000000000000000, -5.802370205355749988 ) ) ;
#112804 = AXIS2_PLACEMENT_3D ( 'NONE', #66369, #106298, #56542 ) ;
#112805 = ORIENTED_EDGE ( 'NONE', *, *, #115264, .T. ) ;
#112806 = DIRECTION ( 'NONE',  ( 0.000000000000000000, 0.000000000000000000, 1.000000000000000000 ) ) ;
#112807 = CARTESIAN_POINT ( 'NONE',  ( 9.199999999999919353, 2.500000000000000000, -2.276824562219559311E-15 ) ) ;
#112809 = CIRCLE ( 'NONE', #89809, 0.06509327318403745899 ) ;
#112808 = CIRCLE ( 'NONE', #66727, 0.1000000000000002554 ) ;
#112810 = AXIS2_PLACEMENT_3D ( 'NONE', #124626, #12718, #4829 ) ;
#112811 = CARTESIAN_POINT ( 'NONE',  ( 184.6302083336747444, -4.367472073101514418, -7.564683531250002702 ) ) ;
#112812 = DIRECTION ( 'NONE',  ( 0.000000000000000000, 1.000000000000000000, 0.000000000000000000 ) ) ;
#112813 = FACE_OUTER_BOUND ( 'NONE', #120868, .T. ) ;
#112814 = CARTESIAN_POINT ( 'NONE',  ( 9.999999999999916511, 2.500000000000000000, -0.6928203230275541413 ) ) ;
#112815 = DIRECTION ( 'NONE',  ( 0.000000000000000000, 0.000000000000000000, 1.000000000000000000 ) ) ;
#112816 = VERTEX_POINT ( 'NONE', #12356 ) ;
#112818 = VECTOR ( 'NONE', #112671, 1000.000000000000000 ) ;
#112817 = CIRCLE ( 'NONE', #18718, 0.06509327318403741736 ) ;
#112819 = FACE_OUTER_BOUND ( 'NONE', #37462, .T. ) ;
#112820 = ADVANCED_FACE ( 'NONE', ( #64680 ), #51807, .T. ) ;
#112821 = CARTESIAN_POINT ( 'NONE',  ( -2.900000000000029221, 2.500000000000000000, -0.7928203230275542301 ) ) ;
#112822 = CARTESIAN_POINT ( 'NONE',  ( -2.700000000000030820, 12.50000000000000000, 0.3464101615137735735 ) ) ;
#112823 = ORIENTED_EDGE ( 'NONE', *, *, #111622, .T. ) ;
#112824 = EDGE_CURVE ( 'NONE', #67674, #100903, #5109, .T. ) ;
#112825 = DIRECTION ( 'NONE',  ( 0.000000000000000000, 0.000000000000000000, 1.000000000000000000 ) ) ;
#112826 = ORIENTED_EDGE ( 'NONE', *, *, #101609, .T. ) ;
#112827 = EDGE_LOOP ( 'NONE', ( #129507, #22385 ) ) ;
#112828 = DIRECTION ( 'NONE',  ( -0.000000000000000000, 1.000000000000000000, -0.000000000000000000 ) ) ;
#112829 = EDGE_CURVE ( 'NONE', #63919, #108022, #62766, .T. ) ;
#112830 = EDGE_LOOP ( 'NONE', ( #91249, #4084, #51755, #21507 ) ) ;
#112831 = CARTESIAN_POINT ( 'NONE',  ( 20.37025966759390272, -0.6621301594381256983, -4.188616773932661630 ) ) ;
#112832 = DIRECTION ( 'NONE',  ( 0.000000000000000000, -0.000000000000000000, 1.000000000000000000 ) ) ;
#112833 = EDGE_CURVE ( 'NONE', #47021, #10500, #3768, .T. ) ;
#112834 = DIRECTION ( 'NONE',  ( -4.274815082592931898E-19, -0.9999939076577903929, -0.003490651415223739937 ) ) ;
#112835 = ADVANCED_FACE ( 'NONE', ( #24771 ), #35085, .T. ) ;
#112836 = ORIENTED_EDGE ( 'NONE', *, *, #12052, .F. ) ;
#112837 = LINE ( 'NONE', #93837, #69668 ) ;
#112838 = CIRCLE ( 'NONE', #14521, 0.06509327318403745899 ) ;
#112839 = EDGE_CURVE ( 'NONE', #128265, #28777, #122907, .T. ) ;
#112840 = DIRECTION ( 'NONE',  ( 0.000000000000000000, 0.000000000000000000, 1.000000000000000000 ) ) ;
#112841 = ORIENTED_EDGE ( 'NONE', *, *, #81343, .T. ) ;
#112844 = EDGE_CURVE ( 'NONE', #42007, #70518, #55983, .T. ) ;
#112843 = VECTOR ( 'NONE', #85212, 1000.000000000000000 ) ;
#112842 = AXIS2_PLACEMENT_3D ( 'NONE', #20691, #40338, #71073 ) ;
#112845 = EDGE_CURVE ( 'NONE', #40379, #42733, #87289, .T. ) ;
#112846 = VERTEX_POINT ( 'NONE', #122336 ) ;
#112847 = ORIENTED_EDGE ( 'NONE', *, *, #16005, .F. ) ;
#112848 = CARTESIAN_POINT ( 'NONE',  ( 0.8499999999999553468, 2.500000000000000000, 1.372243186433545370 ) ) ;
#112849 = CARTESIAN_POINT ( 'NONE',  ( 6.649999999999927525, 12.50000000000000000, 2.165063509461097713 ) ) ;
#112850 = DIRECTION ( 'NONE',  ( 0.000000000000000000, 0.000000000000000000, 1.000000000000000000 ) ) ;
#112851 = ORIENTED_EDGE ( 'NONE', *, *, #3332, .T. ) ;
#112852 = CIRCLE ( 'NONE', #41768, 0.1000000000000000056 ) ;
#112853 = CARTESIAN_POINT ( 'NONE',  ( 4.999999999999935163, 12.50000000000000000, 0.6928203230275494784 ) ) ;
#112854 = DIRECTION ( 'NONE',  ( 0.000000000000000000, 0.000000000000000000, 1.000000000000000000 ) ) ;
#112855 = VERTEX_POINT ( 'NONE', #124258 ) ;
#112857 = CARTESIAN_POINT ( 'NONE',  ( -0.8500000000000386136, 2.500000000000000000, 5.702370205355745014 ) ) ;
#112856 = CONICAL_SURFACE ( 'NONE', #52308, 0.1000000000000002554, 0.003490658503988666988 ) ;
#112858 = CARTESIAN_POINT ( 'NONE',  ( -10.65000000000000213, 2.500000000000000000, 6.048780366869520364 ) ) ;
#112859 = CIRCLE ( 'NONE', #81557, 0.5000000000000004441 ) ;
#112860 = DIRECTION ( 'NONE',  ( 0.000000000000000000, 0.000000000000000000, 1.000000000000000000 ) ) ;
#112861 = DIRECTION ( 'NONE',  ( 0.000000000000000000, -0.9999939076577903929, 0.003490651415223739937 ) ) ;
#112862 = CARTESIAN_POINT ( 'NONE',  ( 1.449999999999951328, 2.500000000000000000, -1.818653347947326138 ) ) ;
#112863 = DIRECTION ( 'NONE',  ( -0.000000000000000000, 1.000000000000000000, -0.000000000000000000 ) ) ;
#112864 = DIRECTION ( 'NONE',  ( 0.000000000000000000, 0.000000000000000000, 1.000000000000000000 ) ) ;
#112865 = AXIS2_PLACEMENT_3D ( 'NONE', #4421, #104585, #24744 ) ;
#112866 = ORIENTED_EDGE ( 'NONE', *, *, #24179, .F. ) ;
#112867 = ORIENTED_EDGE ( 'NONE', *, *, #109950, .T. ) ;
#112868 = ORIENTED_EDGE ( 'NONE', *, *, #66583, .F. ) ;
#112869 = VERTEX_POINT ( 'NONE', #3204 ) ;
#112870 = CIRCLE ( 'NONE', #58513, 0.06509327318403745899 ) ;
#112871 = CARTESIAN_POINT ( 'NONE',  ( -1.900000000000034994, 12.50000000000000000, -0.4115034346978157509 ) ) ;
#112872 = DIRECTION ( 'NONE',  ( 0.000000000000000000, 0.000000000000000000, -1.000000000000000000 ) ) ;
#112873 = DIRECTION ( 'NONE',  ( -0.000000000000000000, 1.000000000000000000, -0.000000000000000000 ) ) ;
#112874 = VERTEX_POINT ( 'NONE', #3831 ) ;
#112875 = FACE_BOUND ( 'NONE', #36956, .T. ) ;
#112876 = DIRECTION ( 'NONE',  ( 0.000000000000000000, 1.000000000000000000, 0.000000000000000000 ) ) ;
#112877 = CARTESIAN_POINT ( 'NONE',  ( 10.64999999999990976, 12.50000000000000000, -6.776507416713039689 ) ) ;
#112878 = CARTESIAN_POINT ( 'NONE',  ( 9.349999999999916156, 2.500000000000000000, 6.148780366869520009 ) ) ;
#112879 = EDGE_CURVE ( 'NONE', #88979, #80302, #20505, .T. ) ;
#112880 = DIRECTION ( 'NONE',  ( 0.000000000000000000, 0.000000000000000000, 1.000000000000000000 ) ) ;
#112881 = DIRECTION ( 'NONE',  ( 0.000000000000000000, 0.000000000000000000, 1.000000000000000000 ) ) ;
#112882 = CARTESIAN_POINT ( 'NONE',  ( 185.3333333333333144, 6.668395609140177704, -3.849999999999998312 ) ) ;
#112884 = LINE ( 'NONE', #20643, #12051 ) ;
#112883 =( BOUNDED_CURVE ( )  B_SPLINE_CURVE ( 2, ( #67154, #99243, #58669 ),
 .UNSPECIFIED., .F., .F. ) 
 B_SPLINE_CURVE_WITH_KNOTS ( ( 3, 3 ),
 ( 0.000000000000000000, 0.01487798352592973813 ),
 .UNSPECIFIED. ) 
 CURVE ( )  GEOMETRIC_REPRESENTATION_ITEM ( )  RATIONAL_B_SPLINE_CURVE ( ( 0.8943752373141968803, 0.7762344340431478473, 1.000000000000000000 ) ) 
 REPRESENTATION_ITEM ( '' )  );
#112885 = CARTESIAN_POINT ( 'NONE',  ( 0.8499999999999545697, 12.50000000000000000, 2.857883832488649301 ) ) ;
#112886 = DIRECTION ( 'NONE',  ( 0.000000000000000000, 0.000000000000000000, 1.000000000000000000 ) ) ;
#112887 = ORIENTED_EDGE ( 'NONE', *, *, #2807, .F. ) ;
#112888 = ADVANCED_FACE ( 'NONE', ( #14283 ), #93764, .T. ) ;
#112889 = EDGE_LOOP ( 'NONE', ( #33391, #35229 ) ) ;
#112890 = ORIENTED_EDGE ( 'NONE', *, *, #91263, .F. ) ;
#112891 = ORIENTED_EDGE ( 'NONE', *, *, #117518, .F. ) ;
#112892 = ORIENTED_EDGE ( 'NONE', *, *, #105051, .F. ) ;
#112893 = ORIENTED_EDGE ( 'NONE', *, *, #12470, .F. ) ;
#112894 = CARTESIAN_POINT ( 'NONE',  ( 12.09999999999990550, 2.500000000000000000, 4.922947341949748257 ) ) ;
#112895 = VECTOR ( 'NONE', #54301, 1000.000000000000000 ) ;
#112896 = EDGE_LOOP ( 'NONE', ( #55245, #104171, #35376, #102044 ) ) ;
#112897 = ORIENTED_EDGE ( 'NONE', *, *, #19225, .F. ) ;
#112899 = AXIS2_PLACEMENT_3D ( 'NONE', #39628, #70344, #108329 ) ;
#112898 = AXIS2_PLACEMENT_3D ( 'NONE', #38276, #38946, #88655 ) ;
#112900 = CARTESIAN_POINT ( 'NONE',  ( 6.249999999999928946, 12.50000000000000000, 2.922977105672686982 ) ) ;
#112901 = DIRECTION ( 'NONE',  ( 0.000000000000000000, 0.000000000000000000, 1.000000000000000000 ) ) ;
#112902 = CARTESIAN_POINT ( 'NONE',  ( 12.49999999999990408, 2.500000000000000000, 4.922947341949748257 ) ) ;
#112903 = EDGE_LOOP ( 'NONE', ( #51429, #73704 ) ) ;
#112904 = DIRECTION ( 'NONE',  ( -0.000000000000000000, 1.000000000000000000, -0.000000000000000000 ) ) ;
#112906 = CIRCLE ( 'NONE', #39485, 0.1000000000000000472 ) ;
#112905 = CONICAL_SURFACE ( 'NONE', #23, 0.1000000000000000472, 0.003490658503988666988 ) ;
#112907 = ORIENTED_EDGE ( 'NONE', *, *, #5060, .T. ) ;
#112908 = ORIENTED_EDGE ( 'NONE', *, *, #116429, .F. ) ;
#112909 = PLANE ( 'NONE',  #96989 ) ;
#112910 = CARTESIAN_POINT ( 'NONE',  ( -12.04999999999999716, 2.500000000000000000, -2.165063509461097713 ) ) ;
#112911 = ORIENTED_EDGE ( 'NONE', *, *, #100483, .F. ) ;
#112912 = ORIENTED_EDGE ( 'NONE', *, *, #70288, .F. ) ;
#112913 = CARTESIAN_POINT ( 'NONE',  ( 14.14999999999989200, 12.50000000000000000, -2.230156782645139391 ) ) ;
#112914 = DIRECTION ( 'NONE',  ( -0.000000000000000000, -1.000000000000000000, -0.000000000000000000 ) ) ;
#112915 = DIRECTION ( 'NONE',  ( -4.274815082592931898E-19, -0.9999939076577903929, -0.003490651415223739937 ) ) ;
#112916 = CARTESIAN_POINT ( 'NONE',  ( -13.94999999999998863, 2.500000000000000000, 2.511473670974877503 ) ) ;
#112917 = DIRECTION ( 'NONE',  ( 0.000000000000000000, -0.000000000000000000, 1.000000000000000000 ) ) ;
#112918 = ORIENTED_EDGE ( 'NONE', *, *, #94990, .F. ) ;
#112919 = CARTESIAN_POINT ( 'NONE',  ( 6.598553918464069135, -2.499999999999999556, 8.770211965307140645 ) ) ;
#112920 = VECTOR ( 'NONE', #54951, 1000.000000000000000 ) ;
#112921 = EDGE_CURVE ( 'NONE', #94312, #121167, #91504, .T. ) ;
#112922 = AXIS2_PLACEMENT_3D ( 'NONE', #58495, #69572, #67632 ) ;
#112923 = ORIENTED_EDGE ( 'NONE', *, *, #24906, .T. ) ;
#112924 = CARTESIAN_POINT ( 'NONE',  ( 87.50000000000002842, 7.402262750143060899, -1.385127402881716430 ) ) ;
#112925 = ORIENTED_EDGE ( 'NONE', *, *, #47669, .F. ) ;
#112926 = CARTESIAN_POINT ( 'NONE',  ( 5.599999999999931255, 2.500000000000000000, 3.983716857408420076 ) ) ;
#112927 = CARTESIAN_POINT ( 'NONE',  ( 13.94999999999989804, 2.500000000000000000, 1.718653347947321386 ) ) ;
#112929 = ADVANCED_FACE ( 'NONE', ( #107175 ), #124952, .T. ) ;
#112928 = DIRECTION ( 'NONE',  ( 0.000000000000000000, 0.000000000000000000, 1.000000000000000000 ) ) ;
#112930 = CARTESIAN_POINT ( 'NONE',  ( -12.49999999999999467, 2.500000000000000000, -3.537306695894647302 ) ) ;
#112931 = EDGE_CURVE ( 'NONE', #10496, #46288, #26696, .T. ) ;
#112932 = EDGE_LOOP ( 'NONE', ( #103900, #124693 ) ) ;
#112933 = CIRCLE ( 'NONE', #2103, 0.06509327318403745899 ) ;
#112934 = CARTESIAN_POINT ( 'NONE',  ( -10.85000000000000142, 2.500000000000000000, -2.265063509461097802 ) ) ;
#112935 = EDGE_CURVE ( 'NONE', #13848, #77485, #5741, .T. ) ;
#112936 = CARTESIAN_POINT ( 'NONE',  ( -8.150000000000012790, 12.50000000000000000, -1.818653347947326138 ) ) ;
#112937 = EDGE_LOOP ( 'NONE', ( #85144, #45960, #46101, #114274 ) ) ;
#112938 = EDGE_CURVE ( 'NONE', #77431, #9926, #105902, .T. ) ;
#112939 = ORIENTED_EDGE ( 'NONE', *, *, #112921, .F. ) ;
#112940 = ORIENTED_EDGE ( 'NONE', *, *, #16974, .T. ) ;
#112941 = DIRECTION ( 'NONE',  ( -0.000000000000000000, 1.000000000000000000, -0.000000000000000000 ) ) ;
#112942 = DIRECTION ( 'NONE',  ( 0.000000000000000000, 0.000000000000000000, -1.000000000000000000 ) ) ;
#112943 = EDGE_CURVE ( 'NONE', #21757, #125307, #26750, .T. ) ;
#112944 = CARTESIAN_POINT ( 'NONE',  ( 186.0677083336747444, -4.367472073101514418, -7.564683531250002702 ) ) ;
#112945 = CIRCLE ( 'NONE', #62780, 0.1000000000000002554 ) ;
#112946 = FACE_OUTER_BOUND ( 'NONE', #68623, .T. ) ;
#112947 = DIRECTION ( 'NONE',  ( 0.000000000000000000, 0.000000000000000000, 1.000000000000000000 ) ) ;
#112948 = AXIS2_PLACEMENT_3D ( 'NONE', #45842, #56288, #66113 ) ;
#112949 = AXIS2_PLACEMENT_3D ( 'NONE', #36543, #33954, #3838 ) ;
#112950 = CARTESIAN_POINT ( 'NONE',  ( -12.89999999999999325, 12.50000000000000000, 0.6277270498435161272 ) ) ;
#112951 = DIRECTION ( 'NONE',  ( 1.000000000000000000, 0.000000000000000000, 0.000000000000000000 ) ) ;
#112952 = ORIENTED_EDGE ( 'NONE', *, *, #31132, .T. ) ;
#112953 = DIRECTION ( 'NONE',  ( 0.000000000000000000, 0.000000000000000000, 1.000000000000000000 ) ) ;
#112954 = ORIENTED_EDGE ( 'NONE', *, *, #5844, .T. ) ;
#112955 = CONICAL_SURFACE ( 'NONE', #102494, 0.1000000000000002554, 0.003490658503988666988 ) ;
#112956 = DIRECTION ( 'NONE',  ( 0.000000000000000000, -0.9999939076577903929, 0.003490651415223739937 ) ) ;
#112957 = DIRECTION ( 'NONE',  ( -0.000000000000000000, -1.000000000000000000, -0.000000000000000000 ) ) ;
#112958 = DIRECTION ( 'NONE',  ( 0.000000000000000000, -0.9999939076577903929, 0.003490651415223739937 ) ) ;
#112959 = CARTESIAN_POINT ( 'NONE',  ( -0.6000000000000388356, 2.500000000000000000, 4.676537180435972552 ) ) ;
#112960 = ORIENTED_EDGE ( 'NONE', *, *, #121972, .T. ) ;
#112961 = CARTESIAN_POINT ( 'NONE',  ( -10.45000000000000462, 2.500000000000000000, -6.495190528383298911 ) ) ;
#112962 = DIRECTION ( 'NONE',  ( 0.000000000000000000, 0.000000000000000000, -1.000000000000000000 ) ) ;
#112964 = ORIENTED_EDGE ( 'NONE', *, *, #37156, .T. ) ;
#112963 = CARTESIAN_POINT ( 'NONE',  ( -11.64999999999999680, 2.500000000000000000, 6.495190528383297135 ) ) ;
#112965 = ORIENTED_EDGE ( 'NONE', *, *, #6045, .T. ) ;
#112966 = DIRECTION ( 'NONE',  ( 0.000000000000000000, 0.000000000000000000, -1.000000000000000000 ) ) ;
#112967 = ORIENTED_EDGE ( 'NONE', *, *, #89485, .T. ) ;
#112968 = ORIENTED_EDGE ( 'NONE', *, *, #16112, .F. ) ;
#112969 = CARTESIAN_POINT ( 'NONE',  ( -7.900000000000014566, 2.500000000000000000, -5.022947341949754119 ) ) ;
#112971 = EDGE_CURVE ( 'NONE', #84933, #17899, #24606, .T. ) ;
#112970 = VECTOR ( 'NONE', #91989, 1000.000000000000000 ) ;
#112972 = ADVANCED_FACE ( 'NONE', ( #107831 ), #110371, .T. ) ;
#112973 = VECTOR ( 'NONE', #84242, 1000.000000000000000 ) ;
#112974 = VERTEX_POINT ( 'NONE', #15571 ) ;
#112975 = CARTESIAN_POINT ( 'NONE',  ( -0.6000000000000383915, 12.50000000000000000, -4.741630453620015118 ) ) ;
#112977 = EDGE_CURVE ( 'NONE', #84112, #2963, #1605, .T. ) ;
#112976 = CARTESIAN_POINT ( 'NONE',  ( 8.299999999999922551, 2.500000000000000000, -0.1000000000000023925 ) ) ;
#112978 = DIRECTION ( 'NONE',  ( 0.000000000000000000, 1.000000000000000000, 0.000000000000000000 ) ) ;
#112979 = VERTEX_POINT ( 'NONE', #27982 ) ;
#112980 = CONICAL_SURFACE ( 'NONE', #35632, 0.1000000000000002554, 0.003490658503988666988 ) ;
#112981 = DIRECTION ( 'NONE',  ( 0.000000000000000000, -0.000000000000000000, 1.000000000000000000 ) ) ;
#112983 = VERTEX_POINT ( 'NONE', #47628 ) ;
#112982 = CARTESIAN_POINT ( 'NONE',  ( 10.84999999999991260, 12.50000000000000000, -2.792790559304616504 ) ) ;
#112984 = EDGE_CURVE ( 'NONE', #15707, #125017, #45545, .T. ) ;
#112985 = CARTESIAN_POINT ( 'NONE',  ( 10.19999999999991225, 12.50000000000000000, -4.676537180435978769 ) ) ;
#112986 = ADVANCED_FACE ( 'NONE', ( #116352 ), #16256, .T. ) ;
#112987 = CARTESIAN_POINT ( 'NONE',  ( 186.4479166673494603, -6.668395609140176816, -3.850000000000003642 ) ) ;
#112988 = ADVANCED_FACE ( 'NONE', ( #58097 ), #12075, .T. ) ;
#112989 = VERTEX_POINT ( 'NONE', #21887 ) ;
#112990 = ADVANCED_FACE ( 'NONE', ( #68541 ), #62039, .T. ) ;
#112991 = EDGE_CURVE ( 'NONE', #15146, #97073, #68509, .T. ) ;
#112992 = EDGE_LOOP ( 'NONE', ( #17510, #18554 ) ) ;
#112993 = ORIENTED_EDGE ( 'NONE', *, *, #76470, .T. ) ;
#112994 = EDGE_LOOP ( 'NONE', ( #81440, #80602, #53462, #37801 ) ) ;
#112995 = LINE ( 'NONE', #124748, #37910 ) ;
#112996 = CARTESIAN_POINT ( 'NONE',  ( -10.85000000000000142, 2.500000000000000000, -5.802370205355746435 ) ) ;
#112997 = DIRECTION ( 'NONE',  ( -4.274815082592931898E-19, -0.9999939076577903929, -0.003490651415223739937 ) ) ;
#112998 = FACE_BOUND ( 'NONE', #47254, .T. ) ;
#112999 = EDGE_LOOP ( 'NONE', ( #22252, #57821 ) ) ;
#113000 = CARTESIAN_POINT ( 'NONE',  ( 183.9062500006828031, -8.891194145520236347, -1.633285867636356693E-15 ) ) ;
#113001 = EDGE_CURVE ( 'NONE', #117215, #129515, #21216, .T. ) ;
#113002 = CARTESIAN_POINT ( 'NONE',  ( 6.049999999999934097, 2.500000000000000000, 6.148780366869520897 ) ) ;
#113003 = CARTESIAN_POINT ( 'NONE',  ( -14.34999999999998543, 2.500000000000000000, -2.611473670974875372 ) ) ;
#113004 = CARTESIAN_POINT ( 'NONE',  ( -2.700000000000031264, 2.500000000000000000, 4.676537180435972552 ) ) ;
#113005 = CARTESIAN_POINT ( 'NONE',  ( -10.20000000000000462, 2.500000000000000000, 0.4464101615137735513 ) ) ;
#113006 = DIRECTION ( 'NONE',  ( 0.000000000000000000, 1.000000000000000000, 0.000000000000000000 ) ) ;
#113007 = CONICAL_SURFACE ( 'NONE', #62841, 0.1000000000000000472, 0.003490658503988666988 ) ;
#113008 = CIRCLE ( 'NONE', #23130, 0.06509327318403745899 ) ;
#113009 = CARTESIAN_POINT ( 'NONE',  ( 4.599999999999938360, 12.50000000000000000, -0.7579135962115916003 ) ) ;
#113010 = ORIENTED_EDGE ( 'NONE', *, *, #19553, .F. ) ;
#113011 = VERTEX_POINT ( 'NONE', #11397 ) ;
#113012 = EDGE_LOOP ( 'NONE', ( #34589, #107063, #115088, #63118 ) ) ;
#113013 = VERTEX_POINT ( 'NONE', #101726 ) ;
#113014 = ORIENTED_EDGE ( 'NONE', *, *, #119280, .F. ) ;
#113015 = DIRECTION ( 'NONE',  ( 0.000000000000000000, 1.000000000000000000, 0.000000000000000000 ) ) ;
#113016 = DIRECTION ( 'NONE',  ( 0.000000000000000000, 1.000000000000000000, 0.000000000000000000 ) ) ;
#113017 = ORIENTED_EDGE ( 'NONE', *, *, #36480, .F. ) ;
#113018 = FACE_BOUND ( 'NONE', #123128, .T. ) ;
#113019 = AXIS2_PLACEMENT_3D ( 'NONE', #118936, #105899, #46325 ) ;
#113020 = DIRECTION ( 'NONE',  ( 0.000000000000000000, -0.9999939076577903929, 0.003490651415223739937 ) ) ;
#113021 = VERTEX_POINT ( 'NONE', #41534 ) ;
#113022 = LINE ( 'NONE', #102552, #57878 ) ;
#113023 = DIRECTION ( 'NONE',  ( 0.000000000000000000, 0.000000000000000000, 1.000000000000000000 ) ) ;
#113024 = DIRECTION ( 'NONE',  ( 0.000000000000000000, 0.000000000000000000, 1.000000000000000000 ) ) ;
#113025 = ORIENTED_EDGE ( 'NONE', *, *, #102176, .T. ) ;
#113026 = DIRECTION ( 'NONE',  ( -0.000000000000000000, 1.000000000000000000, -0.000000000000000000 ) ) ;
#113027 = AXIS2_PLACEMENT_3D ( 'NONE', #119723, #129583, #80474 ) ;
#113028 = EDGE_LOOP ( 'NONE', ( #2962, #42412, #32107, #54209 ) ) ;
#113029 = CIRCLE ( 'NONE', #145, 0.06509327318403745899 ) ;
#113030 = EDGE_CURVE ( 'NONE', #78724, #4520, #118687, .T. ) ;
#113031 = ORIENTED_EDGE ( 'NONE', *, *, #109842, .F. ) ;
#113032 = ORIENTED_EDGE ( 'NONE', *, *, #69248, .T. ) ;
#113033 = CARTESIAN_POINT ( 'NONE',  ( -9.350000000000006750, 2.500000000000000000, -2.511473670974877948 ) ) ;
#113034 = DIRECTION ( 'NONE',  ( 0.000000000000000000, 1.000000000000000000, 0.000000000000000000 ) ) ;
#113035 = DIRECTION ( 'NONE',  ( -0.000000000000000000, 1.000000000000000000, -0.000000000000000000 ) ) ;
#113036 = VERTEX_POINT ( 'NONE', #91899 ) ;
#113037 = DIRECTION ( 'NONE',  ( 0.000000000000000000, 0.000000000000000000, -1.000000000000000000 ) ) ;
#113038 = CONICAL_SURFACE ( 'NONE', #127708, 0.1000000000000000472, 0.003490658503988666988 ) ;
#113039 = DIRECTION ( 'NONE',  ( 0.000000000000000000, 0.000000000000000000, -1.000000000000000000 ) ) ;
#113040 = CARTESIAN_POINT ( 'NONE',  ( 9.999999999999916511, 2.500000000000000000, -0.7928203230275542301 ) ) ;
#113041 = VECTOR ( 'NONE', #16074, 1000.000000000000000 ) ;
#113042 = CARTESIAN_POINT ( 'NONE',  ( 186.9895833340161460, -4.445597072760115509, -7.700000000000001954 ) ) ;
#113043 = ORIENTED_EDGE ( 'NONE', *, *, #14966, .T. ) ;
#113044 = CARTESIAN_POINT ( 'NONE',  ( 13.94999999999989448, 2.500000000000000000, -2.511473670974877948 ) ) ;
#113045 = ORIENTED_EDGE ( 'NONE', *, *, #69631, .T. ) ;
#113046 = DIRECTION ( 'NONE',  ( -0.000000000000000000, -1.000000000000000000, -0.000000000000000000 ) ) ;
#113047 = ORIENTED_EDGE ( 'NONE', *, *, #94141, .F. ) ;
#113048 = EDGE_LOOP ( 'NONE', ( #73070, #16643, #107269, #114369 ) ) ;
#113049 = DIRECTION ( 'NONE',  ( 0.000000000000000000, 0.000000000000000000, 1.000000000000000000 ) ) ;
#113050 = DIRECTION ( 'NONE',  ( 0.000000000000000000, 0.000000000000000000, -1.000000000000000000 ) ) ;
#113051 = DIRECTION ( 'NONE',  ( 0.000000000000000000, 0.000000000000000000, 1.000000000000000000 ) ) ;
#113052 = DIRECTION ( 'NONE',  ( -0.000000000000000000, -1.000000000000000000, -0.000000000000000000 ) ) ;
#113053 = DIRECTION ( 'NONE',  ( 0.000000000000000000, 0.000000000000000000, 1.000000000000000000 ) ) ;
#113054 = ORIENTED_EDGE ( 'NONE', *, *, #7799, .T. ) ;
#113055 = ORIENTED_EDGE ( 'NONE', *, *, #54879, .F. ) ;
#113056 = DIRECTION ( 'NONE',  ( 0.000000000000000000, 0.000000000000000000, -1.000000000000000000 ) ) ;
#113057 = CARTESIAN_POINT ( 'NONE',  ( 3.149999999999946176, 2.500000000000000000, -2.411473670974877859 ) ) ;
#113059 = DIRECTION ( 'NONE',  ( -0.000000000000000000, -1.000000000000000000, -0.000000000000000000 ) ) ;
#113058 = AXIS2_PLACEMENT_3D ( 'NONE', #70110, #128406, #119844 ) ;
#113060 = ORIENTED_EDGE ( 'NONE', *, *, #118280, .T. ) ;
#113061 = VERTEX_POINT ( 'NONE', #42156 ) ;
#113062 = CIRCLE ( 'NONE', #58697, 0.09999999999999999167 ) ;
#113063 = DIRECTION ( 'NONE',  ( 0.000000000000000000, 1.000000000000000000, 0.000000000000000000 ) ) ;
#113064 = VERTEX_POINT ( 'NONE', #82741 ) ;
#113065 = FACE_OUTER_BOUND ( 'NONE', #32363, .T. ) ;
#113066 = PLANE ( 'NONE',  #39438 ) ;
#113067 = EDGE_CURVE ( 'NONE', #31853, #31716, #79003, .T. ) ;
#113068 = CONICAL_SURFACE ( 'NONE', #123438, 0.1000000000000000472, 0.003490658503988666988 ) ;
#113069 = DIRECTION ( 'NONE',  ( 0.000000000000000000, 0.000000000000000000, 1.000000000000000000 ) ) ;
#113070 = EDGE_LOOP ( 'NONE', ( #92074, #21817 ) ) ;
#113071 = DIRECTION ( 'NONE',  ( 0.000000000000000000, 0.000000000000000000, 1.000000000000000000 ) ) ;
#113072 = FACE_OUTER_BOUND ( 'NONE', #68689, .T. ) ;
#113073 = CARTESIAN_POINT ( 'NONE',  ( -6.850000000000013856, 2.500000000000000000, 6.841600689897072485 ) ) ;
#113074 = CARTESIAN_POINT ( 'NONE',  ( 9.149999999999916866, 2.500000000000000000, -2.857883832488653741 ) ) ;
#113075 = AXIS2_PLACEMENT_3D ( 'NONE', #101162, #33085, #41613 ) ;
#113076 = EDGE_CURVE ( 'NONE', #56218, #71451, #95764, .T. ) ;
#113077 = DIRECTION ( 'NONE',  ( -1.000000000000000000, -0.000000000000000000, -0.000000000000000000 ) ) ;
#113078 = EDGE_CURVE ( 'NONE', #62072, #94563, #37561, .T. ) ;
#113079 = VERTEX_POINT ( 'NONE', #123921 ) ;
#113080 = CARTESIAN_POINT ( 'NONE',  ( -2.300000000000032685, 2.500000000000000000, -4.676537180435978769 ) ) ;
#113081 = CARTESIAN_POINT ( 'NONE',  ( 21.24754738303277790, -0.7337760880902381988, 4.182111650399363612 ) ) ;
#113082 = ADVANCED_FACE ( 'NONE', ( #25086 ), #73530, .T. ) ;
#113083 = EDGE_LOOP ( 'NONE', ( #99116, #67312, #1279, #26961 ) ) ;
#113084 = EDGE_CURVE ( 'NONE', #120997, #94406, #114892, .T. ) ;
#113085 = ORIENTED_EDGE ( 'NONE', *, *, #8951, .F. ) ;
#113086 = EDGE_CURVE ( 'NONE', #85023, #97932, #123289, .T. ) ;
#113087 = CARTESIAN_POINT ( 'NONE',  ( 186.9635416670080303, -4.367472073101519747, 7.564683531249999149 ) ) ;
#113089 = EDGE_CURVE ( 'NONE', #35141, #45163, #52130, .T. ) ;
#113088 = CARTESIAN_POINT ( 'NONE',  ( 11.44999999999990692, 2.500000000000000000, -6.841600689897078702 ) ) ;
#113090 = ADVANCED_FACE ( 'NONE', ( #63733 ), #125287, .T. ) ;
#113091 = DIRECTION ( 'NONE',  ( 0.000000000000000000, 0.000000000000000000, -1.000000000000000000 ) ) ;
#113092 = DIRECTION ( 'NONE',  ( 0.000000000000000000, 1.000000000000000000, 0.000000000000000000 ) ) ;
#113093 = CARTESIAN_POINT ( 'NONE',  ( -3.350000000000028955, 2.500000000000000000, 5.902370205355745192 ) ) ;
#113094 = CONICAL_SURFACE ( 'NONE', #14864, 0.1000000000000002554, 0.003490658503988666988 ) ;
#113095 = DIRECTION ( 'NONE',  ( 0.000000000000000000, 1.000000000000000000, 0.000000000000000000 ) ) ;
#113096 = DIRECTION ( 'NONE',  ( 0.000000000000000000, 1.000000000000000000, 0.000000000000000000 ) ) ;
#113097 = DIRECTION ( 'NONE',  ( -4.274815082592931898E-19, -0.9999939076577903929, -0.003490651415223739937 ) ) ;
#113098 = DIRECTION ( 'NONE',  ( 0.000000000000000000, -0.000000000000000000, 1.000000000000000000 ) ) ;
#113099 = EDGE_CURVE ( 'NONE', #72352, #114066, #10355, .T. ) ;
#113100 = DIRECTION ( 'NONE',  ( -0.000000000000000000, -1.000000000000000000, -0.000000000000000000 ) ) ;
#113101 = AXIS2_PLACEMENT_3D ( 'NONE', #68673, #18917, #9109 ) ;
#113102 = ORIENTED_EDGE ( 'NONE', *, *, #117054, .T. ) ;
#113103 = ADVANCED_FACE ( 'NONE', ( #85292 ), #43460, .T. ) ;
#113104 = EDGE_LOOP ( 'NONE', ( #32913, #128538 ) ) ;
#113105 = ORIENTED_EDGE ( 'NONE', *, *, #86039, .T. ) ;
#113106 = ORIENTED_EDGE ( 'NONE', *, *, #35834, .F. ) ;
#113107 = CARTESIAN_POINT ( 'NONE',  ( -9.800000000000006040, 12.50000000000000000, 0.3464101615137735735 ) ) ;
#113108 = PLANE ( 'NONE',  #16505 ) ;
#113109 = AXIS2_PLACEMENT_3D ( 'NONE', #126988, #104741, #105414 ) ;
#113110 = CIRCLE ( 'NONE', #27420, 0.1000000000000000472 ) ;
#113111 = ORIENTED_EDGE ( 'NONE', *, *, #82820, .F. ) ;
#113112 = FACE_OUTER_BOUND ( 'NONE', #71999, .T. ) ;
#113113 = DIRECTION ( 'NONE',  ( 0.000000000000000000, 0.000000000000000000, -1.000000000000000000 ) ) ;
#113115 = VERTEX_POINT ( 'NONE', #93832 ) ;
#113114 = CARTESIAN_POINT ( 'NONE',  ( 108.0000000000000142, 8.500000000000000000, 0.000000000000000000 ) ) ;
#113116 = CARTESIAN_POINT ( 'NONE',  ( -0.4500000000000402012, 12.50000000000000000, 2.230156782645134950 ) ) ;
#113117 = CARTESIAN_POINT ( 'NONE',  ( -4.350000000000023626, 12.50000000000000000, -1.818653347947325916 ) ) ;
#113118 = AXIS2_PLACEMENT_3D ( 'NONE', #116343, #56761, #86229 ) ;
#113119 = VERTEX_POINT ( 'NONE', #75469 ) ;
#113120 = CIRCLE ( 'NONE', #73406, 0.06509327318403743123 ) ;
#113121 = ORIENTED_EDGE ( 'NONE', *, *, #112833, .F. ) ;
#113122 = ORIENTED_EDGE ( 'NONE', *, *, #39977, .T. ) ;
#113123 = VERTEX_POINT ( 'NONE', #104914 ) ;
#113124 = DIRECTION ( 'NONE',  ( 0.000000000000000000, 0.000000000000000000, -1.000000000000000000 ) ) ;
#113125 = ADVANCED_FACE ( 'NONE', ( #26390 ), #8288, .T. ) ;
#113126 = AXIS2_PLACEMENT_3D ( 'NONE', #101245, #112361, #122824 ) ;
#113127 = DIRECTION ( 'NONE',  ( -0.000000000000000000, -1.000000000000000000, -0.000000000000000000 ) ) ;
#113129 = EDGE_CURVE ( 'NONE', #71812, #126312, #100252, .T. ) ;
#113128 = DIRECTION ( 'NONE',  ( 0.000000000000000000, 1.000000000000000000, 0.000000000000000000 ) ) ;
#113130 = DIRECTION ( 'NONE',  ( -0.000000000000000000, -1.000000000000000000, -0.000000000000000000 ) ) ;
#113131 = VERTEX_POINT ( 'NONE', #125854 ) ;
#113132 = EDGE_CURVE ( 'NONE', #62174, #93106, #4135, .T. ) ;
#113133 = CIRCLE ( 'NONE', #254, 0.1000000000000002554 ) ;
#113134 = CIRCLE ( 'NONE', #63059, 0.1000000000000002554 ) ;
#113135 = CARTESIAN_POINT ( 'NONE',  ( -9.400000000000009237, 2.500000000000000000, -4.676537180435974328 ) ) ;
#113136 = ORIENTED_EDGE ( 'NONE', *, *, #85416, .T. ) ;
#113137 = FACE_OUTER_BOUND ( 'NONE', #36157, .T. ) ;
#113138 = CARTESIAN_POINT ( 'NONE',  ( 10.87377556668746514, -2.500000000000257128, -8.986829607522045293 ) ) ;
#113139 = CARTESIAN_POINT ( 'NONE',  ( 1.649999999999951950, 2.500000000000000000, -5.902370205355750521 ) ) ;
#113140 = DIRECTION ( 'NONE',  ( 0.000000000000000000, -0.000000000000000000, 1.000000000000000000 ) ) ;
#113141 = EDGE_CURVE ( 'NONE', #59160, #87633, #65653, .T. ) ;
#113142 = EDGE_CURVE ( 'NONE', #34124, #86025, #102311, .T. ) ;
#113143 = ORIENTED_EDGE ( 'NONE', *, *, #60029, .T. ) ;
#113144 = ADVANCED_FACE ( 'NONE', ( #114112 ), #108642, .T. ) ;
#113145 = ORIENTED_EDGE ( 'NONE', *, *, #26127, .T. ) ;
#113146 = VERTEX_POINT ( 'NONE', #24446 ) ;
#113147 = CARTESIAN_POINT ( 'NONE',  ( -0.2000000000000347888, 2.500000000000000000, 0.2464101615137758439 ) ) ;
#113148 = LINE ( 'NONE', #51671, #20553 ) ;
#113149 = DIRECTION ( 'NONE',  ( -4.274815082592931898E-19, -0.9999939076577903929, -0.003490651415223739937 ) ) ;
#113150 = FACE_BOUND ( 'NONE', #62567, .T. ) ;
#113151 = DIRECTION ( 'NONE',  ( -0.000000000000000000, -1.000000000000000000, -0.000000000000000000 ) ) ;
#113152 = CARTESIAN_POINT ( 'NONE',  ( -9.600000000000008527, 2.500000000000000000, -4.330127018922197202 ) ) ;
#113153 = EDGE_CURVE ( 'NONE', #56350, #47664, #39633, .T. ) ;
#113154 = DIRECTION ( 'NONE',  ( 0.000000000000000000, -0.9999939076577903929, 0.003490651415223739937 ) ) ;
#113155 = CIRCLE ( 'NONE', #8584, 0.1000000000000002554 ) ;
#113156 = VECTOR ( 'NONE', #9908, 1000.000000000000000 ) ;
#113158 = CIRCLE ( 'NONE', #96417, 0.06509327318403745899 ) ;
#113157 = DIRECTION ( 'NONE',  ( -0.000000000000000000, -1.000000000000000000, -0.000000000000000000 ) ) ;
#113159 = CARTESIAN_POINT ( 'NONE',  ( 139.9358549477330200, 2.500000000000000000, -3.576063159858998475 ) ) ;
#113160 = CARTESIAN_POINT ( 'NONE',  ( -2.100000000000033396, 2.500000000000000000, 0.7928203230275495672 ) ) ;
#113161 = ORIENTED_EDGE ( 'NONE', *, *, #37642, .F. ) ;
#113162 = AXIS2_PLACEMENT_3D ( 'NONE', #117135, #117780, #47141 ) ;
#113163 = DIRECTION ( 'NONE',  ( 0.000000000000000000, 0.000000000000000000, 1.000000000000000000 ) ) ;
#113164 = CIRCLE ( 'NONE', #92227, 0.1000000000000002554 ) ;
#113165 = VERTEX_POINT ( 'NONE', #46030 ) ;
#113166 = ORIENTED_EDGE ( 'NONE', *, *, #16615, .T. ) ;
#113167 = PLANE ( 'NONE',  #115532 ) ;
#113168 = EDGE_CURVE ( 'NONE', #22620, #89608, #36211, .T. ) ;
#113169 = FACE_BOUND ( 'NONE', #59394, .T. ) ;
#113170 = CARTESIAN_POINT ( 'NONE',  ( 6.249999999999967137, 2.500000000000000000, -2.065063509461102065 ) ) ;
#113171 = ORIENTED_EDGE ( 'NONE', *, *, #95137, .F. ) ;
#113172 = CARTESIAN_POINT ( 'NONE',  ( 43.31214921617725366, 3.511364963952507967, 3.941696051818830870 ) ) ;
#113173 = DIRECTION ( 'NONE',  ( -0.000000000000000000, 1.000000000000000000, -0.000000000000000000 ) ) ;
#113174 = ORIENTED_EDGE ( 'NONE', *, *, #38009, .F. ) ;
#113175 = DIRECTION ( 'NONE',  ( -4.274815082592931898E-19, -0.9999939076577903929, -0.003490651415223739937 ) ) ;
#113176 = FACE_OUTER_BOUND ( 'NONE', #70953, .T. ) ;
#113177 = EDGE_CURVE ( 'NONE', #109519, #125908, #116947, .T. ) ;
#113178 = EDGE_LOOP ( 'NONE', ( #100462, #36932 ) ) ;
#113179 = CARTESIAN_POINT ( 'NONE',  ( -6.650000000000019007, 2.500000000000000000, -5.702370205355749455 ) ) ;
#113180 = FACE_OUTER_BOUND ( 'NONE', #41118, .T. ) ;
#113181 = CIRCLE ( 'NONE', #106924, 0.06509327318403745899 ) ;
#113182 = VERTEX_POINT ( 'NONE', #87217 ) ;
#113183 = DIRECTION ( 'NONE',  ( -0.000000000000000000, 1.000000000000000000, -0.000000000000000000 ) ) ;
#113184 = CARTESIAN_POINT ( 'NONE',  ( 2.499999999999945377, 2.500000000000000000, 5.022947341949748790 ) ) ;
#113185 = DIRECTION ( 'NONE',  ( 0.000000000000000000, 0.000000000000000000, -1.000000000000000000 ) ) ;
#113186 = EDGE_LOOP ( 'NONE', ( #81879, #123366 ) ) ;
#113187 = ORIENTED_EDGE ( 'NONE', *, *, #3434, .F. ) ;
#113188 = EDGE_CURVE ( 'NONE', #107957, #36304, #57119, .T. ) ;
#113189 = DIRECTION ( 'NONE',  ( 1.000000000000000000, -0.000000000000000000, -0.000000000000000000 ) ) ;
#113190 = CIRCLE ( 'NONE', #8723, 0.1000000000000000472 ) ;
#113191 = ORIENTED_EDGE ( 'NONE', *, *, #7248, .F. ) ;
#113192 = CARTESIAN_POINT ( 'NONE',  ( -3.750000000000027534, 12.50000000000000000, 2.857883832488649301 ) ) ;
#113193 = CIRCLE ( 'NONE', #104774, 0.09999999999999982514 ) ;
#113194 = CARTESIAN_POINT ( 'NONE',  ( 4.799999999999935874, 2.500000000000000000, 3.883716857408421319 ) ) ;
#113195 = EDGE_LOOP ( 'NONE', ( #87166, #53261, #14025, #111002 ) ) ;
#113196 = AXIS2_PLACEMENT_3D ( 'NONE', #57419, #56110, #128091 ) ;
#113197 = DIRECTION ( 'NONE',  ( -4.274815082592931898E-19, -0.9999939076577903929, -0.003490651415223739937 ) ) ;
#113198 = CARTESIAN_POINT ( 'NONE',  ( 9.999999999999948486, 12.50000000000000000, -4.395220292106239768 ) ) ;
#113199 = FACE_OUTER_BOUND ( 'NONE', #68931, .T. ) ;
#113200 = DIRECTION ( 'NONE',  ( -0.000000000000000000, 1.000000000000000000, -0.000000000000000000 ) ) ;
#113201 = CARTESIAN_POINT ( 'NONE',  ( 11.64999999999990443, 2.500000000000000000, -5.802370205355749988 ) ) ;
#113202 = CIRCLE ( 'NONE', #23319, 0.06509327318403741736 ) ;
#113203 = VERTEX_POINT ( 'NONE', #47961 ) ;
#113204 = PRODUCT_DEFINITION_FORMATION_WITH_SPECIFIED_SOURCE ( 'ANY', '', #33622, .NOT_KNOWN. ) ;
#113205 = VECTOR ( 'NONE', #24463, 1000.000000000000000 ) ;
#113206 = ORIENTED_EDGE ( 'NONE', *, *, #72882, .F. ) ;
#113207 = CARTESIAN_POINT ( 'NONE',  ( 5.849999999999932143, 2.500000000000000000, 2.265063509461097357 ) ) ;
#113208 = CARTESIAN_POINT ( 'NONE',  ( 103.2667551388651930, 7.528838585660450278, -1.644710558206996964 ) ) ;
#113209 = CIRCLE ( 'NONE', #54626, 0.1000000000000002554 ) ;
#113211 = VERTEX_POINT ( 'NONE', #18484 ) ;
#113210 = VERTEX_POINT ( 'NONE', #118618 ) ;
#113212 = ORIENTED_EDGE ( 'NONE', *, *, #55940, .F. ) ;
#113213 = DIRECTION ( 'NONE',  ( -0.000000000000000000, 1.000000000000000000, -0.000000000000000000 ) ) ;
#113214 = CONICAL_SURFACE ( 'NONE', #125720, 0.09999999999999999167, 0.003490658503988666988 ) ;
#113215 = CARTESIAN_POINT ( 'NONE',  ( 8.099999999999923261, 12.50000000000000000, -3.983716857408426293 ) ) ;
#113216 = DIRECTION ( 'NONE',  ( 0.000000000000000000, 0.000000000000000000, -1.000000000000000000 ) ) ;
#113217 = EDGE_CURVE ( 'NONE', #30225, #99143, #127441, .T. ) ;
#113218 = DIRECTION ( 'NONE',  ( 1.000000000000000000, 0.000000000000000000, 0.000000000000000000 ) ) ;
#113219 = CARTESIAN_POINT ( 'NONE',  ( -11.25000000000000178, 2.500000000000000000, -5.902370205355746968 ) ) ;
#113220 = CIRCLE ( 'NONE', #123591, 0.06509327318403745899 ) ;
#113221 = CIRCLE ( 'NONE', #52589, 0.06509327318403745899 ) ;
#113222 = DIRECTION ( 'NONE',  ( 0.000000000000000000, 1.000000000000000000, 0.000000000000000000 ) ) ;
#113223 = CARTESIAN_POINT ( 'NONE',  ( 14.79999999999989235, 12.50000000000000000, 0.3464101615137735735 ) ) ;
#113224 = CARTESIAN_POINT ( 'NONE',  ( -4.400000000000025224, 12.50000000000000000, 3.983716857408420076 ) ) ;
#113225 = CARTESIAN_POINT ( 'NONE',  ( -0.8500000000000382805, 2.500000000000000000, -7.088010851410853519 ) ) ;
#113226 = CARTESIAN_POINT ( 'NONE',  ( 6.649999999999930189, 12.50000000000000000, -1.472243186433550122 ) ) ;
#113227 = EDGE_CURVE ( 'NONE', #115931, #109687, #93979, .T. ) ;
#113228 = ORIENTED_EDGE ( 'NONE', *, *, #115816, .T. ) ;
#113229 = LINE ( 'NONE', #22940, #42309 ) ;
#113230 = ADVANCED_FACE ( 'NONE', ( #27641 ), #126518, .T. ) ;
#113231 = VERTEX_POINT ( 'NONE', #69510 ) ;
#113232 = EDGE_CURVE ( 'NONE', #69676, #20627, #12401, .T. ) ;
#113233 = ORIENTED_EDGE ( 'NONE', *, *, #60773, .F. ) ;
#113234 = ADVANCED_FACE ( 'NONE', ( #79357 ), #119257, .T. ) ;
#113235 = CARTESIAN_POINT ( 'NONE',  ( 3.549999999999940314, 2.500000000000000000, 6.841600689897072485 ) ) ;
#113237 = ADVANCED_FACE ( 'NONE', ( #66925 ), #119026, .T. ) ;
#113236 = DIRECTION ( 'NONE',  ( 0.000000000000000000, -0.000000000000000000, 1.000000000000000000 ) ) ;
#113238 = DIRECTION ( 'NONE',  ( 0.000000000000000000, 0.000000000000000000, -1.000000000000000000 ) ) ;
#113239 = CARTESIAN_POINT ( 'NONE',  ( 9.399999999999915090, 12.50000000000000000, 4.676537180435972552 ) ) ;
#113240 = CARTESIAN_POINT ( 'NONE',  ( -12.09999999999999609, 2.500000000000000000, -3.637306695894647390 ) ) ;
#113241 = EDGE_CURVE ( 'NONE', #81692, #119348, #7367, .T. ) ;
#113242 = CARTESIAN_POINT ( 'NONE',  ( 16.56576425165006583, -1.500000000000000666, 6.084390597445813675 ) ) ;
#113243 = EDGE_CURVE ( 'NONE', #127958, #6155, #123238, .T. ) ;
#113244 = AXIS2_PLACEMENT_3D ( 'NONE', #119117, #30759, #100744 ) ;
#113245 = CARTESIAN_POINT ( 'NONE',  ( -11.05000000000000071, 12.50000000000000000, 6.841600689897072485 ) ) ;
#113246 = EDGE_LOOP ( 'NONE', ( #99786, #47279, #39683, #42085 ) ) ;
#113247 = CARTESIAN_POINT ( 'NONE',  ( 112.3254613740535177, 8.329167917205943183, 2.528930095568325598 ) ) ;
#113248 = CIRCLE ( 'NONE', #65117, 0.1000000000000002554 ) ;
#113249 = CIRCLE ( 'NONE', #19138, 0.06509327318403745899 ) ;
#113250 = ADVANCED_FACE ( 'NONE', ( #109447 ), #17839, .T. ) ;
#113252 = ADVANCED_FACE ( 'NONE', ( #116682 ), #79334, .T. ) ;
#113251 = CARTESIAN_POINT ( 'NONE',  ( -3.750000000000029310, 12.50000000000000000, -7.253104124594891289 ) ) ;
#113253 = ORIENTED_EDGE ( 'NONE', *, *, #50072, .T. ) ;
#113255 = ADVANCED_FACE ( 'NONE', ( #117969 ), #6138, .T. ) ;
#113254 = CIRCLE ( 'NONE', #40104, 0.06509327318403745899 ) ;
#113256 = ORIENTED_EDGE ( 'NONE', *, *, #112271, .T. ) ;
#113257 = VECTOR ( 'NONE', #39679, 1000.000000000000000 ) ;
#113258 = ORIENTED_EDGE ( 'NONE', *, *, #95510, .T. ) ;
#113259 = CIRCLE ( 'NONE', #61027, 0.06509327318403745899 ) ;
#113260 = AXIS2_PLACEMENT_3D ( 'NONE', #54521, #83363, #84642 ) ;
#113261 = ORIENTED_EDGE ( 'NONE', *, *, #93326, .T. ) ;
#113262 = EDGE_CURVE ( 'NONE', #109667, #65076, #68226, .T. ) ;
#113263 = DIRECTION ( 'NONE',  ( -0.000000000000000000, -1.000000000000000000, -0.000000000000000000 ) ) ;
#113264 = DIRECTION ( 'NONE',  ( 0.000000000000000000, 1.000000000000000000, 0.000000000000000000 ) ) ;
#113265 = AXIS2_PLACEMENT_3D ( 'NONE', #75656, #103849, #124774 ) ;
#113266 = DIRECTION ( 'NONE',  ( 0.000000000000000000, 1.000000000000000000, 0.000000000000000000 ) ) ;
#113267 = FACE_OUTER_BOUND ( 'NONE', #48915, .T. ) ;
#113268 = CARTESIAN_POINT ( 'NONE',  ( 13.29999999999990301, 2.500000000000000000, -4.330127018922201643 ) ) ;
#113269 = ORIENTED_EDGE ( 'NONE', *, *, #23704, .T. ) ;
#113270 = FACE_OUTER_BOUND ( 'NONE', #115049, .T. ) ;
#113271 = CARTESIAN_POINT ( 'NONE',  ( -9.600000000000008527, 2.500000000000000000, -3.737306695894645259 ) ) ;
#113272 = CARTESIAN_POINT ( 'NONE',  ( -9.200000000000006395, 12.50000000000000000, 4.330127018922196314 ) ) ;
#113273 = CARTESIAN_POINT ( 'NONE',  ( 87.50000000000001421, 0.000000000000000000, 0.000000000000000000 ) ) ;
#113274 = ORIENTED_EDGE ( 'NONE', *, *, #93469, .F. ) ;
#113275 = ORIENTED_EDGE ( 'NONE', *, *, #124814, .T. ) ;
#113276 = VERTEX_POINT ( 'NONE', #6698 ) ;
#113277 = CARTESIAN_POINT ( 'NONE',  ( -15.19999999999998153, 12.50000000000000000, -0.4115034346978133639 ) ) ;
#113278 = FACE_OUTER_BOUND ( 'NONE', #101365, .T. ) ;
#113279 = AXIS2_PLACEMENT_3D ( 'NONE', #70458, #31823, #71753 ) ;
#113280 = CARTESIAN_POINT ( 'NONE',  ( 1.322875655532295136, -1.500000000000000222, -5.000000000000004441 ) ) ;
#113281 = AXIS2_PLACEMENT_3D ( 'NONE', #34233, #31640, #74143 ) ;
#113282 = ORIENTED_EDGE ( 'NONE', *, *, #54052, .T. ) ;
#113283 = DIRECTION ( 'NONE',  ( 0.000000000000000000, 0.000000000000000000, -1.000000000000000000 ) ) ;
#113284 = CARTESIAN_POINT ( 'NONE',  ( -6.450000000000014388, 2.500000000000000000, 1.818653347947321475 ) ) ;
#113285 = CARTESIAN_POINT ( 'NONE',  ( 145.7653593504141725, 0.5000000000000000000, -1.098523788719517169 ) ) ;
#113286 = CARTESIAN_POINT ( 'NONE',  ( -0.6500000000000389910, 12.50000000000000000, -6.148780366869526226 ) ) ;
#113287 = AXIS2_PLACEMENT_3D ( 'NONE', #112985, #120237, #51503 ) ;
#113288 = AXIS2_PLACEMENT_3D ( 'NONE', #82168, #102454, #12122 ) ;
#113289 = EDGE_CURVE ( 'NONE', #118526, #18296, #22892, .T. ) ;
#113290 = CIRCLE ( 'NONE', #17115, 0.1000000000000002554 ) ;
#113291 = DIRECTION ( 'NONE',  ( 0.000000000000000000, 0.000000000000000000, 1.000000000000000000 ) ) ;
#113292 = VECTOR ( 'NONE', #42285, 1000.000000000000000 ) ;
#113293 = EDGE_CURVE ( 'NONE', #45906, #7993, #112775, .T. ) ;
#113294 = VERTEX_POINT ( 'NONE', #121 ) ;
#113295 = EDGE_LOOP ( 'NONE', ( #74642, #15621, #100991, #8887 ) ) ;
#113296 = CARTESIAN_POINT ( 'NONE',  ( 2.099999999999949463, 2.500000000000000000, -3.637306695894650055 ) ) ;
#113297 = DIRECTION ( 'NONE',  ( 0.000000000000000000, 1.000000000000000000, 0.000000000000000000 ) ) ;
#113298 = CARTESIAN_POINT ( 'NONE',  ( -5.450000000000023270, 2.500000000000000000, -2.065063509461102065 ) ) ;
#113300 = AXIS2_PLACEMENT_3D ( 'NONE', #27813, #89321, #39606 ) ;
#113299 = DIRECTION ( 'NONE',  ( -0.000000000000000000, 1.000000000000000000, -0.000000000000000000 ) ) ;
#113301 = EDGE_CURVE ( 'NONE', #68377, #14536, #50517, .T. ) ;
#113303 = CARTESIAN_POINT ( 'NONE',  ( 1.049999999999954969, 2.500000000000000000, -6.841600689897077814 ) ) ;
#113302 = VECTOR ( 'NONE', #119275, 1000.000000000000000 ) ;
#113304 = EDGE_LOOP ( 'NONE', ( #94816, #18419, #12083, #60200 ) ) ;
#113305 = CIRCLE ( 'NONE', #94525, 0.09999999999999982514 ) ;
#113306 = AXIS2_PLACEMENT_3D ( 'NONE', #27577, #46583, #86505 ) ;
#113307 = AXIS2_PLACEMENT_3D ( 'NONE', #38708, #118517, #69412 ) ;
#113308 = ORIENTED_EDGE ( 'NONE', *, *, #90962, .T. ) ;
#113309 = DIRECTION ( 'NONE',  ( -0.000000000000000000, 1.000000000000000000, -0.000000000000000000 ) ) ;
#113310 = DIRECTION ( 'NONE',  ( 0.000000000000000000, 1.000000000000000000, 0.000000000000000000 ) ) ;
#113311 = DIRECTION ( 'NONE',  ( -0.000000000000000000, -1.000000000000000000, -0.000000000000000000 ) ) ;
#113312 = AXIS2_PLACEMENT_3D ( 'NONE', #118473, #58286, #98192 ) ;
#113313 = DIRECTION ( 'NONE',  ( 0.000000000000000000, 1.000000000000000000, 0.000000000000000000 ) ) ;
#113314 = FACE_OUTER_BOUND ( 'NONE', #21831, .T. ) ;
#113315 = ORIENTED_EDGE ( 'NONE', *, *, #30506, .T. ) ;
#113316 = LINE ( 'NONE', #23012, #51097 ) ;
#113317 = DIRECTION ( 'NONE',  ( 0.000000000000000000, -0.9999939076577903929, 0.003490651415223739937 ) ) ;
#113318 = AXIS2_PLACEMENT_3D ( 'NONE', #36077, #14474, #116557 ) ;
#113319 = ORIENTED_EDGE ( 'NONE', *, *, #61840, .F. ) ;
#113320 = DIRECTION ( 'NONE',  ( 0.000000000000000000, 1.000000000000000000, 0.000000000000000000 ) ) ;
#113321 = ORIENTED_EDGE ( 'NONE', *, *, #97279, .T. ) ;
#113322 = DIRECTION ( 'NONE',  ( 0.000000000000000000, -0.9999939076577903929, 0.003490651415223739937 ) ) ;
#113323 = EDGE_LOOP ( 'NONE', ( #116059, #49874, #24295, #111383 ) ) ;
#113324 = DIRECTION ( 'NONE',  ( 0.000000000000000000, -0.000000000000000000, 1.000000000000000000 ) ) ;
#113325 = CARTESIAN_POINT ( 'NONE',  ( 149.5981739382431783, 2.500000000000000000, -1.703575533167231537 ) ) ;
#113326 = ORIENTED_EDGE ( 'NONE', *, *, #12320, .T. ) ;
#113327 = ORIENTED_EDGE ( 'NONE', *, *, #90165, .F. ) ;
#113328 = CARTESIAN_POINT ( 'NONE',  ( 184.5468750003414300, -8.734944146203032389, -1.604583208406768146E-15 ) ) ;
#113329 = DIRECTION ( 'NONE',  ( 0.000000000000000000, 0.000000000000000000, 1.000000000000000000 ) ) ;
#113330 = CARTESIAN_POINT ( 'NONE',  ( 0.7999999999999553024, 12.50000000000000000, -4.330127018922201643 ) ) ;
#113331 = CARTESIAN_POINT ( 'NONE',  ( 185.3593750003413732, 0.000000000000000000, 7.564683531250000925 ) ) ;
#113332 = CIRCLE ( 'NONE', #67337, 0.06509327318403745899 ) ;
#113333 = LINE ( 'NONE', #102242, #11705 ) ;
#113334 = CARTESIAN_POINT ( 'NONE',  ( 0.4499999999999573785, 2.500000000000000000, -6.395190528383301931 ) ) ;
#113335 = AXIS2_PLACEMENT_3D ( 'NONE', #128411, #66230, #48538 ) ;
#113336 = FACE_OUTER_BOUND ( 'NONE', #28801, .T. ) ;
#113337 = DIRECTION ( 'NONE',  ( 0.000000000000000000, 0.000000000000000000, -1.000000000000000000 ) ) ;
#113339 = ORIENTED_EDGE ( 'NONE', *, *, #69944, .F. ) ;
#113338 = AXIS2_PLACEMENT_3D ( 'NONE', #123097, #22330, #84458 ) ;
#113341 = ORIENTED_EDGE ( 'NONE', *, *, #29259, .T. ) ;
#113340 = AXIS2_PLACEMENT_3D ( 'NONE', #108069, #129035, #79275 ) ;
#113342 = LINE ( 'NONE', #120593, #65338 ) ;
#113343 = ORIENTED_EDGE ( 'NONE', *, *, #98150, .F. ) ;
#113344 = DIRECTION ( 'NONE',  ( 0.000000000000000000, 1.000000000000000000, 0.000000000000000000 ) ) ;
#113345 = DIRECTION ( 'NONE',  ( 0.000000000000000000, 0.000000000000000000, 1.000000000000000000 ) ) ;
#113346 = EDGE_CURVE ( 'NONE', #61065, #42141, #52451, .T. ) ;
#113347 = DIRECTION ( 'NONE',  ( 0.000000000000000000, 0.000000000000000000, 1.000000000000000000 ) ) ;
#113350 = ORIENTED_EDGE ( 'NONE', *, *, #34425, .T. ) ;
#113349 = ORIENTED_EDGE ( 'NONE', *, *, #83826, .F. ) ;
#113348 = CIRCLE ( 'NONE', #125961, 0.06509327318403745899 ) ;
#113351 = FACE_BOUND ( 'NONE', #112992, .T. ) ;
#113352 = VERTEX_POINT ( 'NONE', #23006 ) ;
#113353 = EDGE_CURVE ( 'NONE', #123245, #22096, #122497, .T. ) ;
#113354 = CARTESIAN_POINT ( 'NONE',  ( 10.44999999999991402, 2.500000000000000000, 6.595190528383296780 ) ) ;
#113355 = DIRECTION ( 'NONE',  ( 0.000000000000000000, 1.000000000000000000, 0.000000000000000000 ) ) ;
#113356 = AXIS2_PLACEMENT_3D ( 'NONE', #4397, #76403, #36496 ) ;
#113357 = CARTESIAN_POINT ( 'NONE',  ( -9.150000000000005684, 2.500000000000000000, 6.495190528383297135 ) ) ;
#113358 = CARTESIAN_POINT ( 'NONE',  ( 1.249999999999952038, 2.500000000000000000, 5.702370205355745014 ) ) ;
#113359 = DIRECTION ( 'NONE',  ( 0.000000000000000000, -0.000000000000000000, 1.000000000000000000 ) ) ;
#113360 = DIRECTION ( 'NONE',  ( 0.000000000000000000, 0.000000000000000000, 1.000000000000000000 ) ) ;
#113361 = DIRECTION ( 'NONE',  ( 0.000000000000000000, 0.000000000000000000, -1.000000000000000000 ) ) ;
#113362 = CARTESIAN_POINT ( 'NONE',  ( 4.599999999999940137, 2.500000000000000000, -5.122947341949753763 ) ) ;
#113363 = ADVANCED_FACE ( 'NONE', ( #92374 ), #29249, .T. ) ;
#113364 = CARTESIAN_POINT ( 'NONE',  ( 186.1510416670080588, 4.367472073101518859, -7.564683531249999149 ) ) ;
#113365 = CARTESIAN_POINT ( 'NONE',  ( -5.600000000000023626, 2.500000000000000000, -3.983716857408426293 ) ) ;
#113366 = CARTESIAN_POINT ( 'NONE',  ( -7.950000000000012612, 2.500000000000000000, -2.165063509461101710 ) ) ;
#113367 = ORIENTED_EDGE ( 'NONE', *, *, #85172, .T. ) ;
#113368 = VERTEX_POINT ( 'NONE', #110723 ) ;
#113369 = EDGE_LOOP ( 'NONE', ( #87677, #66599, #56013, #50435 ) ) ;
#113370 = CARTESIAN_POINT ( 'NONE',  ( 3.149999999999942624, 2.500000000000000000, 6.148780366869520897 ) ) ;
#113371 = ORIENTED_EDGE ( 'NONE', *, *, #60858, .F. ) ;
#113372 = DIRECTION ( 'NONE',  ( 0.000000000000000000, 0.000000000000000000, 1.000000000000000000 ) ) ;
#113374 = ORIENTED_EDGE ( 'NONE', *, *, #104637, .F. ) ;
#113373 = ORIENTED_EDGE ( 'NONE', *, *, #17549, .F. ) ;
#113375 = ORIENTED_EDGE ( 'NONE', *, *, #59596, .F. ) ;
#113376 = DIRECTION ( 'NONE',  ( 0.000000000000000000, 0.000000000000000000, 1.000000000000000000 ) ) ;
#113377 = VECTOR ( 'NONE', #21866, 1000.000000000000000 ) ;
#113378 = PLANE ( 'NONE',  #9168 ) ;
#113379 = ADVANCED_FACE ( 'NONE', ( #89802 ), #96118, .T. ) ;
#113380 = CARTESIAN_POINT ( 'NONE',  ( 186.9166666666666856, 6.668395609140176816, 3.850000000000000977 ) ) ;
#113381 = CARTESIAN_POINT ( 'NONE',  ( -4.400000000000025224, 2.500000000000000000, 0.3464101615137735735 ) ) ;
#113382 = CARTESIAN_POINT ( 'NONE',  ( -7.700000000000012612, 2.500000000000000000, 4.776537180435972196 ) ) ;
#113383 = ORIENTED_EDGE ( 'NONE', *, *, #123684, .T. ) ;
#113384 = AXIS2_PLACEMENT_3D ( 'NONE', #65808, #4950, #125389 ) ;
#113385 = CIRCLE ( 'NONE', #6746, 0.06509327318403741736 ) ;
#113386 = CARTESIAN_POINT ( 'NONE',  ( 9.349999999999916156, 12.50000000000000000, 6.776507416713035248 ) ) ;
#113387 = ORIENTED_EDGE ( 'NONE', *, *, #172, .F. ) ;
#113389 = EDGE_CURVE ( 'NONE', #4798, #85752, #1417, .T. ) ;
#113388 = CONICAL_SURFACE ( 'NONE', #125896, 0.1000000000000002554, 0.003490658503988666988 ) ;
#113390 = ORIENTED_EDGE ( 'NONE', *, *, #123893, .T. ) ;
#113391 = VECTOR ( 'NONE', #112162, 1000.000000000000000 ) ;
#113392 = ORIENTED_EDGE ( 'NONE', *, *, #100581, .T. ) ;
#113393 = CARTESIAN_POINT ( 'NONE',  ( -15.59999999999998010, 12.50000000000000000, 0.3464101615137759604 ) ) ;
#113394 = EDGE_CURVE ( 'NONE', #110762, #16380, #10444, .T. ) ;
#113395 = VERTEX_POINT ( 'NONE', #12523 ) ;
#113396 = EDGE_CURVE ( 'NONE', #50485, #96613, #54358, .T. ) ;
#113397 = ORIENTED_EDGE ( 'NONE', *, *, #125677, .F. ) ;
#113398 = EDGE_CURVE ( 'NONE', #28288, #62105, #119912, .T. ) ;
#113399 = ORIENTED_EDGE ( 'NONE', *, *, #77240, .F. ) ;
#113400 = ADVANCED_FACE ( 'NONE', ( #60373 ), #125461, .T. ) ;
#113401 = DIRECTION ( 'NONE',  ( 0.000000000000000000, 1.000000000000000000, 0.000000000000000000 ) ) ;
#113402 = CIRCLE ( 'NONE', #29877, 0.1000000000000002554 ) ;
#113403 = CARTESIAN_POINT ( 'NONE',  ( 183.8906250003414016, 0.000000000000000000, 7.700000000000000178 ) ) ;
#113404 = DIRECTION ( 'NONE',  ( -4.274815082592931898E-19, -0.9999939076577903929, -0.003490651415223739937 ) ) ;
#113405 = DIRECTION ( 'NONE',  ( 0.000000000000000000, 0.000000000000000000, -1.000000000000000000 ) ) ;
#113406 = VECTOR ( 'NONE', #3920, 1000.000000000000000 ) ;
#113407 = DIRECTION ( 'NONE',  ( 0.000000000000000000, 0.000000000000000000, 1.000000000000000000 ) ) ;
#113408 = VECTOR ( 'NONE', #42593, 1000.000000000000000 ) ;
#113409 = AXIS2_PLACEMENT_3D ( 'NONE', #95507, #94216, #104664 ) ;
#113410 = ADVANCED_FACE ( 'NONE', ( #22376 ), #21055, .T. ) ;
#113411 = DIRECTION ( 'NONE',  ( 0.000000000000000000, 1.000000000000000000, 0.000000000000000000 ) ) ;
#113412 = EDGE_CURVE ( 'NONE', #128788, #78315, #10579, .T. ) ;
#113413 = AXIS2_PLACEMENT_3D ( 'NONE', #45094, #117014, #105291 ) ;
#113414 = FACE_OUTER_BOUND ( 'NONE', #71511, .T. ) ;
#113415 = ORIENTED_EDGE ( 'NONE', *, *, #35112, .T. ) ;
#113416 = LINE ( 'NONE', #23759, #123731 ) ;
#113417 = ADVANCED_FACE ( 'NONE', ( #772 ), #117028, .T. ) ;
#113418 = ORIENTED_EDGE ( 'NONE', *, *, #100636, .F. ) ;
#113419 = AXIS2_PLACEMENT_3D ( 'NONE', #23514, #113844, #114473 ) ;
#113420 = DIRECTION ( 'NONE',  ( 0.000000000000000000, -0.000000000000000000, 1.000000000000000000 ) ) ;
#113421 = EDGE_LOOP ( 'NONE', ( #82066, #101240 ) ) ;
#113422 = EDGE_CURVE ( 'NONE', #45696, #21874, #112859, .T. ) ;
#113423 = VERTEX_POINT ( 'NONE', #91096 ) ;
#113424 = EDGE_CURVE ( 'NONE', #69423, #49637, #92018, .T. ) ;
#113425 = DIRECTION ( 'NONE',  ( -0.000000000000000000, -1.000000000000000000, -0.000000000000000000 ) ) ;
#113426 = DIRECTION ( 'NONE',  ( 0.000000000000000000, 1.000000000000000000, 0.000000000000000000 ) ) ;
#113427 = DIRECTION ( 'NONE',  ( -0.000000000000000000, -1.000000000000000000, -0.000000000000000000 ) ) ;
#113428 = EDGE_LOOP ( 'NONE', ( #29897, #48408 ) ) ;
#113429 = ORIENTED_EDGE ( 'NONE', *, *, #71310, .F. ) ;
#113430 = DIRECTION ( 'NONE',  ( 0.000000000000000000, 0.000000000000000000, -1.000000000000000000 ) ) ;
#113431 = CARTESIAN_POINT ( 'NONE',  ( 1.049999999999953637, 2.500000000000000000, -1.718653347947326049 ) ) ;
#113432 = CIRCLE ( 'NONE', #119679, 0.09999999999999982514 ) ;
#113433 = PLANE ( 'NONE',  #2070 ) ;
#113434 = DIRECTION ( 'NONE',  ( 0.000000000000000000, 0.000000000000000000, 1.000000000000000000 ) ) ;
#113435 = CARTESIAN_POINT ( 'NONE',  ( 0.6499999999999561684, 2.500000000000000000, -1.718653347947325827 ) ) ;
#113436 = EDGE_LOOP ( 'NONE', ( #102183, #129031 ) ) ;
#113437 = CONICAL_SURFACE ( 'NONE', #21498, 0.1000000000000002554, 0.003490658503988666988 ) ;
#113438 = VECTOR ( 'NONE', #32476, 1000.000000000000000 ) ;
#113439 = EDGE_LOOP ( 'NONE', ( #9511, #109206, #55651, #98121 ) ) ;
#113440 = FACE_OUTER_BOUND ( 'NONE', #80980, .T. ) ;
#113441 = DIRECTION ( 'NONE',  ( 0.000000000000000000, 1.000000000000000000, 0.000000000000000000 ) ) ;
#113442 = AXIS2_PLACEMENT_3D ( 'NONE', #121769, #92312, #70749 ) ;
#113443 = AXIS2_PLACEMENT_3D ( 'NONE', #16017, #65115, #116156 ) ;
#113444 = CONICAL_SURFACE ( 'NONE', #29832, 0.09999999999999982514, 0.003490658503988666988 ) ;
#113445 = AXIS2_PLACEMENT_3D ( 'NONE', #99717, #55430, #40147 ) ;
#113446 = CARTESIAN_POINT ( 'NONE',  ( 185.4635416670080872, -4.367472073101519747, 7.564683531249999149 ) ) ;
#113447 = DIRECTION ( 'NONE',  ( -0.000000000000000000, 1.000000000000000000, -0.000000000000000000 ) ) ;
#113448 = DIRECTION ( 'NONE',  ( -0.000000000000000000, 1.000000000000000000, -0.000000000000000000 ) ) ;
#113449 = DIRECTION ( 'NONE',  ( -0.000000000000000000, -1.000000000000000000, -0.000000000000000000 ) ) ;
#113450 = CARTESIAN_POINT ( 'NONE',  ( 5.399999999999934630, 12.50000000000000000, -0.6928203230275542523 ) ) ;
#113451 = ORIENTED_EDGE ( 'NONE', *, *, #2067, .T. ) ;
#113452 = AXIS2_PLACEMENT_3D ( 'NONE', #52732, #53391, #122135 ) ;
#113454 = ADVANCED_FACE ( 'NONE', ( #121193 ), #6217, .T. ) ;
#113453 = DIRECTION ( 'NONE',  ( 0.000000000000000000, 1.000000000000000000, 0.000000000000000000 ) ) ;
#113455 = CARTESIAN_POINT ( 'NONE',  ( -13.34999999999999076, 2.500000000000000000, 1.472243186433549456 ) ) ;
#113456 = DIRECTION ( 'NONE',  ( 0.000000000000000000, 0.000000000000000000, 1.000000000000000000 ) ) ;
#113457 = ADVANCED_FACE ( 'NONE', ( #61649 ), #22978, .T. ) ;
#113458 = ORIENTED_EDGE ( 'NONE', *, *, #2884, .F. ) ;
#113459 = CARTESIAN_POINT ( 'NONE',  ( 6.849999999999929479, 12.50000000000000000, 6.148780366869520009 ) ) ;
#113460 = CIRCLE ( 'NONE', #75799, 0.06509327318403741736 ) ;
#113461 = ORIENTED_EDGE ( 'NONE', *, *, #95925, .T. ) ;
#113462 = CARTESIAN_POINT ( 'NONE',  ( -8.150000000000012790, 2.500000000000000000, 2.411473670974873862 ) ) ;
#113463 = ORIENTED_EDGE ( 'NONE', *, *, #12466, .T. ) ;
#113464 = DIRECTION ( 'NONE',  ( -4.274815082592931898E-19, -0.9999939076577903929, -0.003490651415223739937 ) ) ;
#113465 = DIRECTION ( 'NONE',  ( 0.000000000000000000, 0.000000000000000000, 1.000000000000000000 ) ) ;
#113466 = FACE_OUTER_BOUND ( 'NONE', #66729, .T. ) ;
#113467 = AXIS2_PLACEMENT_3D ( 'NONE', #123273, #4121, #93183 ) ;
#113468 = ORIENTED_EDGE ( 'NONE', *, *, #63612, .T. ) ;
#113469 = AXIS2_PLACEMENT_3D ( 'NONE', #59916, #67093, #88705 ) ;
#113470 = AXIS2_PLACEMENT_3D ( 'NONE', #116560, #34154, #26904 ) ;
#113471 = CARTESIAN_POINT ( 'NONE',  ( 7.499999999999927169, 2.500000000000000000, -5.122947341949753763 ) ) ;
#113472 = DIRECTION ( 'NONE',  ( 0.000000000000000000, -0.9999939076577903929, 0.003490651415223739937 ) ) ;
#113473 = ORIENTED_EDGE ( 'NONE', *, *, #53289, .T. ) ;
#113474 = CIRCLE ( 'NONE', #54986, 0.06509327318403745899 ) ;
#113475 = AXIS2_PLACEMENT_3D ( 'NONE', #57005, #96937, #55094 ) ;
#113476 = ORIENTED_EDGE ( 'NONE', *, *, #56547, .T. ) ;
#113477 = VERTEX_POINT ( 'NONE', #105433 ) ;
#113478 = CARTESIAN_POINT ( 'NONE',  ( 11.64999999999990621, 12.50000000000000000, -2.165063509461101710 ) ) ;
#113479 = CARTESIAN_POINT ( 'NONE',  ( 7.899999999999921307, 12.50000000000000000, -2.385244779468109755E-15 ) ) ;
#113480 = DIRECTION ( 'NONE',  ( 0.000000000000000000, 0.000000000000000000, -1.000000000000000000 ) ) ;
#113481 = VERTEX_POINT ( 'NONE', #62923 ) ;
#113482 = CARTESIAN_POINT ( 'NONE',  ( -8.350000000000012079, 2.500000000000000000, 2.757883832488649656 ) ) ;
#113483 = DIRECTION ( 'NONE',  ( -0.000000000000000000, 1.000000000000000000, -0.000000000000000000 ) ) ;
#113484 = ORIENTED_EDGE ( 'NONE', *, *, #51210, .F. ) ;
#113486 = EDGE_CURVE ( 'NONE', #31178, #97758, #106583, .T. ) ;
#113485 = LINE ( 'NONE', #63100, #34234 ) ;
#113487 = DIRECTION ( 'NONE',  ( -0.000000000000000000, 1.000000000000000000, -0.000000000000000000 ) ) ;
#113488 = CONICAL_SURFACE ( 'NONE', #105174, 0.1000000000000002554, 0.003490658503988666988 ) ;
#113489 = CONICAL_SURFACE ( 'NONE', #46596, 0.1000000000000002554, 0.003490658503988666988 ) ;
#113490 = VECTOR ( 'NONE', #3115, 1000.000000000000000 ) ;
#113491 = FACE_OUTER_BOUND ( 'NONE', #19656, .T. ) ;
#113492 = CARTESIAN_POINT ( 'NONE',  ( 0.8499999999999527933, 12.50000000000000000, 7.122917578226811486 ) ) ;
#113493 = DIRECTION ( 'NONE',  ( 0.000000000000000000, 1.000000000000000000, 0.000000000000000000 ) ) ;
#113494 = DIRECTION ( 'NONE',  ( 0.000000000000000000, 1.000000000000000000, 0.000000000000000000 ) ) ;
#113495 = VECTOR ( 'NONE', #124775, 1000.000000000000000 ) ;
#113496 = DIRECTION ( 'NONE',  ( -0.000000000000000000, -1.000000000000000000, -0.000000000000000000 ) ) ;
#113497 = VERTEX_POINT ( 'NONE', #104755 ) ;
#113498 = CIRCLE ( 'NONE', #82112, 0.1000000000000002554 ) ;
#113499 = ORIENTED_EDGE ( 'NONE', *, *, #15275, .T. ) ;
#113500 = ORIENTED_EDGE ( 'NONE', *, *, #101081, .T. ) ;
#113501 = VERTEX_POINT ( 'NONE', #55035 ) ;
#113502 = DIRECTION ( 'NONE',  ( -4.274815082592931898E-19, -0.9999939076577903929, -0.003490651415223739937 ) ) ;
#113503 = CARTESIAN_POINT ( 'NONE',  ( -6.850000000000013856, 12.50000000000000000, 1.818653347947321475 ) ) ;
#113504 = EDGE_CURVE ( 'NONE', #126044, #23819, #73147, .T. ) ;
#113505 = DIRECTION ( 'NONE',  ( 0.000000000000000000, 0.000000000000000000, -1.000000000000000000 ) ) ;
#113506 = VERTEX_POINT ( 'NONE', #5279 ) ;
#113507 = FACE_BOUND ( 'NONE', #5455, .T. ) ;
#113508 = ADVANCED_FACE ( 'NONE', ( #85772 ), #115886, .T. ) ;
#113509 = DIRECTION ( 'NONE',  ( 0.000000000000000000, 0.000000000000000000, 1.000000000000000000 ) ) ;
#113510 = DIRECTION ( 'NONE',  ( 0.000000000000000000, -0.9999939076577903929, 0.003490651415223739937 ) ) ;
#113511 = DIRECTION ( 'NONE',  ( 0.000000000000000000, 0.000000000000000000, 1.000000000000000000 ) ) ;
#113512 = CARTESIAN_POINT ( 'NONE',  ( -8.300000000000011369, 2.500000000000000000, 0.09999999999999772959 ) ) ;
#113513 = DIRECTION ( 'NONE',  ( 0.000000000000000000, 0.000000000000000000, 1.000000000000000000 ) ) ;
#113514 = CARTESIAN_POINT ( 'NONE',  ( 2.949999999999946887, 2.500000000000000000, -2.065063509461102065 ) ) ;
#113515 = FACE_OUTER_BOUND ( 'NONE', #5674, .T. ) ;
#113516 = CARTESIAN_POINT ( 'NONE',  ( -9.550000000000007816, 12.50000000000000000, -6.495190528383297135 ) ) ;
#113517 = AXIS2_PLACEMENT_3D ( 'NONE', #114513, #72037, #124354 ) ;
#113518 = VECTOR ( 'NONE', #31999, 1000.000000000000000 ) ;
#113519 = ADVANCED_FACE ( 'NONE', ( #115210 ), #35592, .T. ) ;
#113520 = LINE ( 'NONE', #51408, #70571 ) ;
#113521 = DIRECTION ( 'NONE',  ( -0.000000000000000000, -1.000000000000000000, -0.000000000000000000 ) ) ;
#113522 = ORIENTED_EDGE ( 'NONE', *, *, #102232, .T. ) ;
#113523 = CONICAL_SURFACE ( 'NONE', #2695, 0.1000000000000002554, 0.003490658503988666988 ) ;
#113524 = ORIENTED_EDGE ( 'NONE', *, *, #71949, .T. ) ;
#113525 = ORIENTED_EDGE ( 'NONE', *, *, #46925, .T. ) ;
#113526 = ORIENTED_EDGE ( 'NONE', *, *, #90945, .T. ) ;
#113527 = AXIS2_PLACEMENT_3D ( 'NONE', #77277, #108018, #68743 ) ;
#113528 = ORIENTED_EDGE ( 'NONE', *, *, #95935, .F. ) ;
#113529 = CIRCLE ( 'NONE', #101008, 3.000000000000000000 ) ;
#113530 = EDGE_LOOP ( 'NONE', ( #40536, #26317 ) ) ;
#113531 = VECTOR ( 'NONE', #7484, 1000.000000000000000 ) ;
#113532 = CARTESIAN_POINT ( 'NONE',  ( -5.650000000000023448, 12.50000000000000000, -1.883746621131363597 ) ) ;
#113533 = VERTEX_POINT ( 'NONE', #15078 ) ;
#113534 = VERTEX_POINT ( 'NONE', #103500 ) ;
#113535 = VECTOR ( 'NONE', #59706, 1000.000000000000000 ) ;
#113536 = CIRCLE ( 'NONE', #19434, 0.06509327318403745899 ) ;
#113537 = CARTESIAN_POINT ( 'NONE',  ( 16.04744069018120811, -1.500000000000000222, 6.586254744913174974 ) ) ;
#113538 = DIRECTION ( 'NONE',  ( 0.000000000000000000, 0.000000000000000000, -1.000000000000000000 ) ) ;
#113539 = DIRECTION ( 'NONE',  ( 0.000000000000000000, 0.000000000000000000, 1.000000000000000000 ) ) ;
#113540 = CIRCLE ( 'NONE', #6899, 0.1000000000000002554 ) ;
#113541 = CONICAL_SURFACE ( 'NONE', #6902, 0.1000000000000002554, 0.003490658503988666988 ) ;
#113542 = EDGE_LOOP ( 'NONE', ( #31882, #48033, #87594, #71672 ) ) ;
#113543 = FACE_OUTER_BOUND ( 'NONE', #18661, .T. ) ;
#113544 = VECTOR ( 'NONE', #7324, 1000.000000000000000 ) ;
#113545 = ORIENTED_EDGE ( 'NONE', *, *, #82555, .F. ) ;
#113546 = EDGE_CURVE ( 'NONE', #72199, #83267, #52309, .T. ) ;
#113547 = EDGE_LOOP ( 'NONE', ( #113660, #121652 ) ) ;
#113549 = EDGE_LOOP ( 'NONE', ( #40743, #116226 ) ) ;
#113548 = LINE ( 'NONE', #63813, #99147 ) ;
#113550 = FACE_OUTER_BOUND ( 'NONE', #66142, .T. ) ;
#113551 = ADVANCED_FACE ( 'NONE', ( #24936 ), #36050, .T. ) ;
#113552 = ORIENTED_EDGE ( 'NONE', *, *, #35659, .T. ) ;
#113553 = UNCERTAINTY_MEASURE_WITH_UNIT (LENGTH_MEASURE( 1.000000000000000082E-05 ), #87993, 'distance_accuracy_value', 'NONE');
#113554 = ADVANCED_FACE ( 'NONE', ( #83841 ), #66872, .T. ) ;
#113555 = CONICAL_SURFACE ( 'NONE', #82166, 0.1000000000000002554, 0.003490658503988666988 ) ;
#113556 = DIRECTION ( 'NONE',  ( 0.000000000000000000, 0.000000000000000000, 1.000000000000000000 ) ) ;
#113557 = FACE_OUTER_BOUND ( 'NONE', #33006, .T. ) ;
#113558 = DIRECTION ( 'NONE',  ( -0.000000000000000000, -1.000000000000000000, -0.000000000000000000 ) ) ;
#113559 = CARTESIAN_POINT ( 'NONE',  ( -3.550000000000028688, 2.500000000000000000, 6.841600689897072485 ) ) ;
#113560 = EDGE_CURVE ( 'NONE', #124307, #119121, #77350, .T. ) ;
#113561 = ADVANCED_FACE ( 'NONE', ( #102832 ), #13156, .T. ) ;
#113562 = CARTESIAN_POINT ( 'NONE',  ( -7.700000000000012612, 12.50000000000000000, 4.741630453620009789 ) ) ;
#113563 = EDGE_CURVE ( 'NONE', #93080, #69989, #93038, .T. ) ;
#113564 = EDGE_CURVE ( 'NONE', #29080, #92178, #27167, .T. ) ;
#113565 = EDGE_CURVE ( 'NONE', #116268, #85461, #100340, .T. ) ;
#113567 = ORIENTED_EDGE ( 'NONE', *, *, #81293, .T. ) ;
#113566 = AXIS2_PLACEMENT_3D ( 'NONE', #37166, #8321, #88154 ) ;
#113568 = CARTESIAN_POINT ( 'NONE',  ( 7.499999999999961808, 12.50000000000000000, -4.330127018922201643 ) ) ;
#113569 = VECTOR ( 'NONE', #105619, 1000.000000000000000 ) ;
#113570 = CONICAL_SURFACE ( 'NONE', #25730, 0.1000000000000002554, 0.003490658503988666988 ) ;
#113571 = ORIENTED_EDGE ( 'NONE', *, *, #3505, .T. ) ;
#113572 = FACE_OUTER_BOUND ( 'NONE', #42371, .T. ) ;
#113573 = ADVANCED_FACE ( 'NONE', ( #23644 ), #71090, .T. ) ;
#113574 = EDGE_LOOP ( 'NONE', ( #83586, #129056 ) ) ;
#113575 = DIRECTION ( 'NONE',  ( 0.000000000000000000, 0.000000000000000000, 1.000000000000000000 ) ) ;
#113576 = FACE_OUTER_BOUND ( 'NONE', #23049, .T. ) ;
#113577 = CARTESIAN_POINT ( 'NONE',  ( 4.999999999999971578, 2.500000000000000000, -0.1000000000000022815 ) ) ;
#113579 = CONICAL_SURFACE ( 'NONE', #25844, 0.1000000000000002554, 0.003490658503988666988 ) ;
#113578 = CARTESIAN_POINT ( 'NONE',  ( 11.24999999999990763, 2.500000000000000000, -7.088010851410853519 ) ) ;
#113580 = VERTEX_POINT ( 'NONE', #3991 ) ;
#113581 = AXIS2_PLACEMENT_3D ( 'NONE', #1198, #11661, #43730 ) ;
#113582 = EDGE_CURVE ( 'NONE', #27024, #47911, #4165, .T. ) ;
#113583 = CIRCLE ( 'NONE', #109373, 0.1000000000000000056 ) ;
#113584 = DIRECTION ( 'NONE',  ( 0.000000000000000000, 0.000000000000000000, 1.000000000000000000 ) ) ;
#113585 = AXIS2_PLACEMENT_3D ( 'NONE', #55653, #95586, #5887 ) ;
#113586 = DIRECTION ( 'NONE',  ( 0.000000000000000000, 0.000000000000000000, -1.000000000000000000 ) ) ;
#113587 = ORIENTED_EDGE ( 'NONE', *, *, #48913, .T. ) ;
#113588 = ORIENTED_EDGE ( 'NONE', *, *, #93150, .T. ) ;
#113589 = VERTEX_POINT ( 'NONE', #74036 ) ;
#113590 = DIRECTION ( 'NONE',  ( 0.000000000000000000, 0.000000000000000000, -1.000000000000000000 ) ) ;
#113591 = DIRECTION ( 'NONE',  ( 0.000000000000000000, 1.000000000000000000, 0.000000000000000000 ) ) ;
#113592 = CARTESIAN_POINT ( 'NONE',  ( 184.9010416670080588, -4.367472073101519747, 7.564683531249999149 ) ) ;
#113593 = DIRECTION ( 'NONE',  ( -0.000000000000000000, -1.000000000000000000, -0.000000000000000000 ) ) ;
#113594 = CARTESIAN_POINT ( 'NONE',  ( 17.49149623775394602, 2.499999999999960920, -4.292098716152958460 ) ) ;
#113595 = AXIS2_PLACEMENT_3D ( 'NONE', #2885, #33001, #42837 ) ;
#113596 = CIRCLE ( 'NONE', #94810, 0.06509327318403745899 ) ;
#113597 = FACE_OUTER_BOUND ( 'NONE', #9804, .T. ) ;
#113598 = ORIENTED_EDGE ( 'NONE', *, *, #8623, .F. ) ;
#113599 = DIRECTION ( 'NONE',  ( 0.000000000000000000, 1.000000000000000000, 0.000000000000000000 ) ) ;
#113600 = EDGE_LOOP ( 'NONE', ( #11099, #29636 ) ) ;
#113601 = DIRECTION ( 'NONE',  ( 0.000000000000000000, 1.000000000000000000, 0.000000000000000000 ) ) ;
#113602 = FACE_OUTER_BOUND ( 'NONE', #101022, .T. ) ;
#113603 = CARTESIAN_POINT ( 'NONE',  ( 187.5000000000000000, 9.429780353434619030E-16, -7.700000000000000178 ) ) ;
#113604 = DIRECTION ( 'NONE',  ( 0.000000000000000000, 0.000000000000000000, 1.000000000000000000 ) ) ;
#113605 = EDGE_LOOP ( 'NONE', ( #38721, #128381, #25308, #119551 ) ) ;
#113606 = EDGE_CURVE ( 'NONE', #26142, #30816, #87796, .T. ) ;
#113607 = CARTESIAN_POINT ( 'NONE',  ( 4.549999999999939426, 2.500000000000000000, -2.165063509461101710 ) ) ;
#113609 = ORIENTED_EDGE ( 'NONE', *, *, #103718, .T. ) ;
#113608 = DIRECTION ( 'NONE',  ( 0.000000000000000000, -0.9999939076577903929, 0.003490651415223739937 ) ) ;
#113610 = AXIS2_PLACEMENT_3D ( 'NONE', #28083, #94885, #96165 ) ;
#113611 = AXIS2_PLACEMENT_3D ( 'NONE', #69095, #6929, #88068 ) ;
#113612 = ORIENTED_EDGE ( 'NONE', *, *, #102904, .T. ) ;
#113613 = CARTESIAN_POINT ( 'NONE',  ( 6.649999999999931966, 12.50000000000000000, -7.188010851410854052 ) ) ;
#113614 = ADVANCED_FACE ( 'NONE', ( #26230 ), #36704, .T. ) ;
#113615 = CONICAL_SURFACE ( 'NONE', #73808, 0.1000000000000002554, 0.003490658503988666988 ) ;
#113616 = VECTOR ( 'NONE', #78662, 1000.000000000000000 ) ;
#113617 = ORIENTED_EDGE ( 'NONE', *, *, #110853, .F. ) ;
#113618 = CONICAL_SURFACE ( 'NONE', #59264, 0.09999999999999982514, 0.003490658503988666988 ) ;
#113619 = EDGE_LOOP ( 'NONE', ( #63438, #67450 ) ) ;
#113620 = LINE ( 'NONE', #95276, #27838 ) ;
#113621 = AXIS2_PLACEMENT_3D ( 'NONE', #95359, #103887, #66524 ) ;
#113622 = CONICAL_SURFACE ( 'NONE', #6990, 0.09999999999999982514, 0.003490658503988666988 ) ;
#113623 = ORIENTED_EDGE ( 'NONE', *, *, #34, .F. ) ;
#113624 = CARTESIAN_POINT ( 'NONE',  ( 16.58100817950494843, 2.557139044001659478, -6.067820687733441076 ) ) ;
#113625 = DIRECTION ( 'NONE',  ( 0.000000000000000000, 0.000000000000000000, 1.000000000000000000 ) ) ;
#113626 = LINE ( 'NONE', #52765, #77125 ) ;
#113628 = ORIENTED_EDGE ( 'NONE', *, *, #127740, .T. ) ;
#113627 = CIRCLE ( 'NONE', #115672, 0.06509327318403745899 ) ;
#113629 = AXIS2_PLACEMENT_3D ( 'NONE', #61730, #102913, #13883 ) ;
#113630 = AXIS2_PLACEMENT_3D ( 'NONE', #15920, #44765, #84674 ) ;
#113631 = LINE ( 'NONE', #23965, #81711 ) ;
#113633 = VERTEX_POINT ( 'NONE', #87708 ) ;
#113632 = CARTESIAN_POINT ( 'NONE',  ( -3.000000000000000000, 3.673940397442059868E-16, -5.000000000000004441 ) ) ;
#113634 = AXIS2_PLACEMENT_3D ( 'NONE', #4551, #53056, #23580 ) ;
#113635 = DIRECTION ( 'NONE',  ( 0.000000000000000000, -0.000000000000000000, 1.000000000000000000 ) ) ;
#113636 = DIRECTION ( 'NONE',  ( 0.000000000000000000, 1.000000000000000000, 0.000000000000000000 ) ) ;
#113637 = VERTEX_POINT ( 'NONE', #106701 ) ;
#113638 = EDGE_LOOP ( 'NONE', ( #8358, #118631 ) ) ;
#113639 = ORIENTED_EDGE ( 'NONE', *, *, #31681, .F. ) ;
#113640 = ORIENTED_EDGE ( 'NONE', *, *, #34157, .T. ) ;
#113641 = CARTESIAN_POINT ( 'NONE',  ( -3.550000000000028688, 12.50000000000000000, 6.841600689897072485 ) ) ;
#113642 = DIRECTION ( 'NONE',  ( -0.000000000000000000, -1.000000000000000000, -0.000000000000000000 ) ) ;
#113643 =( BOUNDED_CURVE ( )  B_SPLINE_CURVE ( 2, ( #122949, #111842, #14263 ),
 .UNSPECIFIED., .F., .F. ) 
 B_SPLINE_CURVE_WITH_KNOTS ( ( 3, 3 ),
 ( 0.7857142857142862535, 0.7948312917401810784 ),
 .UNSPECIFIED. ) 
 CURVE ( )  GEOMETRIC_REPRESENTATION_ITEM ( )  RATIONAL_B_SPLINE_CURVE ( ( 0.9999999999999968914, 0.9486992175574040509, 0.9366860366984419706 ) ) 
 REPRESENTATION_ITEM ( '' )  );
#113644 = CARTESIAN_POINT ( 'NONE',  ( 186.2500000000000000, 9.429780353434619030E-16, -7.700000000000000178 ) ) ;
#113645 = FACE_BOUND ( 'NONE', #117169, .T. ) ;
#113646 = ORIENTED_EDGE ( 'NONE', *, *, #68950, .F. ) ;
#113647 = CARTESIAN_POINT ( 'NONE',  ( 184.7812500006828031, 0.000000000000000000, 7.700000000000000178 ) ) ;
#113648 = FACE_OUTER_BOUND ( 'NONE', #75425, .T. ) ;
#113649 = CARTESIAN_POINT ( 'NONE',  ( 11.04999999999991012, 12.50000000000000000, 6.841600689897072485 ) ) ;
#113650 = CIRCLE ( 'NONE', #2837, 0.06509327318403745899 ) ;
#113651 = ADVANCED_FACE ( 'NONE', ( #37972 ), #96234, .T. ) ;
#113652 = CARTESIAN_POINT ( 'NONE',  ( 6.649999999999931077, 2.500000000000000000, -6.495190528383302464 ) ) ;
#113653 = CARTESIAN_POINT ( 'NONE',  ( 3.949999999999938005, 12.50000000000000000, 6.906693963081109722 ) ) ;
#113654 = LINE ( 'NONE', #61988, #103473 ) ;
#113655 = AXIS2_PLACEMENT_3D ( 'NONE', #122801, #45539, #22683 ) ;
#113656 = CIRCLE ( 'NONE', #65528, 0.06509327318403745899 ) ;
#113657 = EDGE_CURVE ( 'NONE', #82898, #76941, #64818, .T. ) ;
#113658 = AXIS2_PLACEMENT_3D ( 'NONE', #8178, #68391, #126680 ) ;
#113659 = DIRECTION ( 'NONE',  ( 1.000000000000000000, 0.000000000000000000, 0.000000000000000000 ) ) ;
#113660 = ORIENTED_EDGE ( 'NONE', *, *, #60713, .F. ) ;
#113661 = ORIENTED_EDGE ( 'NONE', *, *, #11123, .F. ) ;
#113662 = ORIENTED_EDGE ( 'NONE', *, *, #123008, .T. ) ;
#113663 = VERTEX_POINT ( 'NONE', #86420 ) ;
#113664 = ORIENTED_EDGE ( 'NONE', *, *, #115408, .F. ) ;
#113665 = DIRECTION ( 'NONE',  ( 0.000000000000000000, 0.000000000000000000, 1.000000000000000000 ) ) ;
#113666 = EDGE_CURVE ( 'NONE', #11828, #76998, #98267, .T. ) ;
#113667 = DIRECTION ( 'NONE',  ( -0.000000000000000000, -1.000000000000000000, -0.000000000000000000 ) ) ;
#113668 = EDGE_LOOP ( 'NONE', ( #26683, #15957, #26993, #124007 ) ) ;
#113669 = FACE_BOUND ( 'NONE', #28483, .T. ) ;
#113670 = AXIS2_PLACEMENT_3D ( 'NONE', #39781, #453, #8994 ) ;
#113671 = ADVANCED_FACE ( 'NONE', ( #128308 ), #77886, .T. ) ;
#113672 = AXIS2_PLACEMENT_3D ( 'NONE', #61267, #31806, #41645 ) ;
#113673 = FACE_OUTER_BOUND ( 'NONE', #4701, .T. ) ;
#113674 = CIRCLE ( 'NONE', #57234, 0.1000000000000002554 ) ;
#113675 = CIRCLE ( 'NONE', #128363, 3.000000000000000000 ) ;
#113676 = EDGE_CURVE ( 'NONE', #19759, #113210, #83988, .T. ) ;
#113677 = ORIENTED_EDGE ( 'NONE', *, *, #13068, .T. ) ;
#113678 = DIRECTION ( 'NONE',  ( -0.000000000000000000, 1.000000000000000000, -0.000000000000000000 ) ) ;
#113679 = LINE ( 'NONE', #52179, #115800 ) ;
#113680 = EDGE_CURVE ( 'NONE', #49878, #59844, #26868, .T. ) ;
#113681 = DIRECTION ( 'NONE',  ( 0.000000000000000000, 0.000000000000000000, 1.000000000000000000 ) ) ;
#113682 = CIRCLE ( 'NONE', #51001, 0.06509327318403745899 ) ;
#113683 = ORIENTED_EDGE ( 'NONE', *, *, #32597, .T. ) ;
#113684 = FACE_OUTER_BOUND ( 'NONE', #23022, .T. ) ;
#113685 = ORIENTED_EDGE ( 'NONE', *, *, #96861, .T. ) ;
#113686 = AXIS2_PLACEMENT_3D ( 'NONE', #26398, #105600, #66302 ) ;
#113687 = AXIS2_PLACEMENT_3D ( 'NONE', #89910, #108891, #78173 ) ;
#113688 = ORIENTED_EDGE ( 'NONE', *, *, #3767, .F. ) ;
#113689 = VERTEX_POINT ( 'NONE', #116526 ) ;
#113690 = CARTESIAN_POINT ( 'NONE',  ( -11.25000000000000000, 12.50000000000000000, 2.857883832488649301 ) ) ;
#113691 = CYLINDRICAL_SURFACE ( 'NONE', #28851, 3.000000000000000000 ) ;
#113693 = AXIS2_PLACEMENT_3D ( 'NONE', #10001, #17877, #108188 ) ;
#113692 = DIRECTION ( 'NONE',  ( 0.000000000000000000, 0.000000000000000000, -1.000000000000000000 ) ) ;
#113694 = ORIENTED_EDGE ( 'NONE', *, *, #63324, .F. ) ;
#113695 = DIRECTION ( 'NONE',  ( -0.000000000000000000, 1.000000000000000000, -0.000000000000000000 ) ) ;
#113696 = VECTOR ( 'NONE', #115389, 1000.000000000000000 ) ;
#113697 = DIRECTION ( 'NONE',  ( -0.000000000000000000, -1.000000000000000000, -0.000000000000000000 ) ) ;
#113698 = CARTESIAN_POINT ( 'NONE',  ( 2.499999999999947153, 12.50000000000000000, 0.6928203230275494784 ) ) ;
#113699 = CARTESIAN_POINT ( 'NONE',  ( 185.4895833340161175, -4.445597072760115509, -7.700000000000001954 ) ) ;
#113700 = ORIENTED_EDGE ( 'NONE', *, *, #38869, .T. ) ;
#113701 = FACE_OUTER_BOUND ( 'NONE', #60609, .T. ) ;
#113702 = ORIENTED_EDGE ( 'NONE', *, *, #5535, .F. ) ;
#113703 = DIRECTION ( 'NONE',  ( 0.000000000000000000, 0.000000000000000000, -1.000000000000000000 ) ) ;
#113704 = VERTEX_POINT ( 'NONE', #67401 ) ;
#113705 = VERTEX_POINT ( 'NONE', #46495 ) ;
#113706 = CARTESIAN_POINT ( 'NONE',  ( -5.850000000000019185, 2.500000000000000000, 6.495190528383297135 ) ) ;
#113707 = CARTESIAN_POINT ( 'NONE',  ( 9.999999999999948486, 2.500000000000000000, 4.330127018922196314 ) ) ;
#113708 = CIRCLE ( 'NONE', #111550, 0.06509327318403745899 ) ;
#113709 = FACE_OUTER_BOUND ( 'NONE', #39002, .T. ) ;
#113710 = VECTOR ( 'NONE', #17560, 1000.000000000000000 ) ;
#113711 = CARTESIAN_POINT ( 'NONE',  ( 5.399999999999934630, 2.500000000000000000, -0.7928203230275543412 ) ) ;
#113712 = CARTESIAN_POINT ( 'NONE',  ( 184.4999999999999716, -5.087293621995115700, -5.751705878905746694 ) ) ;
#113713 = ORIENTED_EDGE ( 'NONE', *, *, #110310, .F. ) ;
#113714 = ORIENTED_EDGE ( 'NONE', *, *, #76389, .F. ) ;
#113715 = CARTESIAN_POINT ( 'NONE',  ( 105.6184301395928031, 9.000000000000001776, 1.375000000000001110 ) ) ;
#113716 = AXIS2_PLACEMENT_3D ( 'NONE', #36369, #116827, #26529 ) ;
#113717 = CONICAL_SURFACE ( 'NONE', #80273, 0.1000000000000002554, 0.003490658503988666988 ) ;
#113718 = CONICAL_SURFACE ( 'NONE', #109513, 0.1000000000000000472, 0.003490658503988666988 ) ;
#113719 = CARTESIAN_POINT ( 'NONE',  ( 0.5999999999999551248, 2.500000000000000000, -4.776537180435978414 ) ) ;
#113720 = CONICAL_SURFACE ( 'NONE', #57282, 0.1000000000000002554, 0.003490658503988666988 ) ;
#113722 = ADVANCED_FACE ( 'NONE', ( #38647 ), #66777, .T. ) ;
#113721 = CARTESIAN_POINT ( 'NONE',  ( -5.600000000000020073, 2.500000000000000000, 3.883716857408421319 ) ) ;
#113723 = ORIENTED_EDGE ( 'NONE', *, *, #70162, .T. ) ;
#113724 = ORIENTED_EDGE ( 'NONE', *, *, #33492, .F. ) ;
#113725 = ADVANCED_FACE ( 'NONE', ( #49104 ), #56314, .T. ) ;
#113726 = DIRECTION ( 'NONE',  ( 0.000000000000000000, 1.000000000000000000, 0.000000000000000000 ) ) ;
#113727 = EDGE_CURVE ( 'NONE', #46092, #116053, #17678, .T. ) ;
#113728 = EDGE_CURVE ( 'NONE', #44827, #86121, #65116, .T. ) ;
#113729 = ORIENTED_EDGE ( 'NONE', *, *, #93828, .T. ) ;
#113730 = DIRECTION ( 'NONE',  ( -0.000000000000000000, 1.000000000000000000, -0.000000000000000000 ) ) ;
#113731 = AXIS2_PLACEMENT_3D ( 'NONE', #109921, #71266, #52285 ) ;
#113732 = AXIS2_PLACEMENT_3D ( 'NONE', #63513, #104699, #103434 ) ;
#113733 = AXIS2_PLACEMENT_3D ( 'NONE', #126386, #54410, #116553 ) ;
#113734 = CARTESIAN_POINT ( 'NONE',  ( -11.44999999999999929, 2.500000000000000000, -1.818653347947322141 ) ) ;
#113735 = ORIENTED_EDGE ( 'NONE', *, *, #12190, .F. ) ;
#113736 = DIRECTION ( 'NONE',  ( -0.000000000000000000, 1.000000000000000000, -0.000000000000000000 ) ) ;
#113737 = EDGE_CURVE ( 'NONE', #13514, #46605, #87064, .T. ) ;
#113738 = CARTESIAN_POINT ( 'NONE',  ( -8.350000000000010303, 2.500000000000000000, 6.395190528383296602 ) ) ;
#113739 = DIRECTION ( 'NONE',  ( 0.000000000000000000, -0.9999939076577903929, 0.003490651415223739937 ) ) ;
#113740 = AXIS2_PLACEMENT_3D ( 'NONE', #27435, #97480, #68017 ) ;
#113741 = FACE_OUTER_BOUND ( 'NONE', #99625, .T. ) ;
#113742 = ORIENTED_EDGE ( 'NONE', *, *, #50030, .T. ) ;
#113743 = EDGE_CURVE ( 'NONE', #32290, #31868, #98556, .T. ) ;
#113744 = CARTESIAN_POINT ( 'NONE',  ( 10.84999999999990905, 2.500000000000000000, -6.395190528383301931 ) ) ;
#113745 = EDGE_CURVE ( 'NONE', #22907, #114764, #75586, .T. ) ;
#113746 = DIRECTION ( 'NONE',  ( -0.000000000000000000, 1.000000000000000000, -0.000000000000000000 ) ) ;
#113747 = CONICAL_SURFACE ( 'NONE', #100912, 0.1000000000000000472, 0.003490658503988666988 ) ;
#113748 = ORIENTED_EDGE ( 'NONE', *, *, #118887, .T. ) ;
#113749 = VERTEX_POINT ( 'NONE', #47806 ) ;
#113750 = CARTESIAN_POINT ( 'NONE',  ( 184.6510416670080588, 4.367472073101518859, -7.564683531249999149 ) ) ;
#113751 = CARTESIAN_POINT ( 'NONE',  ( 7.699999999999925571, 12.50000000000000000, -4.741630453620016006 ) ) ;
#113752 = CARTESIAN_POINT ( 'NONE',  ( -7.900000000000014566, 2.500000000000000000, -0.6928203230275541413 ) ) ;
#113753 = AXIS2_PLACEMENT_3D ( 'NONE', #117154, #105434, #5280 ) ;
#113754 = CARTESIAN_POINT ( 'NONE',  ( -12.29999999999999538, 12.50000000000000000, -4.611443907251937979 ) ) ;
#113755 = DIRECTION ( 'NONE',  ( 0.000000000000000000, 1.000000000000000000, 0.000000000000000000 ) ) ;
#113756 = DIRECTION ( 'NONE',  ( 0.000000000000000000, -0.9999939076577903929, 0.003490651415223739937 ) ) ;
#113757 = CARTESIAN_POINT ( 'NONE',  ( -13.74999999999998757, 2.500000000000000000, 1.572243186433549544 ) ) ;
#113758 = CARTESIAN_POINT ( 'NONE',  ( 1.849999999999950129, 2.500000000000000000, -6.841600689897078702 ) ) ;
#113759 = CARTESIAN_POINT ( 'NONE',  ( -12.09999999999999609, 12.50000000000000000, -4.330127018922198978 ) ) ;
#113760 = FACE_OUTER_BOUND ( 'NONE', #49510, .T. ) ;
#113762 = AXIS2_PLACEMENT_3D ( 'NONE', #53774, #125094, #93703 ) ;
#113761 = CARTESIAN_POINT ( 'NONE',  ( -1.050000000000038236, 2.500000000000000000, -6.248780366869526759 ) ) ;
#113763 = ORIENTED_EDGE ( 'NONE', *, *, #26068, .F. ) ;
#113764 = CONICAL_SURFACE ( 'NONE', #32207, 0.09999999999999982514, 0.003490658503988666988 ) ;
#113765 = EDGE_LOOP ( 'NONE', ( #112267, #21474 ) ) ;
#113766 = EDGE_LOOP ( 'NONE', ( #86824, #129380 ) ) ;
#113767 = ORIENTED_EDGE ( 'NONE', *, *, #16899, .F. ) ;
#113768 = CARTESIAN_POINT ( 'NONE',  ( 13.29999999999990301, 12.50000000000000000, -4.265033745738164406 ) ) ;
#113769 = LINE ( 'NONE', #117427, #58496 ) ;
#113770 = ORIENTED_EDGE ( 'NONE', *, *, #25401, .T. ) ;
#113771 = CARTESIAN_POINT ( 'NONE',  ( -12.94999999999999218, 12.50000000000000000, 2.230156782645138946 ) ) ;
#113772 = VECTOR ( 'NONE', #19261, 1000.000000000000000 ) ;
#113773 = CARTESIAN_POINT ( 'NONE',  ( 8.349999999999923261, 12.50000000000000000, -7.122917578226816815 ) ) ;
#113775 = ORIENTED_EDGE ( 'NONE', *, *, #59366, .T. ) ;
#113774 = LINE ( 'NONE', #22826, #13987 ) ;
#113776 = CARTESIAN_POINT ( 'NONE',  ( -12.09999999999999609, 2.500000000000000000, -0.6928203230275501445 ) ) ;
#113777 = FACE_OUTER_BOUND ( 'NONE', #2245, .T. ) ;
#113778 = VERTEX_POINT ( 'NONE', #68073 ) ;
#113779 = EDGE_CURVE ( 'NONE', #21428, #32421, #33826, .T. ) ;
#113780 = CIRCLE ( 'NONE', #26040, 0.06509327318403745899 ) ;
#113781 = CIRCLE ( 'NONE', #82399, 0.06509327318403745899 ) ;
#113782 = ORIENTED_EDGE ( 'NONE', *, *, #124215, .F. ) ;
#113783 = ORIENTED_EDGE ( 'NONE', *, *, #114850, .T. ) ;
#113784 = ORIENTED_EDGE ( 'NONE', *, *, #89307, .T. ) ;
#113785 = CARTESIAN_POINT ( 'NONE',  ( -4.999999999999986677, 2.500000000000000000, 4.430127018922196847 ) ) ;
#113786 = AXIS2_PLACEMENT_3D ( 'NONE', #104177, #35449, #14484 ) ;
#113787 = CARTESIAN_POINT ( 'NONE',  ( -0.4000000000000404898, 2.500000000000000000, 5.122947341949749323 ) ) ;
#113788 = FACE_OUTER_BOUND ( 'NONE', #122944, .T. ) ;
#113789 = VECTOR ( 'NONE', #93366, 1000.000000000000000 ) ;
#113790 = DIRECTION ( 'NONE',  ( -0.000000000000000000, 1.000000000000000000, -0.000000000000000000 ) ) ;
#113791 = ORIENTED_EDGE ( 'NONE', *, *, #97949, .T. ) ;
#113792 = DIRECTION ( 'NONE',  ( 0.000000000000000000, 1.000000000000000000, 0.000000000000000000 ) ) ;
#113793 = ORIENTED_EDGE ( 'NONE', *, *, #11878, .T. ) ;
#113794 = DIRECTION ( 'NONE',  ( 0.000000000000000000, -0.000000000000000000, 1.000000000000000000 ) ) ;
#113795 = CARTESIAN_POINT ( 'NONE',  ( 10.61495711640258932, -2.500000000000000888, -8.020491764208069085 ) ) ;
#113796 = LINE ( 'NONE', #64045, #123700 ) ;
#113797 = PLANE ( 'NONE',  #4501 ) ;
#113798 = ORIENTED_EDGE ( 'NONE', *, *, #67748, .T. ) ;
#113799 = CIRCLE ( 'NONE', #114083, 0.06509327318403741736 ) ;
#113800 = ORIENTED_EDGE ( 'NONE', *, *, #13874, .F. ) ;
#113801 = VECTOR ( 'NONE', #5704, 1000.000000000000000 ) ;
#113802 = ORIENTED_EDGE ( 'NONE', *, *, #85171, .F. ) ;
#113803 = CARTESIAN_POINT ( 'NONE',  ( -9.150000000000009237, 12.50000000000000000, 2.165063509461097713 ) ) ;
#113805 = CIRCLE ( 'NONE', #124268, 0.1000000000000000472 ) ;
#113804 = CARTESIAN_POINT ( 'NONE',  ( -12.94999999999999218, 12.50000000000000000, -2.165063509461099489 ) ) ;
#113806 = CONICAL_SURFACE ( 'NONE', #57365, 0.1000000000000002554, 0.003490658503988666988 ) ;
#113807 = CARTESIAN_POINT ( 'NONE',  ( -1.850000000000033840, 12.50000000000000000, 6.083687093685483660 ) ) ;
#113808 = FACE_BOUND ( 'NONE', #123694, .T. ) ;
#113809 = DIRECTION ( 'NONE',  ( 0.000000000000000000, 0.000000000000000000, -1.000000000000000000 ) ) ;
#113810 = DIRECTION ( 'NONE',  ( 0.000000000000000000, 1.000000000000000000, 0.000000000000000000 ) ) ;
#113811 = CARTESIAN_POINT ( 'NONE',  ( 0.000000000000000000, 2.500000000000000000, 9.000000000000001776 ) ) ;
#113812 = AXIS2_PLACEMENT_3D ( 'NONE', #12287, #52234, #62703 ) ;
#113813 = CIRCLE ( 'NONE', #936, 0.06509327318403745899 ) ;
#113814 = FACE_OUTER_BOUND ( 'NONE', #74625, .T. ) ;
#113815 = CARTESIAN_POINT ( 'NONE',  ( -1.050000000000037348, 2.500000000000000000, -6.741600689897078169 ) ) ;
#113816 = ORIENTED_EDGE ( 'NONE', *, *, #86413, .T. ) ;
#113817 = CIRCLE ( 'NONE', #15506, 0.1000000000000002554 ) ;
#113819 = EDGE_CURVE ( 'NONE', #93646, #81193, #68717, .T. ) ;
#113818 = CONICAL_SURFACE ( 'NONE', #101300, 0.09999999999999982514, 0.003490658503988666988 ) ;
#113820 = FACE_OUTER_BOUND ( 'NONE', #33009, .T. ) ;
#113821 = EDGE_LOOP ( 'NONE', ( #21129, #113321 ) ) ;
#113822 = ORIENTED_EDGE ( 'NONE', *, *, #73057, .F. ) ;
#113823 = ORIENTED_EDGE ( 'NONE', *, *, #75693, .T. ) ;
#113824 = EDGE_LOOP ( 'NONE', ( #36542, #39023, #52823, #93255 ) ) ;
#113825 = AXIS2_PLACEMENT_3D ( 'NONE', #46956, #66563, #18113 ) ;
#113826 = EDGE_CURVE ( 'NONE', #24484, #112609, #42152, .T. ) ;
#113827 = CARTESIAN_POINT ( 'NONE',  ( 13.09999999999990195, 2.500000000000000000, 4.083716857408420609 ) ) ;
#113828 = FACE_BOUND ( 'NONE', #20583, .T. ) ;
#113829 = ADVANCED_FACE ( 'NONE', ( #19633 ), #11735, .T. ) ;
#113830 = DIRECTION ( 'NONE',  ( -0.000000000000000000, 1.000000000000000000, -0.000000000000000000 ) ) ;
#113831 = EDGE_CURVE ( 'NONE', #125498, #7881, #25402, .T. ) ;
#113832 = ADVANCED_FACE ( 'NONE', ( #109290 ), #49752, .T. ) ;
#113833 = ORIENTED_EDGE ( 'NONE', *, *, #82549, .F. ) ;
#113834 = CARTESIAN_POINT ( 'NONE',  ( -8.100000000000013856, 12.50000000000000000, 0.4115034346978110880 ) ) ;
#113835 = EDGE_CURVE ( 'NONE', #70628, #41760, #12875, .T. ) ;
#113836 = EDGE_CURVE ( 'NONE', #81889, #51160, #100717, .T. ) ;
#113837 = DIRECTION ( 'NONE',  ( 0.000000000000000000, 1.000000000000000000, 0.000000000000000000 ) ) ;
#113838 = EDGE_CURVE ( 'NONE', #87808, #69735, #39925, .T. ) ;
#113840 = ORIENTED_EDGE ( 'NONE', *, *, #32447, .T. ) ;
#113839 = AXIS2_PLACEMENT_3D ( 'NONE', #67613, #27065, #107559 ) ;
#113841 = DIRECTION ( 'NONE',  ( 0.000000000000000000, 0.000000000000000000, -1.000000000000000000 ) ) ;
#113842 = DIRECTION ( 'NONE',  ( -0.000000000000000000, -1.000000000000000000, -0.000000000000000000 ) ) ;
#113843 = ORIENTED_EDGE ( 'NONE', *, *, #120655, .F. ) ;
#113844 = DIRECTION ( 'NONE',  ( 0.000000000000000000, 1.000000000000000000, 0.000000000000000000 ) ) ;
#113846 = EDGE_CURVE ( 'NONE', #80552, #64315, #79828, .T. ) ;
#113845 = CARTESIAN_POINT ( 'NONE',  ( -5.850000000000018296, 2.500000000000000000, 5.902370205355745192 ) ) ;
#113847 = AXIS2_PLACEMENT_3D ( 'NONE', #82938, #94033, #71167 ) ;
#113848 = AXIS2_PLACEMENT_3D ( 'NONE', #9810, #58913, #98825 ) ;
#113849 = ORIENTED_EDGE ( 'NONE', *, *, #98895, .T. ) ;
#113850 = DIRECTION ( 'NONE',  ( -0.000000000000000000, 1.000000000000000000, -0.000000000000000000 ) ) ;
#113851 = DIRECTION ( 'NONE',  ( -0.000000000000000000, 1.000000000000000000, -0.000000000000000000 ) ) ;
#113852 = DIRECTION ( 'NONE',  ( 0.000000000000000000, 0.000000000000000000, 1.000000000000000000 ) ) ;
#113853 = ORIENTED_EDGE ( 'NONE', *, *, #120655, .T. ) ;
#113854 = ORIENTED_EDGE ( 'NONE', *, *, #52411, .T. ) ;
#113855 = CARTESIAN_POINT ( 'NONE',  ( -10.60000000000000320, 2.500000000000000000, -4.576537180435972907 ) ) ;
#113856 = EDGE_LOOP ( 'NONE', ( #68550, #79287 ) ) ;
#113857 = CARTESIAN_POINT ( 'NONE',  ( -8.100000000000013856, 2.500000000000000000, -3.883716857408426648 ) ) ;
#113858 = CARTESIAN_POINT ( 'NONE',  ( -0.8500000000000382805, 2.500000000000000000, -2.857883832488653741 ) ) ;
#113859 = CONICAL_SURFACE ( 'NONE', #111811, 0.1000000000000002554, 0.003490658503988666988 ) ;
#113860 = VERTEX_POINT ( 'NONE', #41224 ) ;
#113862 = CARTESIAN_POINT ( 'NONE',  ( 7.949999999999925571, 2.500000000000000000, -6.595190528383302109 ) ) ;
#113861 = AXIS2_PLACEMENT_3D ( 'NONE', #6568, #106730, #36071 ) ;
#113863 = LINE ( 'NONE', #64106, #108876 ) ;
#113864 = DIRECTION ( 'NONE',  ( 0.000000000000000000, 0.000000000000000000, 1.000000000000000000 ) ) ;
#113865 = FACE_OUTER_BOUND ( 'NONE', #120858, .T. ) ;
#113866 = DIRECTION ( 'NONE',  ( 0.000000000000000000, 0.000000000000000000, 1.000000000000000000 ) ) ;
#113867 = ORIENTED_EDGE ( 'NONE', *, *, #25902, .T. ) ;
#113868 = VERTEX_POINT ( 'NONE', #119754 ) ;
#113869 = CARTESIAN_POINT ( 'NONE',  ( -6.249999999999984901, 2.500000000000000000, -2.165063509461101710 ) ) ;
#113870 = CIRCLE ( 'NONE', #74165, 0.06509327318403745899 ) ;
#113871 = CIRCLE ( 'NONE', #94999, 0.1000000000000002554 ) ;
#113872 = CARTESIAN_POINT ( 'NONE',  ( 104.0411730856320389, 7.066873072444588288, -3.070937804656772130 ) ) ;
#113874 = ORIENTED_EDGE ( 'NONE', *, *, #56633, .F. ) ;
#113873 = VERTEX_POINT ( 'NONE', #69355 ) ;
#113875 = VERTEX_POINT ( 'NONE', #81136 ) ;
#113876 = CIRCLE ( 'NONE', #105268, 0.06509327318403745899 ) ;
#113877 = EDGE_CURVE ( 'NONE', #88394, #35493, #69319, .T. ) ;
#113878 = DIRECTION ( 'NONE',  ( 0.000000000000000000, 1.000000000000000000, 0.000000000000000000 ) ) ;
#113879 = ADVANCED_FACE ( 'NONE', ( #20268 ), #121045, .T. ) ;
#113880 = CIRCLE ( 'NONE', #57442, 0.09999999999999982514 ) ;
#113881 = DIRECTION ( 'NONE',  ( 0.000000000000000000, 1.000000000000000000, 0.000000000000000000 ) ) ;
#113882 = CARTESIAN_POINT ( 'NONE',  ( 4.149999999999941735, 2.500000000000000000, -5.902370205355750521 ) ) ;
#113883 = EDGE_CURVE ( 'NONE', #50530, #55864, #44287, .T. ) ;
#113884 = DIRECTION ( 'NONE',  ( 0.000000000000000000, 0.000000000000000000, 1.000000000000000000 ) ) ;
#113885 = DIRECTION ( 'NONE',  ( 0.000000000000000000, 0.000000000000000000, 1.000000000000000000 ) ) ;
#113886 = DIRECTION ( 'NONE',  ( 0.000000000000000000, 0.000000000000000000, 1.000000000000000000 ) ) ;
#113887 = CARTESIAN_POINT ( 'NONE',  ( 154.1524742528378056, 0.5000000000000000000, -1.703575533167231537 ) ) ;
#113888 = CARTESIAN_POINT ( 'NONE',  ( -9.999999999999971578, 2.500000000000000000, -4.330127018922197202 ) ) ;
#113889 = DIRECTION ( 'NONE',  ( -0.000000000000000000, 1.000000000000000000, -0.000000000000000000 ) ) ;
#113890 = EDGE_CURVE ( 'NONE', #57147, #100871, #61504, .T. ) ;
#113891 = CARTESIAN_POINT ( 'NONE',  ( 14.14999999999989377, 2.500000000000000000, -1.472243186433550122 ) ) ;
#113892 = ADVANCED_FACE ( 'NONE', ( #90274 ), #73526, .T. ) ;
#113894 = VERTEX_POINT ( 'NONE', #80497 ) ;
#113893 = ADVANCED_FACE ( 'NONE', ( #29453 ), #50372, .T. ) ;
#113895 = ADVANCED_FACE ( 'NONE', ( #70656 ), #48409, .T. ) ;
#113896 = AXIS2_PLACEMENT_3D ( 'NONE', #59521, #99432, #71234 ) ;
#113897 = VECTOR ( 'NONE', #128078, 1000.000000000000000 ) ;
#113898 = DIRECTION ( 'NONE',  ( 0.000000000000000000, -0.9999939076577903929, 0.003490651415223739937 ) ) ;
#113899 = AXIS2_PLACEMENT_3D ( 'NONE', #19895, #48713, #57889 ) ;
#113900 = CIRCLE ( 'NONE', #90905, 0.1000000000000000472 ) ;
#113901 = ORIENTED_EDGE ( 'NONE', *, *, #124437, .F. ) ;
#113902 = ORIENTED_EDGE ( 'NONE', *, *, #5208, .T. ) ;
#113903 = CARTESIAN_POINT ( 'NONE',  ( -14.34999999999998543, 2.500000000000000000, 2.511473670974877503 ) ) ;
#113904 = LINE ( 'NONE', #24226, #99063 ) ;
#113905 = LINE ( 'NONE', #104700, #123897 ) ;
#113906 = EDGE_CURVE ( 'NONE', #15576, #100404, #115275, .T. ) ;
#113907 = CARTESIAN_POINT ( 'NONE',  ( 186.5416666666666572, -4.445597072760092416, 7.700000000000049916 ) ) ;
#113909 = DIRECTION ( 'NONE',  ( 0.000000000000000000, 1.000000000000000000, 0.000000000000000000 ) ) ;
#113908 = AXIS2_PLACEMENT_3D ( 'NONE', #102315, #82015, #42771 ) ;
#113910 = CARTESIAN_POINT ( 'NONE',  ( 9.599999999999914380, 2.500000000000000000, 3.637306695894644726 ) ) ;
#113911 = DIRECTION ( 'NONE',  ( 0.000000000000000000, 0.000000000000000000, 1.000000000000000000 ) ) ;
#113912 = ORIENTED_EDGE ( 'NONE', *, *, #41630, .T. ) ;
#113913 = FACE_OUTER_BOUND ( 'NONE', #38096, .T. ) ;
#113914 = CIRCLE ( 'NONE', #120263, 0.1000000000000002554 ) ;
#113915 = CARTESIAN_POINT ( 'NONE',  ( 6.449999999999931788, 12.50000000000000000, 6.213873640053558134 ) ) ;
#113917 = EDGE_LOOP ( 'NONE', ( #129445, #61257 ) ) ;
#113916 = AXIS2_PLACEMENT_3D ( 'NONE', #39073, #8282, #78341 ) ;
#113918 = VERTEX_POINT ( 'NONE', #5131 ) ;
#113919 = VERTEX_POINT ( 'NONE', #103355 ) ;
#113920 = ADVANCED_FACE ( 'NONE', ( #35262 ), #22870, .F. ) ;
#113921 = VERTEX_POINT ( 'NONE', #105277 ) ;
#113922 = CARTESIAN_POINT ( 'NONE',  ( 8.099999999999921485, 2.500000000000000000, -0.2464101615137783419 ) ) ;
#113923 = LINE ( 'NONE', #94265, #58221 ) ;
#113924 = DIRECTION ( 'NONE',  ( 0.000000000000000000, 0.000000000000000000, 1.000000000000000000 ) ) ;
#113925 = CARTESIAN_POINT ( 'NONE',  ( 4.349999999999940137, 2.500000000000000000, -6.941600689897078347 ) ) ;
#113926 = CARTESIAN_POINT ( 'NONE',  ( 1.449999999999952216, 12.50000000000000000, 1.883746621131358934 ) ) ;
#113927 = ORIENTED_EDGE ( 'NONE', *, *, #19659, .T. ) ;
#113928 = CARTESIAN_POINT ( 'NONE',  ( -9.150000000000009237, 12.50000000000000000, -2.857883832488653741 ) ) ;
#113929 = DIRECTION ( 'NONE',  ( 0.000000000000000000, 0.000000000000000000, -1.000000000000000000 ) ) ;
#113930 = CIRCLE ( 'NONE', #116062, 0.06509327318403745899 ) ;
#113931 = DIRECTION ( 'NONE',  ( 0.000000000000000000, 1.000000000000000000, 0.000000000000000000 ) ) ;
#113932 = VERTEX_POINT ( 'NONE', #13657 ) ;
#113933 = EDGE_CURVE ( 'NONE', #102898, #55074, #75172, .T. ) ;
#113934 = VERTEX_POINT ( 'NONE', #94163 ) ;
#113935 = VERTEX_POINT ( 'NONE', #115071 ) ;
#113936 = CARTESIAN_POINT ( 'NONE',  ( 9.799999999999917222, 12.50000000000000000, 0.4115034346978109769 ) ) ;
#113937 = CONICAL_SURFACE ( 'NONE', #19858, 0.1000000000000002554, 0.003490658503988666988 ) ;
#113938 = DIRECTION ( 'NONE',  ( 0.000000000000000000, 0.000000000000000000, 1.000000000000000000 ) ) ;
#113939 = CARTESIAN_POINT ( 'NONE',  ( 106.0514428414850272, 9.000000000000001776, -1.125000000000000222 ) ) ;
#113940 = CIRCLE ( 'NONE', #36590, 0.06509327318403745899 ) ;
#113941 = EDGE_LOOP ( 'NONE', ( #35000, #128292 ) ) ;
#113942 = DIRECTION ( 'NONE',  ( 0.000000000000000000, -0.9999939076577903929, 0.003490651415223739937 ) ) ;
#113943 = CARTESIAN_POINT ( 'NONE',  ( 7.949999999999925571, 2.500000000000000000, 2.165063509461097713 ) ) ;
#113944 = ADVANCED_FACE ( 'NONE', ( #33337 ), #124919, .F. ) ;
#113945 = DIRECTION ( 'NONE',  ( -0.000000000000000000, 1.000000000000000000, -0.000000000000000000 ) ) ;
#113946 = DIRECTION ( 'NONE',  ( 0.000000000000000000, 0.000000000000000000, -1.000000000000000000 ) ) ;
#113947 = VECTOR ( 'NONE', #55025, 1000.000000000000000 ) ;
#113948 = DIRECTION ( 'NONE',  ( 0.000000000000000000, 0.000000000000000000, -1.000000000000000000 ) ) ;
#113949 = CIRCLE ( 'NONE', #57520, 0.09999999999999982514 ) ;
#113950 = EDGE_LOOP ( 'NONE', ( #121569, #42452 ) ) ;
#113951 = ORIENTED_EDGE ( 'NONE', *, *, #75621, .T. ) ;
#113952 = DIRECTION ( 'NONE',  ( -4.274815082592931898E-19, -0.9999939076577903929, -0.003490651415223739937 ) ) ;
#113953 = DIRECTION ( 'NONE',  ( 0.000000000000000000, 1.000000000000000000, 0.000000000000000000 ) ) ;
#113954 = CARTESIAN_POINT ( 'NONE',  ( 3.149999999999946176, 2.500000000000000000, -1.818653347947325916 ) ) ;
#113955 = FACE_OUTER_BOUND ( 'NONE', #61780, .T. ) ;
#113956 = DIRECTION ( 'NONE',  ( -0.000000000000000000, -1.000000000000000000, -0.000000000000000000 ) ) ;
#113957 = ORIENTED_EDGE ( 'NONE', *, *, #17308, .T. ) ;
#113958 = CONICAL_SURFACE ( 'NONE', #53334, 0.09999999999999982514, 0.003490658503988666988 ) ;
#113959 = VECTOR ( 'NONE', #31743, 1000.000000000000000 ) ;
#113960 = EDGE_LOOP ( 'NONE', ( #58421, #42827 ) ) ;
#113961 = CARTESIAN_POINT ( 'NONE',  ( 3.749999999999942268, 2.500000000000000000, 1.472243186433545459 ) ) ;
#113962 = DIRECTION ( 'NONE',  ( 0.000000000000000000, -0.9999939076577903929, 0.003490651415223739937 ) ) ;
#113963 = CARTESIAN_POINT ( 'NONE',  ( 1.249999999999952038, 12.50000000000000000, -1.472243186433550122 ) ) ;
#113964 = CARTESIAN_POINT ( 'NONE',  ( 13.34999999999989662, 2.500000000000000000, -1.572243186433550211 ) ) ;
#113965 = EDGE_LOOP ( 'NONE', ( #124202, #121504 ) ) ;
#113966 = PLANE ( 'NONE',  #97048 ) ;
#113967 = ADVANCED_FACE ( 'NONE', ( #45081 ), #3848, .T. ) ;
#113968 = CARTESIAN_POINT ( 'NONE',  ( 179.5000000000000000, 1.375000000000000000, 7.634788798650556707 ) ) ;
#113969 = VERTEX_POINT ( 'NONE', #112531 ) ;
#113970 = FACE_OUTER_BOUND ( 'NONE', #22896, .T. ) ;
#113971 = CIRCLE ( 'NONE', #72226, 0.06509327318403745899 ) ;
#113972 = VERTEX_POINT ( 'NONE', #94812 ) ;
#113973 = EDGE_CURVE ( 'NONE', #68600, #125596, #121552, .T. ) ;
#113974 = CARTESIAN_POINT ( 'NONE',  ( -4.550000000000022915, 2.500000000000000000, 6.595190528383296780 ) ) ;
#113975 = CIRCLE ( 'NONE', #111923, 0.06509327318403745899 ) ;
#113976 = VERTEX_POINT ( 'NONE', #84980 ) ;
#113977 = DIRECTION ( 'NONE',  ( 0.000000000000000000, 0.000000000000000000, 1.000000000000000000 ) ) ;
#113978 = FACE_OUTER_BOUND ( 'NONE', #55726, .T. ) ;
#113979 = ADVANCED_FACE ( 'NONE', ( #83072 ), #17068, .T. ) ;
#113980 = CIRCLE ( 'NONE', #1104, 0.1000000000000000472 ) ;
#113981 = ORIENTED_EDGE ( 'NONE', *, *, #27423, .F. ) ;
#113982 = ADVANCED_FACE ( 'NONE', ( #63421 ), #31689, .T. ) ;
#113983 = ORIENTED_EDGE ( 'NONE', *, *, #72842, .F. ) ;
#113984 = EDGE_CURVE ( 'NONE', #102067, #14892, #871, .T. ) ;
#113985 = EDGE_CURVE ( 'NONE', #65870, #66105, #18174, .T. ) ;
#113986 = CARTESIAN_POINT ( 'NONE',  ( 187.0885416670080872, -6.551208109652273848, -3.782341765625003571 ) ) ;
#113987 = CARTESIAN_POINT ( 'NONE',  ( 12.89999999999990266, 12.50000000000000000, -3.702399969078687292 ) ) ;
#113988 = CARTESIAN_POINT ( 'NONE',  ( 184.7135416670080588, 4.367472073101518859, -7.564683531249999149 ) ) ;
#113989 = DIRECTION ( 'NONE',  ( 0.000000000000000000, 1.000000000000000000, 0.000000000000000000 ) ) ;
#113990 = VECTOR ( 'NONE', #113046, 1000.000000000000000 ) ;
#113991 = CIRCLE ( 'NONE', #91005, 0.1000000000000000472 ) ;
#113992 = FACE_OUTER_BOUND ( 'NONE', #47934, .T. ) ;
#113993 = DIRECTION ( 'NONE',  ( -0.000000000000000000, 1.000000000000000000, -0.000000000000000000 ) ) ;
#113994 = AXIS2_PLACEMENT_3D ( 'NONE', #27160, #36988, #87353 ) ;
#113995 = CARTESIAN_POINT ( 'NONE',  ( -3.350000000000031619, 2.500000000000000000, -5.802370205355749988 ) ) ;
#113996 = FACE_OUTER_BOUND ( 'NONE', #52364, .T. ) ;
#113997 = EDGE_CURVE ( 'NONE', #22231, #119031, #58879, .T. ) ;
#113998 = ADVANCED_FACE ( 'NONE', ( #109792 ), #119503, .T. ) ;
#113999 = CIRCLE ( 'NONE', #116048, 0.1000000000000002554 ) ;
#114000 = CIRCLE ( 'NONE', #86889, 0.06509327318403745899 ) ;
#114001 = EDGE_CURVE ( 'NONE', #15869, #23517, #46342, .T. ) ;
#114002 = ORIENTED_EDGE ( 'NONE', *, *, #77093, .T. ) ;
#114003 = VERTEX_POINT ( 'NONE', #11578 ) ;
#114004 = FACE_OUTER_BOUND ( 'NONE', #39160, .T. ) ;
#114005 = CARTESIAN_POINT ( 'NONE',  ( 3.749999999999944045, 2.500000000000000000, -7.188010851410854052 ) ) ;
#114006 = DIRECTION ( 'NONE',  ( 0.000000000000000000, 1.000000000000000000, 0.000000000000000000 ) ) ;
#114007 = AXIS2_PLACEMENT_3D ( 'NONE', #45347, #124549, #52102 ) ;
#114008 = DIRECTION ( 'NONE',  ( 0.000000000000000000, 0.000000000000000000, 1.000000000000000000 ) ) ;
#114010 = EDGE_LOOP ( 'NONE', ( #11488, #106767, #8074, #64930 ) ) ;
#114009 = ORIENTED_EDGE ( 'NONE', *, *, #44494, .T. ) ;
#114011 = CARTESIAN_POINT ( 'NONE',  ( 8.149999999999923972, 12.50000000000000000, -6.906693963081115051 ) ) ;
#114012 = ORIENTED_EDGE ( 'NONE', *, *, #39816, .T. ) ;
#114013 = CARTESIAN_POINT ( 'NONE',  ( 15.59999999999988951, 2.500000000000000000, -0.4464101615137783252 ) ) ;
#114014 = CARTESIAN_POINT ( 'NONE',  ( -3.350000000000028955, 2.500000000000000000, 2.165063509461097713 ) ) ;
#114015 = EDGE_LOOP ( 'NONE', ( #81735, #77708 ) ) ;
#114016 = CARTESIAN_POINT ( 'NONE',  ( -0.4000000000000396572, 12.50000000000000000, 3.637306695894644726 ) ) ;
#114017 = DIRECTION ( 'NONE',  ( 0.000000000000000000, -0.000000000000000000, 1.000000000000000000 ) ) ;
#114018 = DIRECTION ( 'NONE',  ( -0.000000000000000000, -1.000000000000000000, -0.000000000000000000 ) ) ;
#114019 = CARTESIAN_POINT ( 'NONE',  ( 2.499999999999948930, 12.50000000000000000, -0.7579135962115916003 ) ) ;
#114020 = CARTESIAN_POINT ( 'NONE',  ( -13.09999999999999254, 12.50000000000000000, -4.676537180435975216 ) ) ;
#114021 = DIRECTION ( 'NONE',  ( -0.000000000000000000, -1.000000000000000000, -0.000000000000000000 ) ) ;
#114022 = CARTESIAN_POINT ( 'NONE',  ( 187.1927083336747160, 6.551208109652275624, -3.782341765624998686 ) ) ;
#114023 = DIRECTION ( 'NONE',  ( 0.000000000000000000, 1.000000000000000000, 0.000000000000000000 ) ) ;
#114024 = AXIS2_PLACEMENT_3D ( 'NONE', #30146, #89052, #117841 ) ;
#114025 = CARTESIAN_POINT ( 'NONE',  ( -3.350000000000031619, 2.500000000000000000, -5.902370205355750521 ) ) ;
#114026 = ORIENTED_EDGE ( 'NONE', *, *, #70107, .F. ) ;
#114027 = ORIENTED_EDGE ( 'NONE', *, *, #16324, .F. ) ;
#114028 = ORIENTED_EDGE ( 'NONE', *, *, #47660, .F. ) ;
#114029 = PLANE ( 'NONE',  #109696 ) ;
#114030 = ORIENTED_EDGE ( 'NONE', *, *, #91763, .T. ) ;
#114032 = EDGE_LOOP ( 'NONE', ( #2918, #69764 ) ) ;
#114031 = VERTEX_POINT ( 'NONE', #128812 ) ;
#114033 = EDGE_LOOP ( 'NONE', ( #124601, #123600, #11549, #94041 ) ) ;
#114034 = CARTESIAN_POINT ( 'NONE',  ( 0.3999999999999563904, 12.50000000000000000, 5.088040615133786027 ) ) ;
#114035 = CONICAL_SURFACE ( 'NONE', #82744, 0.09999999999999982514, 0.003490658503988666988 ) ;
#114036 = AXIS2_PLACEMENT_3D ( 'NONE', #17363, #119439, #49448 ) ;
#114037 = FACE_OUTER_BOUND ( 'NONE', #116133, .T. ) ;
#114038 = DIRECTION ( 'NONE',  ( 0.000000000000000000, 0.000000000000000000, -1.000000000000000000 ) ) ;
#114039 = CARTESIAN_POINT ( 'NONE',  ( -1.050000000000037348, 12.50000000000000000, -6.906693963081115939 ) ) ;
#114040 = DIRECTION ( 'NONE',  ( -0.000000000000000000, -1.000000000000000000, -0.000000000000000000 ) ) ;
#114041 = EDGE_LOOP ( 'NONE', ( #36669, #117049, #18920, #98436 ) ) ;
#114042 = EDGE_CURVE ( 'NONE', #44898, #82776, #50651, .T. ) ;
#114043 = CARTESIAN_POINT ( 'NONE',  ( 15.39999999999989200, 2.500000000000000000, -0.6928203230275542523 ) ) ;
#114044 = ORIENTED_EDGE ( 'NONE', *, *, #41363, .F. ) ;
#114045 = VECTOR ( 'NONE', #8489, 1000.000000000000000 ) ;
#114046 = EDGE_CURVE ( 'NONE', #25459, #21997, #58973, .T. ) ;
#114047 = ORIENTED_EDGE ( 'NONE', *, *, #100123, .T. ) ;
#114048 = ORIENTED_EDGE ( 'NONE', *, *, #58717, .T. ) ;
#114050 = EDGE_CURVE ( 'NONE', #49778, #110877, #30602, .T. ) ;
#114049 = AXIS2_PLACEMENT_3D ( 'NONE', #82941, #109815, #60086 ) ;
#114051 = DIRECTION ( 'NONE',  ( -0.000000000000000000, 1.000000000000000000, -0.000000000000000000 ) ) ;
#114052 = VERTEX_POINT ( 'NONE', #22068 ) ;
#114053 = ORIENTED_EDGE ( 'NONE', *, *, #111124, .T. ) ;
#114054 = ORIENTED_EDGE ( 'NONE', *, *, #106888, .T. ) ;
#114055 = CARTESIAN_POINT ( 'NONE',  ( -8.550000000000011369, 12.50000000000000000, 1.818653347947321475 ) ) ;
#114056 = EDGE_CURVE ( 'NONE', #92222, #54959, #71802, .T. ) ;
#114057 = DIRECTION ( 'NONE',  ( 1.000000000000000000, -0.000000000000000000, -0.000000000000000000 ) ) ;
#114058 = CARTESIAN_POINT ( 'NONE',  ( -6.650000000000018119, 2.500000000000000000, -2.265063509461101798 ) ) ;
#114059 = CIRCLE ( 'NONE', #76405, 0.09999999999999982514 ) ;
#114060 = CARTESIAN_POINT ( 'NONE',  ( 4.149999999999941735, 2.500000000000000000, -1.372243186433550033 ) ) ;
#114061 = FACE_OUTER_BOUND ( 'NONE', #36135, .T. ) ;
#114062 = DIRECTION ( 'NONE',  ( 0.000000000000000000, 0.000000000000000000, 1.000000000000000000 ) ) ;
#114063 = CARTESIAN_POINT ( 'NONE',  ( 0.5999999999999612310, 2.500000000000000000, -0.3464101615137760715 ) ) ;
#114064 = EDGE_LOOP ( 'NONE', ( #119837, #83681 ) ) ;
#114065 = DIRECTION ( 'NONE',  ( 0.000000000000000000, 0.000000000000000000, 1.000000000000000000 ) ) ;
#114066 = VERTEX_POINT ( 'NONE', #118958 ) ;
#114067 = CARTESIAN_POINT ( 'NONE',  ( 186.0312500006828031, 9.429780353434619030E-16, -7.700000000000000178 ) ) ;
#114068 = ORIENTED_EDGE ( 'NONE', *, *, #10468, .F. ) ;
#114069 = EDGE_CURVE ( 'NONE', #56093, #58995, #88180, .T. ) ;
#114070 = EDGE_LOOP ( 'NONE', ( #15093, #45427, #109374, #59851 ) ) ;
#114071 = LINE ( 'NONE', #95077, #128533 ) ;
#114072 = CARTESIAN_POINT ( 'NONE',  ( 184.2760416670080588, 6.551208109652274736, 3.782341765625001351 ) ) ;
#114073 = VECTOR ( 'NONE', #68274, 1000.000000000000000 ) ;
#114074 = CARTESIAN_POINT ( 'NONE',  ( -14.39999999999998614, 12.50000000000000000, -0.3464101615137760715 ) ) ;
#114075 = ORIENTED_EDGE ( 'NONE', *, *, #38955, .T. ) ;
#114076 = DIRECTION ( 'NONE',  ( 0.000000000000000000, 0.000000000000000000, 1.000000000000000000 ) ) ;
#114077 = ORIENTED_EDGE ( 'NONE', *, *, #92465, .F. ) ;
#114078 = PLANE ( 'NONE',  #18492 ) ;
#114079 = CARTESIAN_POINT ( 'NONE',  ( 5.399999999999933742, 2.500000000000000000, -2.385244779468109755E-15 ) ) ;
#114080 = APPLICATION_CONTEXT ( 'automotive_design' ) ;
#114081 = CARTESIAN_POINT ( 'NONE',  ( -0.4000000000000392131, 12.50000000000000000, -4.330127018922201643 ) ) ;
#114082 = DIRECTION ( 'NONE',  ( -0.000000000000000000, 1.000000000000000000, -0.000000000000000000 ) ) ;
#114083 = AXIS2_PLACEMENT_3D ( 'NONE', #52399, #104083, #43247 ) ;
#114084 = DIRECTION ( 'NONE',  ( 0.000000000000000000, 1.000000000000000000, 0.000000000000000000 ) ) ;
#114085 = ORIENTED_EDGE ( 'NONE', *, *, #33624, .T. ) ;
#114086 = ADVANCED_FACE ( 'NONE', ( #121520 ), #6693, .T. ) ;
#114087 = AXIS2_PLACEMENT_3D ( 'NONE', #48751, #10717, #90587 ) ;
#114088 = EDGE_LOOP ( 'NONE', ( #63452, #21190, #98937, #88189 ) ) ;
#114089 = AXIS2_PLACEMENT_3D ( 'NONE', #50644, #49379, #89284 ) ;
#114090 = FACE_OUTER_BOUND ( 'NONE', #32759, .T. ) ;
#114092 = CONICAL_SURFACE ( 'NONE', #80649, 0.09999999999999982514, 0.003490658503988666988 ) ;
#114091 = CARTESIAN_POINT ( 'NONE',  ( 10.84999999999991260, 2.500000000000000000, 6.495190528383297135 ) ) ;
#114093 = VECTOR ( 'NONE', #59694, 1000.000000000000000 ) ;
#114094 = CARTESIAN_POINT ( 'NONE',  ( 185.8802083336747444, 4.367472073101515306, 7.564683531250000925 ) ) ;
#114095 = CARTESIAN_POINT ( 'NONE',  ( -5.200000000000022382, 2.500000000000000000, 4.676537180435972552 ) ) ;
#114096 = CARTESIAN_POINT ( 'NONE',  ( 2.499999999999945377, 12.50000000000000000, 5.088040615133786027 ) ) ;
#114097 = EDGE_CURVE ( 'NONE', #51506, #110134, #19239, .T. ) ;
#114098 = CARTESIAN_POINT ( 'NONE',  ( 10.84999999999990905, 2.500000000000000000, 2.265063509461097357 ) ) ;
#114099 = CARTESIAN_POINT ( 'NONE',  ( -0.6500000000000394351, 12.50000000000000000, 6.776507416713035248 ) ) ;
#114100 = VERTEX_POINT ( 'NONE', #120887 ) ;
#114101 = DIRECTION ( 'NONE',  ( 0.000000000000000000, 0.000000000000000000, 1.000000000000000000 ) ) ;
#114102 = CARTESIAN_POINT ( 'NONE',  ( -12.09999999999999432, 12.50000000000000000, 5.022947341949748790 ) ) ;
#114103 = CARTESIAN_POINT ( 'NONE',  ( 108.0000000000000142, 8.500000000000000000, -2.749999999999997335 ) ) ;
#114104 = VERTEX_POINT ( 'NONE', #100597 ) ;
#114105 = EDGE_CURVE ( 'NONE', #75943, #100949, #31784, .T. ) ;
#114106 = CIRCLE ( 'NONE', #89073, 4.000000000000000000 ) ;
#114107 = DIRECTION ( 'NONE',  ( -0.000000000000000000, -1.000000000000000000, -0.000000000000000000 ) ) ;
#114108 = ORIENTED_EDGE ( 'NONE', *, *, #96435, .F. ) ;
#114109 = DIRECTION ( 'NONE',  ( 0.000000000000000000, 0.000000000000000000, 1.000000000000000000 ) ) ;
#114110 = CIRCLE ( 'NONE', #82739, 0.06509327318403745899 ) ;
#114111 = ORIENTED_EDGE ( 'NONE', *, *, #13944, .T. ) ;
#114112 = FACE_OUTER_BOUND ( 'NONE', #112937, .T. ) ;
#114113 = CARTESIAN_POINT ( 'NONE',  ( 9.999999999999914735, 12.50000000000000000, 0.6277270498435120194 ) ) ;
#114114 = DIRECTION ( 'NONE',  ( -4.274815082592931898E-19, -0.9999939076577903929, -0.003490651415223739937 ) ) ;
#114115 = AXIS2_PLACEMENT_3D ( 'NONE', #127822, #118645, #98352 ) ;
#114116 = ORIENTED_EDGE ( 'NONE', *, *, #5101, .T. ) ;
#114117 = DIRECTION ( 'NONE',  ( -0.000000000000000000, 1.000000000000000000, -0.000000000000000000 ) ) ;
#114118 = CIRCLE ( 'NONE', #91133, 0.1000000000000002554 ) ;
#114119 = EDGE_CURVE ( 'NONE', #48486, #43713, #104910, .T. ) ;
#114120 = DIRECTION ( 'NONE',  ( 0.000000000000000000, -0.000000000000000000, 1.000000000000000000 ) ) ;
#114121 = ORIENTED_EDGE ( 'NONE', *, *, #25210, .T. ) ;
#114123 = CIRCLE ( 'NONE', #13860, 0.06509327318403745899 ) ;
#114122 = FACE_OUTER_BOUND ( 'NONE', #34069, .T. ) ;
#114124 = EDGE_CURVE ( 'NONE', #25500, #104198, #54836, .T. ) ;
#114125 = ORIENTED_EDGE ( 'NONE', *, *, #121524, .T. ) ;
#114127 = AXIS2_PLACEMENT_3D ( 'NONE', #21110, #61037, #37065 ) ;
#114126 = VECTOR ( 'NONE', #112591, 1000.000000000000000 ) ;
#114128 = VERTEX_POINT ( 'NONE', #129459 ) ;
#114129 = CARTESIAN_POINT ( 'NONE',  ( -7.050000000000013145, 2.500000000000000000, 6.495190528383297135 ) ) ;
#114130 = CARTESIAN_POINT ( 'NONE',  ( -1.650000000000034328, 12.50000000000000000, -2.922977105672691422 ) ) ;
#114131 = DIRECTION ( 'NONE',  ( -0.000000000000000000, 1.000000000000000000, -0.000000000000000000 ) ) ;
#114132 = ADVANCED_FACE ( 'NONE', ( #39780 ), #79677, .T. ) ;
#114133 = EDGE_CURVE ( 'NONE', #80090, #54834, #23455, .T. ) ;
#114134 = ORIENTED_EDGE ( 'NONE', *, *, #4595, .F. ) ;
#114135 = ADVANCED_FACE ( 'NONE', ( #1113 ), #41071, .T. ) ;
#114136 = ADVANCED_FACE ( 'NONE', ( #61335 ), #41707, .T. ) ;
#114137 = DIRECTION ( 'NONE',  ( -0.000000000000000000, 1.000000000000000000, -0.000000000000000000 ) ) ;
#114138 = PLANE ( 'NONE',  #92047 ) ;
#114139 = ORIENTED_EDGE ( 'NONE', *, *, #9216, .F. ) ;
#114140 = CARTESIAN_POINT ( 'NONE',  ( 11.64999999999990443, 2.500000000000000000, -7.088010851410853519 ) ) ;
#114141 = DIRECTION ( 'NONE',  ( 0.000000000000000000, 0.000000000000000000, -1.000000000000000000 ) ) ;
#114142 = AXIS2_PLACEMENT_3D ( 'NONE', #44628, #64257, #55729 ) ;
#114143 = EDGE_CURVE ( 'NONE', #104575, #128976, #94007, .T. ) ;
#114144 = CARTESIAN_POINT ( 'NONE',  ( 11.04999999999990656, 2.500000000000000000, -6.248780366869526759 ) ) ;
#114145 = CARTESIAN_POINT ( 'NONE',  ( -8.750000000000008882, 12.50000000000000000, -2.792790559304616504 ) ) ;
#114146 = CARTESIAN_POINT ( 'NONE',  ( 187.5000000000000000, 0.000000000000000000, 0.000000000000000000 ) ) ;
#114147 = ADVANCED_FACE ( 'NONE', ( #82268 ), #73081, .F. ) ;
#114148 = LINE ( 'NONE', #24477, #97387 ) ;
#114149 = DIRECTION ( 'NONE',  ( 0.000000000000000000, -0.9999939076577903929, 0.003490651415223739937 ) ) ;
#114150 = EDGE_CURVE ( 'NONE', #102205, #11990, #93371, .T. ) ;
#114151 = EDGE_CURVE ( 'NONE', #52643, #55268, #8771, .T. ) ;
#114152 = ADVANCED_FACE ( 'NONE', ( #82914 ), #115366, .T. ) ;
#114153 = VERTEX_POINT ( 'NONE', #94640 ) ;
#114154 = VERTEX_POINT ( 'NONE', #34464 ) ;
#114155 = ORIENTED_EDGE ( 'NONE', *, *, #53892, .T. ) ;
#114156 = ORIENTED_EDGE ( 'NONE', *, *, #34528, .T. ) ;
#114157 = CARTESIAN_POINT ( 'NONE',  ( -4.077824815344644402E-14, 2.500000000000000000, -5.122947341949753763 ) ) ;
#114158 = CARTESIAN_POINT ( 'NONE',  ( 6.899999999999928413, 2.500000000000000000, 3.883716857408421319 ) ) ;
#114159 = DIRECTION ( 'NONE',  ( 0.000000000000000000, 1.000000000000000000, 0.000000000000000000 ) ) ;
#114160 = ORIENTED_EDGE ( 'NONE', *, *, #85576, .T. ) ;
#114161 = EDGE_CURVE ( 'NONE', #12624, #55645, #107065, .T. ) ;
#114162 = FACE_BOUND ( 'NONE', #129569, .T. ) ;
#114163 = EDGE_CURVE ( 'NONE', #61624, #69063, #74370, .T. ) ;
#114164 = PLANE ( 'NONE',  #14515 ) ;
#114165 = PLANE ( 'NONE',  #77211 ) ;
#114166 = DIRECTION ( 'NONE',  ( 0.000000000000000000, 0.000000000000000000, 1.000000000000000000 ) ) ;
#114167 = AXIS2_PLACEMENT_3D ( 'NONE', #58337, #78624, #98879 ) ;
#114168 = CARTESIAN_POINT ( 'NONE',  ( -10.80000000000000071, 12.50000000000000000, 4.330127018922196314 ) ) ;
#114169 = AXIS2_PLACEMENT_3D ( 'NONE', #5246, #94931, #85739 ) ;
#114170 = DIRECTION ( 'NONE',  ( 0.000000000000000000, -0.9999939076577903929, 0.003490651415223739937 ) ) ;
#114171 = DIRECTION ( 'NONE',  ( -0.000000000000000000, -1.000000000000000000, -0.000000000000000000 ) ) ;
#114172 = DIRECTION ( 'NONE',  ( 0.000000000000000000, 0.000000000000000000, 1.000000000000000000 ) ) ;
#114173 = CARTESIAN_POINT ( 'NONE',  ( -1.250000000000036193, 2.500000000000000000, 1.472243186433545459 ) ) ;
#114174 = DIRECTION ( 'NONE',  ( 0.000000000000000000, 0.000000000000000000, 1.000000000000000000 ) ) ;
#114175 = CARTESIAN_POINT ( 'NONE',  ( 3.099999999999944134, 2.500000000000000000, 4.576537180435972019 ) ) ;
#114177 = CIRCLE ( 'NONE', #57751, 0.06509327318403745899 ) ;
#114176 = AXIS2_PLACEMENT_3D ( 'NONE', #95897, #105721, #124711 ) ;
#114178 = EDGE_LOOP ( 'NONE', ( #112847, #53786, #53351, #35161 ) ) ;
#114179 = EDGE_LOOP ( 'NONE', ( #65253, #127255, #71789, #53563 ) ) ;
#114180 = ORIENTED_EDGE ( 'NONE', *, *, #41295, .F. ) ;
#114181 = VERTEX_POINT ( 'NONE', #33178 ) ;
#114182 = ORIENTED_EDGE ( 'NONE', *, *, #109244, .T. ) ;
#114183 = CARTESIAN_POINT ( 'NONE',  ( -11.69999999999999929, 2.500000000000000000, -4.330127018922198978 ) ) ;
#114184 = ORIENTED_EDGE ( 'NONE', *, *, #105863, .T. ) ;
#114185 = VERTEX_POINT ( 'NONE', #104469 ) ;
#114187 = VECTOR ( 'NONE', #124434, 1000.000000000000000 ) ;
#114186 = AXIS2_PLACEMENT_3D ( 'NONE', #12640, #124552, #42791 ) ;
#114188 = CONICAL_SURFACE ( 'NONE', #64011, 0.1000000000000000056, 0.003490658503988666988 ) ;
#114189 = CARTESIAN_POINT ( 'NONE',  ( 13.34999999999990017, 12.50000000000000000, 1.407149913249508000 ) ) ;
#114190 = DIRECTION ( 'NONE',  ( 0.000000000000000000, -0.9999939076577903929, 0.003490651415223739937 ) ) ;
#114191 = CARTESIAN_POINT ( 'NONE',  ( -4.400000000000025224, 2.500000000000000000, 0.3464101615137735735 ) ) ;
#114192 = CARTESIAN_POINT ( 'NONE',  ( -5.450000000000019718, 12.50000000000000000, 2.165063509461097713 ) ) ;
#114193 = EDGE_LOOP ( 'NONE', ( #31840, #20106, #58822, #70460 ) ) ;
#114194 = EDGE_LOOP ( 'NONE', ( #129308, #7384 ) ) ;
#114195 = ADVANCED_FACE ( 'NONE', ( #23988 ), #65202, .T. ) ;
#114196 = EDGE_LOOP ( 'NONE', ( #72554, #38231, #104456, #54517 ) ) ;
#114198 = EDGE_LOOP ( 'NONE', ( #105361, #120710, #97543, #99957 ) ) ;
#114197 = DIRECTION ( 'NONE',  ( 0.000000000000000000, 0.000000000000000000, 1.000000000000000000 ) ) ;
#114199 = EDGE_CURVE ( 'NONE', #1969, #107840, #83559, .T. ) ;
#114200 = DIRECTION ( 'NONE',  ( -4.274815082592931898E-19, -0.9999939076577903929, -0.003490651415223739937 ) ) ;
#114201 = ORIENTED_EDGE ( 'NONE', *, *, #69863, .T. ) ;
#114202 = CIRCLE ( 'NONE', #70295, 0.09999999999999982514 ) ;
#114203 = VERTEX_POINT ( 'NONE', #114290 ) ;
#114204 = DIRECTION ( 'NONE',  ( -0.000000000000000000, 1.000000000000000000, -0.000000000000000000 ) ) ;
#114205 = EDGE_CURVE ( 'NONE', #29149, #19578, #38129, .T. ) ;
#114206 = DIRECTION ( 'NONE',  ( 0.000000000000000000, 1.000000000000000000, 0.000000000000000000 ) ) ;
#114207 = DIRECTION ( 'NONE',  ( 0.000000000000000000, 0.000000000000000000, 1.000000000000000000 ) ) ;
#114208 = AXIS2_PLACEMENT_3D ( 'NONE', #124689, #54634, #42930 ) ;
#114209 = FACE_OUTER_BOUND ( 'NONE', #51837, .T. ) ;
#114210 = DIRECTION ( 'NONE',  ( 0.000000000000000000, 1.000000000000000000, 0.000000000000000000 ) ) ;
#114211 = CIRCLE ( 'NONE', #74498, 0.09999999999999982514 ) ;
#114212 = CONICAL_SURFACE ( 'NONE', #9750, 0.09999999999999982514, 0.003490658503988666988 ) ;
#114213 = ADVANCED_FACE ( 'NONE', ( #122194 ), #42251, .T. ) ;
#114214 = ORIENTED_EDGE ( 'NONE', *, *, #68001, .F. ) ;
#114216 = AXIS2_PLACEMENT_3D ( 'NONE', #89194, #7393, #27056 ) ;
#114215 = LINE ( 'NONE', #76231, #69991 ) ;
#114217 = ORIENTED_EDGE ( 'NONE', *, *, #94645, .F. ) ;
#114218 = CARTESIAN_POINT ( 'NONE',  ( 87.50000000000002842, 6.099025433955697295, 4.412011999987998756 ) ) ;
#114219 = VERTEX_POINT ( 'NONE', #44921 ) ;
#114220 = DIRECTION ( 'NONE',  ( -0.000000000000000000, 1.000000000000000000, -0.000000000000000000 ) ) ;
#114221 = CARTESIAN_POINT ( 'NONE',  ( 8.949999999999917577, 2.500000000000000000, -2.411473670974877859 ) ) ;
#114222 = DIRECTION ( 'NONE',  ( 0.000000000000000000, 1.000000000000000000, 0.000000000000000000 ) ) ;
#114223 = CARTESIAN_POINT ( 'NONE',  ( 8.549999999999922551, 12.50000000000000000, 2.511473670974873507 ) ) ;
#114224 = VERTEX_POINT ( 'NONE', #53455 ) ;
#114225 = AXIS2_PLACEMENT_3D ( 'NONE', #67587, #118628, #87227 ) ;
#114226 = PLANE ( 'NONE',  #785 ) ;
#114228 = VECTOR ( 'NONE', #124479, 1000.000000000000000 ) ;
#114227 = VECTOR ( 'NONE', #104671, 1000.000000000000000 ) ;
#114229 = DIRECTION ( 'NONE',  ( 0.000000000000000000, 0.000000000000000000, 1.000000000000000000 ) ) ;
#114230 = ORIENTED_EDGE ( 'NONE', *, *, #45358, .F. ) ;
#114231 = VERTEX_POINT ( 'NONE', #75020 ) ;
#114232 = VERTEX_POINT ( 'NONE', #114924 ) ;
#114233 = CARTESIAN_POINT ( 'NONE',  ( 4.199999999999938005, 12.50000000000000000, 4.330127018922196314 ) ) ;
#114234 = PLANE ( 'NONE',  #59654 ) ;
#114235 = CARTESIAN_POINT ( 'NONE',  ( 186.6510416670080303, 4.367472073101518859, -7.564683531249999149 ) ) ;
#114236 = DIRECTION ( 'NONE',  ( -0.000000000000000000, 1.000000000000000000, -0.000000000000000000 ) ) ;
#114237 = ADVANCED_FACE ( 'NONE', ( #3692 ), #92402, .T. ) ;
#114238 = CARTESIAN_POINT ( 'NONE',  ( 17.45652598566545066, 2.453228361101884580, -4.494719241542722621 ) ) ;
#114239 = CARTESIAN_POINT ( 'NONE',  ( -0.4500000000000402012, 2.500000000000000000, 6.495190528383297135 ) ) ;
#114240 = VERTEX_POINT ( 'NONE', #25248 ) ;
#114241 = FACE_OUTER_BOUND ( 'NONE', #43045, .T. ) ;
#114242 = ORIENTED_EDGE ( 'NONE', *, *, #123011, .T. ) ;
#114243 = EDGE_CURVE ( 'NONE', #121831, #2267, #71472, .T. ) ;
#114244 = DIRECTION ( 'NONE',  ( 0.000000000000000000, 0.000000000000000000, 1.000000000000000000 ) ) ;
#114245 = CARTESIAN_POINT ( 'NONE',  ( -5.200000000000020606, 2.500000000000000000, -0.2464101615137782308 ) ) ;
#114246 = CARTESIAN_POINT ( 'NONE',  ( 3.349999999999945466, 2.500000000000000000, -7.288010851410854585 ) ) ;
#114247 = VERTEX_POINT ( 'NONE', #32539 ) ;
#114248 = CIRCLE ( 'NONE', #22329, 0.06509327318403745899 ) ;
#114249 = AXIS2_PLACEMENT_3D ( 'NONE', #47128, #78535, #19591 ) ;
#114250 = DIRECTION ( 'NONE',  ( 0.000000000000000000, 0.000000000000000000, 1.000000000000000000 ) ) ;
#114251 = DIRECTION ( 'NONE',  ( 0.000000000000000000, 1.000000000000000000, 0.000000000000000000 ) ) ;
#114252 = EDGE_CURVE ( 'NONE', #80635, #20888, #113332, .T. ) ;
#114253 = ORIENTED_EDGE ( 'NONE', *, *, #10324, .T. ) ;
#114255 = CONICAL_SURFACE ( 'NONE', #57841, 0.1000000000000002554, 0.003490658503988666988 ) ;
#114254 = VECTOR ( 'NONE', #110077, 1000.000000000000000 ) ;
#114256 = DIRECTION ( 'NONE',  ( 0.000000000000000000, 1.000000000000000000, 0.000000000000000000 ) ) ;
#114257 = ORIENTED_EDGE ( 'NONE', *, *, #2365, .T. ) ;
#114258 = EDGE_LOOP ( 'NONE', ( #119886, #19826, #12809, #98257 ) ) ;
#114259 = CARTESIAN_POINT ( 'NONE',  ( 6.249999999999930722, 2.500000000000000000, 7.288010851410849256 ) ) ;
#114260 = ORIENTED_EDGE ( 'NONE', *, *, #75437, .T. ) ;
#114261 = CARTESIAN_POINT ( 'NONE',  ( 16.79927703354236357, 2.472530191752521311, -3.248144252803072618 ) ) ;
#114262 = PLANE ( 'NONE',  #119552 ) ;
#114263 = CONICAL_SURFACE ( 'NONE', #74558, 0.1000000000000002554, 0.003490658503988666988 ) ;
#114264 = DIRECTION ( 'NONE',  ( 0.000000000000000000, 0.000000000000000000, 1.000000000000000000 ) ) ;
#114265 = VERTEX_POINT ( 'NONE', #73711 ) ;
#114266 = CONICAL_SURFACE ( 'NONE', #68201, 0.1000000000000002554, 0.003490658503988666988 ) ;
#114267 = DIRECTION ( 'NONE',  ( 0.000000000000000000, 1.000000000000000000, 0.000000000000000000 ) ) ;
#114269 = EDGE_LOOP ( 'NONE', ( #89582, #32668, #104131, #72569 ) ) ;
#114268 = LINE ( 'NONE', #27178, #16528 ) ;
#114270 = LINE ( 'NONE', #64523, #117561 ) ;
#114271 = DIRECTION ( 'NONE',  ( -0.000000000000000000, -1.000000000000000000, -0.000000000000000000 ) ) ;
#114272 = ORIENTED_EDGE ( 'NONE', *, *, #56174, .F. ) ;
#114273 = EDGE_CURVE ( 'NONE', #108629, #13143, #100804, .T. ) ;
#114274 = ORIENTED_EDGE ( 'NONE', *, *, #114881, .T. ) ;
#114275 = EDGE_LOOP ( 'NONE', ( #8005, #106523 ) ) ;
#114276 = LINE ( 'NONE', #16057, #104703 ) ;
#114277 = PLANE ( 'NONE',  #118921 ) ;
#114278 = CARTESIAN_POINT ( 'NONE',  ( 5.649999999999932854, 12.50000000000000000, 2.511473670974873507 ) ) ;
#114279 = EDGE_CURVE ( 'NONE', #88674, #117051, #35984, .T. ) ;
#114280 = FACE_BOUND ( 'NONE', #101187, .T. ) ;
#114281 = EDGE_LOOP ( 'NONE', ( #12836, #95776, #56463, #28488 ) ) ;
#114282 = CONICAL_SURFACE ( 'NONE', #39098, 0.1000000000000002554, 0.003490658503988666988 ) ;
#114283 = CARTESIAN_POINT ( 'NONE',  ( 186.2343750003414016, 8.734944146203032389, 5.348610694689227483E-16 ) ) ;
#114284 = EDGE_CURVE ( 'NONE', #7581, #109083, #115561, .T. ) ;
#114285 = DIRECTION ( 'NONE',  ( 0.000000000000000000, -0.000000000000000000, 1.000000000000000000 ) ) ;
#114286 = DIRECTION ( 'NONE',  ( 0.000000000000000000, 0.000000000000000000, 1.000000000000000000 ) ) ;
#114287 = VECTOR ( 'NONE', #97105, 1000.000000000000000 ) ;
#114288 = DIRECTION ( 'NONE',  ( 0.000000000000000000, 0.000000000000000000, 1.000000000000000000 ) ) ;
#114289 = ADVANCED_FACE ( 'NONE', ( #126701 ), #117510, .T. ) ;
#114290 = CARTESIAN_POINT ( 'NONE',  ( -0.8500000000000386136, 12.50000000000000000, 7.253104124594885960 ) ) ;
#114291 = ADVANCED_FACE ( 'NONE', ( #76310 ), #10904, .T. ) ;
#114292 = DIRECTION ( 'NONE',  ( 0.000000000000000000, -0.000000000000000000, 1.000000000000000000 ) ) ;
#114293 = ADVANCED_FACE ( 'NONE', ( #117483 ), #34018, .T. ) ;
#114294 = DIRECTION ( 'NONE',  ( 0.000000000000000000, 0.000000000000000000, 1.000000000000000000 ) ) ;
#114295 = AXIS2_PLACEMENT_3D ( 'NONE', #37840, #127519, #4646 ) ;
#114296 = DIRECTION ( 'NONE',  ( 0.000000000000000000, 0.000000000000000000, 1.000000000000000000 ) ) ;
#114297 = AXIS2_PLACEMENT_3D ( 'NONE', #60350, #111337, #100262 ) ;
#114298 = EDGE_CURVE ( 'NONE', #100751, #84404, #5607, .T. ) ;
#114299 = ORIENTED_EDGE ( 'NONE', *, *, #97027, .T. ) ;
#114300 = VERTEX_POINT ( 'NONE', #56638 ) ;
#114301 = EDGE_LOOP ( 'NONE', ( #98980, #41342, #64678, #117891 ) ) ;
#114302 = ORIENTED_EDGE ( 'NONE', *, *, #113877, .F. ) ;
#114303 = EDGE_LOOP ( 'NONE', ( #121345, #55741, #39048, #75090 ) ) ;
#114304 = CARTESIAN_POINT ( 'NONE',  ( 6.449999999999930012, 2.500000000000000000, 6.941600689897073018 ) ) ;
#114305 = CARTESIAN_POINT ( 'NONE',  ( 5.799999999999933209, 2.500000000000000000, 0.09999999999999761857 ) ) ;
#114306 = VECTOR ( 'NONE', #35319, 1000.000000000000000 ) ;
#114307 = ORIENTED_EDGE ( 'NONE', *, *, #46154, .F. ) ;
#114308 = FACE_BOUND ( 'NONE', #104572, .T. ) ;
#114309 = EDGE_CURVE ( 'NONE', #102404, #105289, #38235, .T. ) ;
#114311 = DIRECTION ( 'NONE',  ( 0.000000000000000000, -0.000000000000000000, 1.000000000000000000 ) ) ;
#114310 = AXIS2_PLACEMENT_3D ( 'NONE', #94984, #64223, #5292 ) ;
#114313 = VECTOR ( 'NONE', #128355, 1000.000000000000000 ) ;
#114312 = AXIS2_PLACEMENT_3D ( 'NONE', #90696, #80889, #41621 ) ;
#114314 = CARTESIAN_POINT ( 'NONE',  ( 6.049999999999932321, 2.500000000000000000, 6.841600689897072485 ) ) ;
#114315 = VERTEX_POINT ( 'NONE', #105105 ) ;
#114316 = DIRECTION ( 'NONE',  ( -4.274815082592931898E-19, -0.9999939076577903929, -0.003490651415223739937 ) ) ;
#114317 = CARTESIAN_POINT ( 'NONE',  ( -13.74999999999998757, 2.500000000000000000, -2.957883832488651610 ) ) ;
#114318 = CARTESIAN_POINT ( 'NONE',  ( -6.450000000000017941, 12.50000000000000000, -6.776507416713039689 ) ) ;
#114319 = EDGE_LOOP ( 'NONE', ( #40816, #41543 ) ) ;
#114320 = DIRECTION ( 'NONE',  ( 0.000000000000000000, -0.000000000000000000, 1.000000000000000000 ) ) ;
#114321 = ORIENTED_EDGE ( 'NONE', *, *, #44394, .F. ) ;
#114322 = VERTEX_POINT ( 'NONE', #57314 ) ;
#114323 = VERTEX_POINT ( 'NONE', #67769 ) ;
#114324 = DIRECTION ( 'NONE',  ( -0.000000000000000000, -1.000000000000000000, -0.000000000000000000 ) ) ;
#114325 = CARTESIAN_POINT ( 'NONE',  ( 3.549999999999941203, 12.50000000000000000, 6.148780366869520897 ) ) ;
#114326 = CARTESIAN_POINT ( 'NONE',  ( 14.14999999999989377, 2.500000000000000000, -1.372243186433550033 ) ) ;
#114327 = ORIENTED_EDGE ( 'NONE', *, *, #115408, .T. ) ;
#114328 = CARTESIAN_POINT ( 'NONE',  ( -9.150000000000009237, 12.50000000000000000, -2.165063509461101710 ) ) ;
#114329 = CARTESIAN_POINT ( 'NONE',  ( 0.8499999999999527933, 12.50000000000000000, 7.188010851410848723 ) ) ;
#114330 = DIRECTION ( 'NONE',  ( 0.000000000000000000, 0.000000000000000000, 1.000000000000000000 ) ) ;
#114331 = FACE_OUTER_BOUND ( 'NONE', #27586, .T. ) ;
#114333 = EDGE_LOOP ( 'NONE', ( #69121, #127632 ) ) ;
#114332 = CARTESIAN_POINT ( 'NONE',  ( 1.249999999999953815, 2.500000000000000000, -2.857883832488653741 ) ) ;
#114334 = DIRECTION ( 'NONE',  ( 0.000000000000000000, 1.000000000000000000, 0.000000000000000000 ) ) ;
#114335 = EDGE_LOOP ( 'NONE', ( #124095, #28547, #77403, #18544 ) ) ;
#114336 = DIRECTION ( 'NONE',  ( 0.000000000000000000, 1.000000000000000000, 0.000000000000000000 ) ) ;
#114337 = ORIENTED_EDGE ( 'NONE', *, *, #14407, .F. ) ;
#114338 = EDGE_CURVE ( 'NONE', #2220, #41822, #25921, .T. ) ;
#114339 = ORIENTED_EDGE ( 'NONE', *, *, #81555, .T. ) ;
#114340 = CARTESIAN_POINT ( 'NONE',  ( 5.649999999999934630, 12.50000000000000000, 6.841600689897072485 ) ) ;
#114341 = CARTESIAN_POINT ( 'NONE',  ( 2.099999999999949463, 2.500000000000000000, 0.6928203230275494784 ) ) ;
#114342 = CARTESIAN_POINT ( 'NONE',  ( 12.09999999999990550, 2.500000000000000000, 3.637306695894644726 ) ) ;
#114343 = DIRECTION ( 'NONE',  ( 0.000000000000000000, 1.000000000000000000, 0.000000000000000000 ) ) ;
#114344 = CARTESIAN_POINT ( 'NONE',  ( -7.100000000000018296, 2.500000000000000000, -2.385244779468109755E-15 ) ) ;
#114345 = EDGE_LOOP ( 'NONE', ( #50912, #81352, #87951, #63208 ) ) ;
#114348 = EDGE_LOOP ( 'NONE', ( #26358, #74345, #81218, #33808 ) ) ;
#114347 = AXIS2_PLACEMENT_3D ( 'NONE', #102857, #31565, #102241 ) ;
#114346 = CIRCLE ( 'NONE', #7729, 0.09999999999999982514 ) ;
#114349 = ADVANCED_FACE ( 'NONE', ( #126035 ), #116214, .T. ) ;
#114350 = CARTESIAN_POINT ( 'NONE',  ( 10.79999999999991012, 12.50000000000000000, -4.330127018922201643 ) ) ;
#114351 = DIRECTION ( 'NONE',  ( 0.000000000000000000, 0.000000000000000000, 1.000000000000000000 ) ) ;
#114352 = DIRECTION ( 'NONE',  ( 0.000000000000000000, 0.000000000000000000, 1.000000000000000000 ) ) ;
#114353 = ORIENTED_EDGE ( 'NONE', *, *, #44883, .F. ) ;
#114354 = ORIENTED_EDGE ( 'NONE', *, *, #49296, .F. ) ;
#114355 = CARTESIAN_POINT ( 'NONE',  ( 10.59999999999991260, 2.500000000000000000, -0.4464101615137783252 ) ) ;
#114356 = VECTOR ( 'NONE', #66147, 1000.000000000000000 ) ;
#114357 = EDGE_LOOP ( 'NONE', ( #121703, #20314, #103756, #125623 ) ) ;
#114358 = DIRECTION ( 'NONE',  ( 0.000000000000000000, 0.000000000000000000, -1.000000000000000000 ) ) ;
#114359 = CONICAL_SURFACE ( 'NONE', #74649, 0.1000000000000002554, 0.003490658503988666988 ) ;
#114360 = DIRECTION ( 'NONE',  ( 0.000000000000000000, -0.000000000000000000, 1.000000000000000000 ) ) ;
#114361 = EDGE_LOOP ( 'NONE', ( #96970, #58207, #114781, #24885 ) ) ;
#114362 = CARTESIAN_POINT ( 'NONE',  ( 7.299999999999927880, 2.500000000000000000, 4.083716857408421497 ) ) ;
#114363 = DIRECTION ( 'NONE',  ( -0.000000000000000000, -1.000000000000000000, -0.000000000000000000 ) ) ;
#114364 = CARTESIAN_POINT ( 'NONE',  ( 15.39999999999989022, 2.500000000000000000, -2.385244779468109755E-15 ) ) ;
#114365 = DIRECTION ( 'NONE',  ( 0.000000000000000000, 1.000000000000000000, 0.000000000000000000 ) ) ;
#114366 = ORIENTED_EDGE ( 'NONE', *, *, #78837, .T. ) ;
#114367 = DIRECTION ( 'NONE',  ( 0.000000000000000000, 0.000000000000000000, 1.000000000000000000 ) ) ;
#114368 = CARTESIAN_POINT ( 'NONE',  ( 81.97620568556726539, -3.937821662896079378, 6.124242991616513976 ) ) ;
#114369 = ORIENTED_EDGE ( 'NONE', *, *, #115850, .F. ) ;
#114370 = ORIENTED_EDGE ( 'NONE', *, *, #98418, .T. ) ;
#114371 = CARTESIAN_POINT ( 'NONE',  ( 184.1302083336747160, -4.367472073101514418, -7.564683531250002702 ) ) ;
#114372 = DIRECTION ( 'NONE',  ( 0.000000000000000000, 0.000000000000000000, -1.000000000000000000 ) ) ;
#114373 = CARTESIAN_POINT ( 'NONE',  ( 6.849999999999929479, 12.50000000000000000, -2.511473670974877948 ) ) ;
#114374 = AXIS2_PLACEMENT_3D ( 'NONE', #103398, #31441, #53645 ) ;
#114375 = LINE ( 'NONE', #27283, #13431 ) ;
#114376 = CARTESIAN_POINT ( 'NONE',  ( -5.650000000000023448, 2.500000000000000000, -1.918653347947326004 ) ) ;
#114377 = ADVANCED_FACE ( 'NONE', ( #7549 ), #87396, .T. ) ;
#114378 = DIRECTION ( 'NONE',  ( 0.000000000000000000, 0.000000000000000000, 1.000000000000000000 ) ) ;
#114379 = CARTESIAN_POINT ( 'NONE',  ( 10.64999999999990976, 2.500000000000000000, 2.511473670974873507 ) ) ;
#114380 = CARTESIAN_POINT ( 'NONE',  ( -4.350000000000023626, 12.50000000000000000, 6.213873640053559022 ) ) ;
#114381 = DIRECTION ( 'NONE',  ( 0.000000000000000000, 0.000000000000000000, 1.000000000000000000 ) ) ;
#114382 = AXIS2_PLACEMENT_3D ( 'NONE', #20642, #60578, #128685 ) ;
#114383 = FACE_OUTER_BOUND ( 'NONE', #32986, .T. ) ;
#114384 = ADVANCED_FACE ( 'NONE', ( #116858 ), #119686, .T. ) ;
#114385 = VERTEX_POINT ( 'NONE', #95943 ) ;
#114386 = VERTEX_POINT ( 'NONE', #106403 ) ;
#114387 = CIRCLE ( 'NONE', #64215, 0.1000000000000000472 ) ;
#114388 = ORIENTED_EDGE ( 'NONE', *, *, #10553, .T. ) ;
#114389 = EDGE_CURVE ( 'NONE', #11701, #55594, #65827, .T. ) ;
#114390 = VERTEX_POINT ( 'NONE', #37031 ) ;
#114391 = CONICAL_SURFACE ( 'NONE', #18253, 0.1000000000000002554, 0.003490658503988666988 ) ;
#114392 = CARTESIAN_POINT ( 'NONE',  ( 15.39999999999989022, 12.50000000000000000, -2.385244779468109755E-15 ) ) ;
#114393 = EDGE_CURVE ( 'NONE', #79899, #114770, #127351, .T. ) ;
#114394 = DIRECTION ( 'NONE',  ( 0.000000000000000000, 0.000000000000000000, 1.000000000000000000 ) ) ;
#114395 = LINE ( 'NONE', #14877, #58401 ) ;
#114396 = EDGE_LOOP ( 'NONE', ( #60788, #43435 ) ) ;
#114397 = FACE_OUTER_BOUND ( 'NONE', #54596, .T. ) ;
#114399 = CIRCLE ( 'NONE', #118606, 0.06509327318403745899 ) ;
#114398 = CIRCLE ( 'NONE', #57982, 0.1000000000000000472 ) ;
#114400 = ADVANCED_FACE ( 'NONE', ( #77576 ), #31873, .T. ) ;
#114401 = CARTESIAN_POINT ( 'NONE',  ( 2.699999999999946443, 12.50000000000000000, -3.983716857408426293 ) ) ;
#114403 = VERTEX_POINT ( 'NONE', #48141 ) ;
#114402 = DIRECTION ( 'NONE',  ( 0.000000000000000000, 1.000000000000000000, 0.000000000000000000 ) ) ;
#114404 = EDGE_CURVE ( 'NONE', #104514, #127159, #111353, .T. ) ;
#114405 = FACE_OUTER_BOUND ( 'NONE', #109142, .T. ) ;
#114406 = CARTESIAN_POINT ( 'NONE',  ( 11.84999999999990372, 2.500000000000000000, 2.511473670974873507 ) ) ;
#114407 = ORIENTED_EDGE ( 'NONE', *, *, #5193, .T. ) ;
#114408 = ORIENTED_EDGE ( 'NONE', *, *, #83348, .F. ) ;
#114409 = EDGE_LOOP ( 'NONE', ( #14110, #110157, #13604, #20672 ) ) ;
#114410 = ORIENTED_EDGE ( 'NONE', *, *, #40074, .T. ) ;
#114411 = DIRECTION ( 'NONE',  ( -1.000000000000000000, -0.000000000000000000, -0.000000000000000000 ) ) ;
#114412 = AXIS2_PLACEMENT_3D ( 'NONE', #109013, #79579, #78945 ) ;
#114413 = LINE ( 'NONE', #34599, #59302 ) ;
#114414 = CARTESIAN_POINT ( 'NONE',  ( 0.3999999999999619971, 2.500000000000000000, -1.084202172485504434E-16 ) ) ;
#114415 = DIRECTION ( 'NONE',  ( 0.000000000000000000, 0.000000000000000000, -1.000000000000000000 ) ) ;
#114416 = ORIENTED_EDGE ( 'NONE', *, *, #90134, .F. ) ;
#114417 = EDGE_CURVE ( 'NONE', #23243, #52693, #15208, .T. ) ;
#114418 = FACE_OUTER_BOUND ( 'NONE', #67906, .T. ) ;
#114419 = EDGE_LOOP ( 'NONE', ( #74386, #79078, #121454, #28636 ) ) ;
#114420 = DIRECTION ( 'NONE',  ( -0.000000000000000000, 1.000000000000000000, -0.000000000000000000 ) ) ;
#114421 = CARTESIAN_POINT ( 'NONE',  ( 2.499999999999948930, 2.500000000000000000, -0.6928203230275541413 ) ) ;
#114422 = DIRECTION ( 'NONE',  ( 0.000000000000000000, 1.000000000000000000, 0.000000000000000000 ) ) ;
#114423 = DIRECTION ( 'NONE',  ( 0.000000000000000000, -0.9999939076577903929, 0.003490651415223739937 ) ) ;
#114424 = ORIENTED_EDGE ( 'NONE', *, *, #125825, .T. ) ;
#114425 = AXIS2_PLACEMENT_3D ( 'NONE', #30347, #127247, #59154 ) ;
#114426 = EDGE_CURVE ( 'NONE', #13310, #129065, #123888, .T. ) ;
#114427 = VERTEX_POINT ( 'NONE', #51377 ) ;
#114428 = ORIENTED_EDGE ( 'NONE', *, *, #62279, .F. ) ;
#114429 = CARTESIAN_POINT ( 'NONE',  ( -0.2000000000000404232, 2.500000000000000000, 3.883716857408421319 ) ) ;
#114430 = DIRECTION ( 'NONE',  ( -0.000000000000000000, -1.000000000000000000, -0.000000000000000000 ) ) ;
#114431 = DIRECTION ( 'NONE',  ( -0.000000000000000000, 1.000000000000000000, -0.000000000000000000 ) ) ;
#114432 = FACE_BOUND ( 'NONE', #16761, .T. ) ;
#114433 = DIRECTION ( 'NONE',  ( 0.000000000000000000, 0.000000000000000000, 1.000000000000000000 ) ) ;
#114434 = FACE_OUTER_BOUND ( 'NONE', #103030, .T. ) ;
#114437 = ADVANCED_FACE ( 'NONE', ( #961 ), #105011, .T. ) ;
#114436 = CIRCLE ( 'NONE', #81000, 0.1000000000000000472 ) ;
#114435 = CIRCLE ( 'NONE', #58023, 0.1000000000000002554 ) ;
#114438 = DIRECTION ( 'NONE',  ( 0.000000000000000000, 0.000000000000000000, -1.000000000000000000 ) ) ;
#114439 = VECTOR ( 'NONE', #34200, 1000.000000000000000 ) ;
#114440 = ADVANCED_FACE ( 'NONE', ( #128661 ), #40286, .T. ) ;
#114441 = CARTESIAN_POINT ( 'NONE',  ( 186.8802083336747444, 4.367472073101515306, 7.564683531250000925 ) ) ;
#114442 = CARTESIAN_POINT ( 'NONE',  ( -10.65000000000000213, 12.50000000000000000, 2.511473670974873507 ) ) ;
#114443 = ADVANCED_FACE ( 'NONE', ( #91279 ), #113437, .T. ) ;
#114444 = DIRECTION ( 'NONE',  ( 1.000000000000000000, 0.000000000000000000, 0.000000000000000000 ) ) ;
#114445 = EDGE_LOOP ( 'NONE', ( #84131, #72148 ) ) ;
#114447 = EDGE_CURVE ( 'NONE', #41701, #35924, #40257, .T. ) ;
#114446 = CONICAL_SURFACE ( 'NONE', #126979, 0.1000000000000002554, 0.003490658503988666988 ) ;
#114448 = CIRCLE ( 'NONE', #110251, 0.06509327318403745899 ) ;
#114449 = DIRECTION ( 'NONE',  ( -0.000000000000000000, -1.000000000000000000, -0.000000000000000000 ) ) ;
#114450 = EDGE_CURVE ( 'NONE', #34926, #120592, #20614, .T. ) ;
#114451 = EDGE_LOOP ( 'NONE', ( #9995, #13472, #4422, #20053 ) ) ;
#114452 = EDGE_LOOP ( 'NONE', ( #109379, #110431 ) ) ;
#114453 = ORIENTED_EDGE ( 'NONE', *, *, #114273, .T. ) ;
#114454 = VERTEX_POINT ( 'NONE', #39635 ) ;
#114455 = CARTESIAN_POINT ( 'NONE',  ( -8.150000000000012790, 12.50000000000000000, 1.818653347947321475 ) ) ;
#114456 = FACE_BOUND ( 'NONE', #2374, .T. ) ;
#114457 = CARTESIAN_POINT ( 'NONE',  ( -13.29999999999999005, 2.500000000000000000, -0.09999999999999815981 ) ) ;
#114458 = ADVANCED_FACE ( 'NONE', ( #8836 ), #50746, .T. ) ;
#114459 = AXIS2_PLACEMENT_3D ( 'NONE', #9315, #49260, #81912 ) ;
#114460 = EDGE_CURVE ( 'NONE', #73591, #107817, #65297, .T. ) ;
#114461 = AXIS2_PLACEMENT_3D ( 'NONE', #67454, #9206, #87754 ) ;
#114462 = VERTEX_POINT ( 'NONE', #69054 ) ;
#114463 = UNCERTAINTY_MEASURE_WITH_UNIT (LENGTH_MEASURE( 1.000000000000000082E-05 ), #80562, 'distance_accuracy_value', 'NONE');
#114464 = CARTESIAN_POINT ( 'NONE',  ( 65.40763333621140418, 3.109051995140788005, 5.794606894440900824 ) ) ;
#114465 = DIRECTION ( 'NONE',  ( 0.000000000000000000, -0.9999939076577903929, 0.003490651415223739937 ) ) ;
#114466 = CIRCLE ( 'NONE', #9923, 0.06509327318403745899 ) ;
#114467 = VERTEX_POINT ( 'NONE', #69707 ) ;
#114468 = CARTESIAN_POINT ( 'NONE',  ( 2.499999999999947153, 2.500000000000000000, 0.7928203230275495672 ) ) ;
#114469 = CONICAL_SURFACE ( 'NONE', #45530, 0.1000000000000000472, 0.003490658503988666988 ) ;
#114470 = CARTESIAN_POINT ( 'NONE',  ( -14.34999999999998543, 2.500000000000000000, -1.718653347947323606 ) ) ;
#114471 = VECTOR ( 'NONE', #84134, 1000.000000000000000 ) ;
#114472 = EDGE_LOOP ( 'NONE', ( #91132, #118493, #110671, #110982 ) ) ;
#114473 = DIRECTION ( 'NONE',  ( 0.000000000000000000, 0.000000000000000000, 1.000000000000000000 ) ) ;
#114474 = FACE_OUTER_BOUND ( 'NONE', #112444, .T. ) ;
#114475 = CIRCLE ( 'NONE', #16253, 0.06509327318403745899 ) ;
#114476 = AXIS2_PLACEMENT_3D ( 'NONE', #89380, #57990, #97892 ) ;
#114477 = ORIENTED_EDGE ( 'NONE', *, *, #16430, .T. ) ;
#114478 = CIRCLE ( 'NONE', #49761, 0.06509327318403741736 ) ;
#114479 = FACE_OUTER_BOUND ( 'NONE', #124714, .T. ) ;
#114480 = CARTESIAN_POINT ( 'NONE',  ( 186.7812500006828031, 0.000000000000000000, 7.700000000000000178 ) ) ;
#114481 = CARTESIAN_POINT ( 'NONE',  ( -7.100000000000013856, 2.500000000000000000, 5.122947341949749323 ) ) ;
#114482 = VERTEX_POINT ( 'NONE', #120104 ) ;
#114483 = EDGE_LOOP ( 'NONE', ( #100028, #119067, #33718, #55721 ) ) ;
#114484 = AXIS2_PLACEMENT_3D ( 'NONE', #106464, #118220, #58026 ) ;
#114485 = CARTESIAN_POINT ( 'NONE',  ( -6.250000000000017764, 2.500000000000000000, 7.188010851410848723 ) ) ;
#114486 = ORIENTED_EDGE ( 'NONE', *, *, #3079, .F. ) ;
#114487 = DIRECTION ( 'NONE',  ( 0.000000000000000000, 0.000000000000000000, 1.000000000000000000 ) ) ;
#114488 = CARTESIAN_POINT ( 'NONE',  ( -6.650000000000015454, 12.50000000000000000, 7.188010851410848723 ) ) ;
#114489 = AXIS2_PLACEMENT_3D ( 'NONE', #20010, #109004, #8868 ) ;
#114490 = EDGE_LOOP ( 'NONE', ( #93741, #126867, #89060, #7745 ) ) ;
#114491 = CARTESIAN_POINT ( 'NONE',  ( 1.849999999999950129, 2.500000000000000000, -6.841600689897078702 ) ) ;
#114492 = DIRECTION ( 'NONE',  ( 0.000000000000000000, -0.9999939076577903929, 0.003490651415223739937 ) ) ;
#114493 = DIRECTION ( 'NONE',  ( 0.000000000000000000, -0.9999939076577903929, 0.003490651415223739937 ) ) ;
#114494 = DIRECTION ( 'NONE',  ( -4.274815082592931898E-19, -0.9999939076577903929, -0.003490651415223739937 ) ) ;
#114495 = CARTESIAN_POINT ( 'NONE',  ( -2.900000000000029665, 2.500000000000000000, 4.330127018922196314 ) ) ;
#114496 = ORIENTED_EDGE ( 'NONE', *, *, #99979, .T. ) ;
#114497 = EDGE_CURVE ( 'NONE', #33480, #45085, #56979, .T. ) ;
#114498 = ORIENTED_EDGE ( 'NONE', *, *, #45455, .T. ) ;
#114499 = DIRECTION ( 'NONE',  ( 0.000000000000000000, -0.000000000000000000, 1.000000000000000000 ) ) ;
#114500 = DIRECTION ( 'NONE',  ( 0.000000000000000000, 1.000000000000000000, 0.000000000000000000 ) ) ;
#114501 = DIRECTION ( 'NONE',  ( 0.000000000000000000, 0.000000000000000000, -1.000000000000000000 ) ) ;
#114503 = ORIENTED_EDGE ( 'NONE', *, *, #59049, .T. ) ;
#114502 = ORIENTED_EDGE ( 'NONE', *, *, #113153, .F. ) ;
#114504 = EDGE_LOOP ( 'NONE', ( #122388, #59924 ) ) ;
#114505 = CARTESIAN_POINT ( 'NONE',  ( 3.349999999999943689, 2.500000000000000000, 1.472243186433545459 ) ) ;
#114506 = DIRECTION ( 'NONE',  ( -0.000000000000000000, 1.000000000000000000, -0.000000000000000000 ) ) ;
#114507 = LINE ( 'NONE', #7126, #83188 ) ;
#114508 =( NAMED_UNIT ( * ) PLANE_ANGLE_UNIT ( ) SI_UNIT ( $, .RADIAN. ) );
#114509 = LINE ( 'NONE', #2617, #66146 ) ;
#114510 = DIRECTION ( 'NONE',  ( 0.000000000000000000, 0.000000000000000000, -1.000000000000000000 ) ) ;
#114511 = DIRECTION ( 'NONE',  ( 0.000000000000000000, 0.000000000000000000, -1.000000000000000000 ) ) ;
#114512 = PLANE ( 'NONE',  #107716 ) ;
#114513 = CARTESIAN_POINT ( 'NONE',  ( 3.549999999999943867, 2.500000000000000000, -1.818653347947326138 ) ) ;
#114514 = CARTESIAN_POINT ( 'NONE',  ( 7.049999999999926992, 12.50000000000000000, 2.230156782645134950 ) ) ;
#114515 = EDGE_LOOP ( 'NONE', ( #36487, #12279 ) ) ;
#114516 = CONICAL_SURFACE ( 'NONE', #14161, 0.1000000000000002554, 0.003490658503988666988 ) ;
#114517 = CARTESIAN_POINT ( 'NONE',  ( 2.899999999999946620, 2.500000000000000000, -4.922947341949753586 ) ) ;
#114518 = ORIENTED_EDGE ( 'NONE', *, *, #89517, .T. ) ;
#114519 = ORIENTED_EDGE ( 'NONE', *, *, #67657, .F. ) ;
#114520 = FACE_OUTER_BOUND ( 'NONE', #62659, .T. ) ;
#114521 = DIRECTION ( 'NONE',  ( -4.274815082592931898E-19, -0.9999939076577903929, -0.003490651415223739937 ) ) ;
#114522 = DIRECTION ( 'NONE',  ( -0.000000000000000000, -1.000000000000000000, -0.000000000000000000 ) ) ;
#114523 = CIRCLE ( 'NONE', #1657, 0.09999999999999982514 ) ;
#114524 = DIRECTION ( 'NONE',  ( 0.000000000000000000, 0.000000000000000000, 1.000000000000000000 ) ) ;
#114525 = VECTOR ( 'NONE', #49188, 1000.000000000000000 ) ;
#114526 = AXIS2_PLACEMENT_3D ( 'NONE', #103343, #13648, #101407 ) ;
#114527 = DIRECTION ( 'NONE',  ( 0.000000000000000000, 0.000000000000000000, -1.000000000000000000 ) ) ;
#114528 = CARTESIAN_POINT ( 'NONE',  ( 9.399999999999918643, 12.50000000000000000, 0.4115034346978110880 ) ) ;
#114529 = DIRECTION ( 'NONE',  ( 0.000000000000000000, 0.000000000000000000, 1.000000000000000000 ) ) ;
#114530 = ORIENTED_EDGE ( 'NONE', *, *, #107886, .T. ) ;
#114531 = DIRECTION ( 'NONE',  ( 0.000000000000000000, 0.000000000000000000, 1.000000000000000000 ) ) ;
#114532 = CARTESIAN_POINT ( 'NONE',  ( -4.150000000000025224, 12.50000000000000000, 7.122917578226811486 ) ) ;
#114533 = ORIENTED_EDGE ( 'NONE', *, *, #32738, .T. ) ;
#114535 = ADVANCED_FACE ( 'NONE', ( #81469 ), #102966, .T. ) ;
#114534 = CIRCLE ( 'NONE', #104089, 0.1000000000000002554 ) ;
#114536 = EDGE_LOOP ( 'NONE', ( #25605, #125589 ) ) ;
#114537 = ORIENTED_EDGE ( 'NONE', *, *, #50306, .F. ) ;
#114538 = EDGE_CURVE ( 'NONE', #49438, #65903, #59265, .T. ) ;
#114539 = VERTEX_POINT ( 'NONE', #99176 ) ;
#114540 = EDGE_CURVE ( 'NONE', #110245, #94388, #90632, .T. ) ;
#114541 = DIRECTION ( 'NONE',  ( 0.000000000000000000, 0.000000000000000000, 1.000000000000000000 ) ) ;
#114542 = FACE_OUTER_BOUND ( 'NONE', #56149, .T. ) ;
#114543 = CIRCLE ( 'NONE', #85302, 0.06509327318403745899 ) ;
#114544 = DIRECTION ( 'NONE',  ( 0.000000000000000000, 1.000000000000000000, 0.000000000000000000 ) ) ;
#114545 = DIRECTION ( 'NONE',  ( 0.000000000000000000, 0.000000000000000000, 1.000000000000000000 ) ) ;
#114546 = EDGE_CURVE ( 'NONE', #10471, #76809, #68408, .T. ) ;
#114547 = CARTESIAN_POINT ( 'NONE',  ( -8.750000000000008882, 2.500000000000000000, 1.472243186433545459 ) ) ;
#114549 = ORIENTED_EDGE ( 'NONE', *, *, #62469, .F. ) ;
#114548 = EDGE_CURVE ( 'NONE', #83056, #9531, #129300, .T. ) ;
#114550 = CARTESIAN_POINT ( 'NONE',  ( 3.749999999999944045, 2.500000000000000000, -7.088010851410853519 ) ) ;
#114551 = EDGE_CURVE ( 'NONE', #18098, #37160, #17258, .T. ) ;
#114552 = EDGE_CURVE ( 'NONE', #64139, #14119, #13058, .T. ) ;
#114553 = DIRECTION ( 'NONE',  ( 0.000000000000000000, 0.000000000000000000, 1.000000000000000000 ) ) ;
#114554 = AXIS2_PLACEMENT_3D ( 'NONE', #21806, #61735, #99068 ) ;
#114555 = AXIS2_PLACEMENT_3D ( 'NONE', #109360, #49183, #40655 ) ;
#114556 = FACE_OUTER_BOUND ( 'NONE', #32271, .T. ) ;
#114557 = EDGE_LOOP ( 'NONE', ( #55608, #6782, #106660, #128933 ) ) ;
#114558 = AXIS2_PLACEMENT_3D ( 'NONE', #122639, #11384, #102985 ) ;
#114559 = EDGE_LOOP ( 'NONE', ( #76055, #117809 ) ) ;
#114560 = VERTEX_POINT ( 'NONE', #80828 ) ;
#114561 = FACE_OUTER_BOUND ( 'NONE', #123770, .T. ) ;
#114562 = AXIS2_PLACEMENT_3D ( 'NONE', #108698, #39346, #49800 ) ;
#114563 = DIRECTION ( 'NONE',  ( 0.000000000000000000, 0.000000000000000000, -1.000000000000000000 ) ) ;
#114564 = CARTESIAN_POINT ( 'NONE',  ( -9.200000000000009948, 12.50000000000000000, -4.330127018922197202 ) ) ;
#114565 = ORIENTED_EDGE ( 'NONE', *, *, #26542, .T. ) ;
#114566 = DIRECTION ( 'NONE',  ( 0.000000000000000000, 0.000000000000000000, -1.000000000000000000 ) ) ;
#114568 = CIRCLE ( 'NONE', #56084, 0.06509327318403745899 ) ;
#114567 = FACE_OUTER_BOUND ( 'NONE', #80371, .T. ) ;
#114569 = DIRECTION ( 'NONE',  ( 0.000000000000000000, 1.000000000000000000, 0.000000000000000000 ) ) ;
#114570 = FACE_OUTER_BOUND ( 'NONE', #96059, .T. ) ;
#114571 = CARTESIAN_POINT ( 'NONE',  ( -6.650000000000015454, 12.50000000000000000, 2.857883832488649301 ) ) ;
#114572 = EDGE_LOOP ( 'NONE', ( #69550, #83415, #63581, #32713 ) ) ;
#114574 = AXIS2_PLACEMENT_3D ( 'NONE', #22368, #53105, #23633 ) ;
#114573 = CONICAL_SURFACE ( 'NONE', #89544, 0.1000000000000002554, 0.003490658503988666988 ) ;
#114575 = CARTESIAN_POINT ( 'NONE',  ( -10.85000000000000142, 2.500000000000000000, -5.902370205355746968 ) ) ;
#114576 = ORIENTED_EDGE ( 'NONE', *, *, #75452, .F. ) ;
#114577 = EDGE_LOOP ( 'NONE', ( #72697, #2091, #120577, #56 ) ) ;
#114578 = ADVANCED_FACE ( 'NONE', ( #120738 ), #31094, .T. ) ;
#114579 = CARTESIAN_POINT ( 'NONE',  ( -10.65000000000000213, 12.50000000000000000, 1.818653347947321475 ) ) ;
#114580 = FACE_BOUND ( 'NONE', #59896, .T. ) ;
#114581 = DIRECTION ( 'NONE',  ( 0.000000000000000000, 0.000000000000000000, -1.000000000000000000 ) ) ;
#114582 = DIRECTION ( 'NONE',  ( 0.000000000000000000, 1.000000000000000000, 0.000000000000000000 ) ) ;
#114583 = DIRECTION ( 'NONE',  ( 0.000000000000000000, 0.000000000000000000, -1.000000000000000000 ) ) ;
#114584 = ORIENTED_EDGE ( 'NONE', *, *, #51055, .F. ) ;
#114585 = EDGE_CURVE ( 'NONE', #26891, #76567, #21911, .T. ) ;
#114586 = VECTOR ( 'NONE', #30926, 1000.000000000000000 ) ;
#114587 = ORIENTED_EDGE ( 'NONE', *, *, #7831, .F. ) ;
#114588 = ADVANCED_FACE ( 'NONE', ( #13990 ), #122039, .T. ) ;
#114589 = DIRECTION ( 'NONE',  ( 0.000000000000000000, 0.000000000000000000, 1.000000000000000000 ) ) ;
#114590 = DIRECTION ( 'NONE',  ( 0.000000000000000000, 0.000000000000000000, 1.000000000000000000 ) ) ;
#114591 = CARTESIAN_POINT ( 'NONE',  ( 16.98389417445357452, -2.499999999999999556, -5.627887362461234666 ) ) ;
#114592 = ADVANCED_FACE ( 'NONE', ( #113491 ), #72299, .T. ) ;
#114593 = FACE_OUTER_BOUND ( 'NONE', #93058, .T. ) ;
#114594 = ORIENTED_EDGE ( 'NONE', *, *, #91255, .T. ) ;
#114595 = CARTESIAN_POINT ( 'NONE',  ( -12.29999999999999538, 12.50000000000000000, -4.676537180435976104 ) ) ;
#114596 = CIRCLE ( 'NONE', #39425, 0.06509327318403745899 ) ;
#114597 = DIRECTION ( 'NONE',  ( 0.000000000000000000, 0.000000000000000000, 1.000000000000000000 ) ) ;
#114598 = AXIS2_PLACEMENT_3D ( 'NONE', #30, #30158, #81806 ) ;
#114599 = EDGE_CURVE ( 'NONE', #100830, #42825, #44475, .T. ) ;
#114600 = VERTEX_POINT ( 'NONE', #112214 ) ;
#114601 = CARTESIAN_POINT ( 'NONE',  ( 10.44999999999991047, 2.500000000000000000, -6.495190528383302464 ) ) ;
#114602 = EDGE_CURVE ( 'NONE', #79817, #93212, #22560, .T. ) ;
#114603 = ORIENTED_EDGE ( 'NONE', *, *, #125950, .T. ) ;
#114604 = FACE_BOUND ( 'NONE', #51409, .T. ) ;
#114605 = FACE_OUTER_BOUND ( 'NONE', #17441, .T. ) ;
#114606 = EDGE_CURVE ( 'NONE', #69532, #76244, #92569, .T. ) ;
#114608 = EDGE_CURVE ( 'NONE', #79956, #53157, #84176, .T. ) ;
#114607 = AXIS2_PLACEMENT_3D ( 'NONE', #51750, #12448, #40004 ) ;
#114609 = EDGE_CURVE ( 'NONE', #26275, #59971, #61837, .T. ) ;
#114610 = VERTEX_POINT ( 'NONE', #23173 ) ;
#114611 = DIRECTION ( 'NONE',  ( -0.000000000000000000, 1.000000000000000000, -0.000000000000000000 ) ) ;
#114612 = DIRECTION ( 'NONE',  ( -0.000000000000000000, 1.000000000000000000, -0.000000000000000000 ) ) ;
#114613 = ORIENTED_EDGE ( 'NONE', *, *, #20277, .F. ) ;
#114614 = ORIENTED_EDGE ( 'NONE', *, *, #120078, .F. ) ;
#114615 = CARTESIAN_POINT ( 'NONE',  ( 186.8385416670080872, 6.551208109652274736, 3.782341765625001351 ) ) ;
#114616 = EDGE_CURVE ( 'NONE', #55512, #20680, #4747, .T. ) ;
#114617 = CARTESIAN_POINT ( 'NONE',  ( 185.8385416670080872, 6.551208109652274736, 3.782341765625001351 ) ) ;
#114618 = DIRECTION ( 'NONE',  ( -0.000000000000000000, 1.000000000000000000, -0.000000000000000000 ) ) ;
#114619 = AXIS2_PLACEMENT_3D ( 'NONE', #72594, #61492, #22863 ) ;
#114620 = CARTESIAN_POINT ( 'NONE',  ( 4.999999999999938716, 2.500000000000000000, -5.022947341949754119 ) ) ;
#114621 = CARTESIAN_POINT ( 'NONE',  ( -6.700000000000016165, 12.50000000000000000, 4.330127018922196314 ) ) ;
#114622 = FACE_OUTER_BOUND ( 'NONE', #87954, .T. ) ;
#114623 = CARTESIAN_POINT ( 'NONE',  ( 0.6499999999999561684, 2.500000000000000000, 2.411473670974873862 ) ) ;
#114624 = AXIS2_PLACEMENT_3D ( 'NONE', #64096, #82467, #14960 ) ;
#114625 = VERTEX_POINT ( 'NONE', #62482 ) ;
#114626 = ORIENTED_EDGE ( 'NONE', *, *, #10704, .F. ) ;
#114627 = DIRECTION ( 'NONE',  ( -0.000000000000000000, 1.000000000000000000, -0.000000000000000000 ) ) ;
#114628 = CARTESIAN_POINT ( 'NONE',  ( 187.3333333333333144, 6.668395609140177704, -3.849999999999998312 ) ) ;
#114629 = FACE_OUTER_BOUND ( 'NONE', #50115, .T. ) ;
#114630 = AXIS2_PLACEMENT_3D ( 'NONE', #95083, #103621, #104879 ) ;
#114631 = DIRECTION ( 'NONE',  ( -0.000000000000000000, -1.000000000000000000, -0.000000000000000000 ) ) ;
#114633 = EDGE_LOOP ( 'NONE', ( #116119, #112356 ) ) ;
#114632 = EDGE_LOOP ( 'NONE', ( #43649, #10544 ) ) ;
#114634 = FACE_BOUND ( 'NONE', #115469, .T. ) ;
#114635 = VERTEX_POINT ( 'NONE', #101749 ) ;
#114636 = EDGE_CURVE ( 'NONE', #57530, #65577, #123951, .T. ) ;
#114637 = FACE_OUTER_BOUND ( 'NONE', #105343, .T. ) ;
#114638 = DIRECTION ( 'NONE',  ( -0.000000000000000000, 1.000000000000000000, -0.000000000000000000 ) ) ;
#114639 = ORIENTED_EDGE ( 'NONE', *, *, #84591, .T. ) ;
#114640 = FACE_OUTER_BOUND ( 'NONE', #82424, .T. ) ;
#114641 = CIRCLE ( 'NONE', #47761, 0.06509327318403745899 ) ;
#114642 = CARTESIAN_POINT ( 'NONE',  ( 5.649999999999936406, 2.500000000000000000, -6.048780366869526581 ) ) ;
#114643 = CARTESIAN_POINT ( 'NONE',  ( -11.69999999999999929, 12.50000000000000000, -0.06509327318403569651 ) ) ;
#114644 = DIRECTION ( 'NONE',  ( 0.000000000000000000, 0.000000000000000000, 1.000000000000000000 ) ) ;
#114645 = MECHANICAL_DESIGN_GEOMETRIC_PRESENTATION_REPRESENTATION (  '', ( #33199 ), #74948 ) ;
#114646 = CARTESIAN_POINT ( 'NONE',  ( 3.149999999999944400, 12.50000000000000000, 1.818653347947321475 ) ) ;
#114647 = LINE ( 'NONE', #123816, #109071 ) ;
#114648 = CARTESIAN_POINT ( 'NONE',  ( -10.20000000000000284, 2.500000000000000000, 3.983716857408420964 ) ) ;
#114649 = PLANE ( 'NONE',  #38107 ) ;
#114650 = CIRCLE ( 'NONE', #60308, 0.06509327318403745899 ) ;
#114651 = DIRECTION ( 'NONE',  ( 0.000000000000000000, 0.000000000000000000, 1.000000000000000000 ) ) ;
#114652 = ORIENTED_EDGE ( 'NONE', *, *, #116175, .T. ) ;
#114654 = ORIENTED_EDGE ( 'NONE', *, *, #98864, .F. ) ;
#114653 = AXIS2_PLACEMENT_3D ( 'NONE', #91728, #80633, #60357 ) ;
#114655 = ADVANCED_FACE ( 'NONE', ( #34314 ), #48696, .T. ) ;
#114656 = ORIENTED_EDGE ( 'NONE', *, *, #11073, .T. ) ;
#114657 = FACE_OUTER_BOUND ( 'NONE', #22201, .T. ) ;
#114658 = EDGE_LOOP ( 'NONE', ( #43627, #17942, #24866, #18493 ) ) ;
#114659 = CARTESIAN_POINT ( 'NONE',  ( 9.549999999999915445, 2.500000000000000000, 6.395190528383296602 ) ) ;
#114661 = ORIENTED_EDGE ( 'NONE', *, *, #13826, .F. ) ;
#114660 = EDGE_LOOP ( 'NONE', ( #950, #21169 ) ) ;
#114662 = EDGE_LOOP ( 'NONE', ( #30390, #81478, #21251, #24310 ) ) ;
#114663 = AXIS2_PLACEMENT_3D ( 'NONE', #72162, #12568, #123808 ) ;
#114664 = CARTESIAN_POINT ( 'NONE',  ( 10.64999999999991331, 12.50000000000000000, -2.511473670974877948 ) ) ;
#114665 = DIRECTION ( 'NONE',  ( -0.000000000000000000, -1.000000000000000000, -0.000000000000000000 ) ) ;
#114666 = DIRECTION ( 'NONE',  ( -0.000000000000000000, -1.000000000000000000, -0.000000000000000000 ) ) ;
#114667 = DIRECTION ( 'NONE',  ( 0.000000000000000000, 0.000000000000000000, 1.000000000000000000 ) ) ;
#114668 = DIRECTION ( 'NONE',  ( 0.000000000000000000, 0.000000000000000000, 1.000000000000000000 ) ) ;
#114669 = CONICAL_SURFACE ( 'NONE', #81233, 0.1000000000000002554, 0.003490658503988666988 ) ;
#114670 = ADVANCED_FACE ( 'NONE', ( #13352 ), #103690, .T. ) ;
#114671 = VERTEX_POINT ( 'NONE', #53936 ) ;
#114672 = CARTESIAN_POINT ( 'NONE',  ( -0.6500000000000389910, 12.50000000000000000, -1.818653347947326138 ) ) ;
#114673 = ORIENTED_EDGE ( 'NONE', *, *, #16166, .F. ) ;
#114675 = VECTOR ( 'NONE', #94135, 1000.000000000000000 ) ;
#114674 = AXIS2_PLACEMENT_3D ( 'NONE', #6324, #77031, #16148 ) ;
#114676 = ORIENTED_EDGE ( 'NONE', *, *, #46571, .F. ) ;
#114677 = EDGE_LOOP ( 'NONE', ( #74552, #20061, #2007, #57157 ) ) ;
#114678 = CARTESIAN_POINT ( 'NONE',  ( -4.150000000000024336, 12.50000000000000000, -2.099970236277064473 ) ) ;
#114679 = ORIENTED_EDGE ( 'NONE', *, *, #29692, .F. ) ;
#114680 = EDGE_LOOP ( 'NONE', ( #43240, #127652 ) ) ;
#114681 = ORIENTED_EDGE ( 'NONE', *, *, #73935, .F. ) ;
#114682 = DIRECTION ( 'NONE',  ( -0.000000000000000000, -1.000000000000000000, -0.000000000000000000 ) ) ;
#114683 = CARTESIAN_POINT ( 'NONE',  ( -13.94999999999998863, 2.500000000000000000, -1.818653347947323917 ) ) ;
#114684 = CARTESIAN_POINT ( 'NONE',  ( 8.149999999999920419, 12.50000000000000000, 6.841600689897072485 ) ) ;
#114685 = CARTESIAN_POINT ( 'NONE',  ( -0.2000000000000399791, 12.50000000000000000, -4.676537180435977881 ) ) ;
#114686 = PLANE ( 'NONE',  #118187 ) ;
#114687 = CARTESIAN_POINT ( 'NONE',  ( -2.500000000000032863, 12.50000000000000000, 5.022947341949748790 ) ) ;
#114688 = VERTEX_POINT ( 'NONE', #4166 ) ;
#114689 = FACE_OUTER_BOUND ( 'NONE', #75228, .T. ) ;
#114690 = VERTEX_POINT ( 'NONE', #52635 ) ;
#114692 = DIRECTION ( 'NONE',  ( 0.000000000000000000, 1.000000000000000000, 0.000000000000000000 ) ) ;
#114691 = AXIS2_PLACEMENT_3D ( 'NONE', #126973, #37313, #17644 ) ;
#114693 = ADVANCED_FACE ( 'NONE', ( #2908 ), #126033, .T. ) ;
#114695 = ORIENTED_EDGE ( 'NONE', *, *, #91198, .F. ) ;
#114694 = AXIS2_PLACEMENT_3D ( 'NONE', #13753, #94258, #86365 ) ;
#114696 = DIRECTION ( 'NONE',  ( -0.000000000000000000, 1.000000000000000000, -0.000000000000000000 ) ) ;
#114697 = VECTOR ( 'NONE', #56072, 1000.000000000000000 ) ;
#114698 = ORIENTED_EDGE ( 'NONE', *, *, #75702, .T. ) ;
#114699 = ORIENTED_EDGE ( 'NONE', *, *, #107376, .T. ) ;
#114700 = ADVANCED_FACE ( 'NONE', ( #82770 ), #46625, .T. ) ;
#114702 = PLANE ( 'NONE',  #120100 ) ;
#114701 = CONICAL_SURFACE ( 'NONE', #41578, 0.09999999999999982514, 0.003490658503988666988 ) ;
#114703 = DIRECTION ( 'NONE',  ( 0.000000000000000000, 0.000000000000000000, 1.000000000000000000 ) ) ;
#114704 = CIRCLE ( 'NONE', #95928, 0.06509327318403745899 ) ;
#114705 = AXIS2_PLACEMENT_3D ( 'NONE', #45640, #64614, #46929 ) ;
#114706 = DIRECTION ( 'NONE',  ( -0.000000000000000000, 1.000000000000000000, -0.000000000000000000 ) ) ;
#114707 = ADVANCED_FACE ( 'NONE', ( #122670 ), #3543, .T. ) ;
#114708 = CARTESIAN_POINT ( 'NONE',  ( -6.650000000000018119, 12.50000000000000000, -2.165063509461101710 ) ) ;
#114710 = ORIENTED_EDGE ( 'NONE', *, *, #51603, .F. ) ;
#114709 = ADVANCED_FACE ( 'NONE', ( #84677 ), #108665, .F. ) ;
#114711 = DIRECTION ( 'NONE',  ( 0.000000000000000000, 0.000000000000000000, -1.000000000000000000 ) ) ;
#114712 = CARTESIAN_POINT ( 'NONE',  ( -2.100000000000034728, 12.50000000000000000, 4.330127018922196314 ) ) ;
#114713 = ADVANCED_FACE ( 'NONE', ( #116550 ), #121832, .T. ) ;
#114714 = DIRECTION ( 'NONE',  ( 0.000000000000000000, 0.000000000000000000, 1.000000000000000000 ) ) ;
#114715 = EDGE_CURVE ( 'NONE', #75618, #78396, #109310, .T. ) ;
#114716 = EDGE_CURVE ( 'NONE', #116590, #126587, #90537, .T. ) ;
#114717 = FACE_OUTER_BOUND ( 'NONE', #65730, .T. ) ;
#114718 = LINE ( 'NONE', #7333, #121152 ) ;
#114719 = CONICAL_SURFACE ( 'NONE', #12215, 0.1000000000000002554, 0.003490658503988666988 ) ;
#114720 = VERTEX_POINT ( 'NONE', #37371 ) ;
#114721 = EDGE_LOOP ( 'NONE', ( #44540, #33545 ) ) ;
#114722 = ADVANCED_FACE ( 'NONE', ( #68092 ), #26892, .T. ) ;
#114723 = ORIENTED_EDGE ( 'NONE', *, *, #45454, .F. ) ;
#114724 = ADVANCED_FACE ( 'NONE', ( #78591 ), #31978, .T. ) ;
#114725 = DIRECTION ( 'NONE',  ( 0.000000000000000000, -0.000000000000000000, 1.000000000000000000 ) ) ;
#114727 = CONICAL_SURFACE ( 'NONE', #97996, 0.1000000000000002554, 0.003490658503988666988 ) ;
#114726 = CARTESIAN_POINT ( 'NONE',  ( -11.25000000000000000, 12.50000000000000000, 2.857883832488649301 ) ) ;
#114728 = EDGE_CURVE ( 'NONE', #103358, #22461, #89036, .T. ) ;
#114729 = CIRCLE ( 'NONE', #85491, 0.09999999999999999167 ) ;
#114730 = CARTESIAN_POINT ( 'NONE',  ( 184.7552083336747444, 6.551208109652275624, -3.782341765624998686 ) ) ;
#114731 = CARTESIAN_POINT ( 'NONE',  ( 9.149999999999920419, 2.500000000000000000, -7.088010851410853519 ) ) ;
#114732 = CARTESIAN_POINT ( 'NONE',  ( -7.700000000000014388, 12.50000000000000000, -4.741630453620015118 ) ) ;
#114733 = LINE ( 'NONE', #83359, #48146 ) ;
#114734 = LINE ( 'NONE', #45372, #118630 ) ;
#114735 = EDGE_LOOP ( 'NONE', ( #53706, #27959 ) ) ;
#114736 = CARTESIAN_POINT ( 'NONE',  ( 7.699999999999923794, 2.500000000000000000, -0.3464101615137783474 ) ) ;
#114737 = DIRECTION ( 'NONE',  ( 0.000000000000000000, 1.000000000000000000, 0.000000000000000000 ) ) ;
#114738 = CONICAL_SURFACE ( 'NONE', #129443, 0.1000000000000002554, 0.003490658503988666988 ) ;
#114739 = ORIENTED_EDGE ( 'NONE', *, *, #69967, .F. ) ;
#114740 = AXIS2_PLACEMENT_3D ( 'NONE', #96475, #116129, #66388 ) ;
#114741 = DIRECTION ( 'NONE',  ( 0.000000000000000000, 0.000000000000000000, -1.000000000000000000 ) ) ;
#114742 = CIRCLE ( 'NONE', #89623, 0.06509327318403745899 ) ;
#114743 = ORIENTED_EDGE ( 'NONE', *, *, #79398, .T. ) ;
#114744 = DIRECTION ( 'NONE',  ( 0.000000000000000000, 0.000000000000000000, 1.000000000000000000 ) ) ;
#114745 = ORIENTED_EDGE ( 'NONE', *, *, #76474, .F. ) ;
#114747 = CIRCLE ( 'NONE', #54122, 9.000000000000001776 ) ;
#114746 = DIRECTION ( 'NONE',  ( 0.000000000000000000, 0.000000000000000000, 1.000000000000000000 ) ) ;
#114748 = CARTESIAN_POINT ( 'NONE',  ( 0.4499999999999569344, 2.500000000000000000, 2.165063509461097713 ) ) ;
#114749 = LINE ( 'NONE', #15242, #6703 ) ;
#114750 = ORIENTED_EDGE ( 'NONE', *, *, #69459, .T. ) ;
#114751 = CARTESIAN_POINT ( 'NONE',  ( -11.05000000000000249, 2.500000000000000000, -1.818653347947322141 ) ) ;
#114753 = CONICAL_SURFACE ( 'NONE', #123089, 0.1000000000000000472, 0.003490658503988666988 ) ;
#114752 = CIRCLE ( 'NONE', #58351, 0.06509327318403741736 ) ;
#114754 = CARTESIAN_POINT ( 'NONE',  ( 186.5416666666666572, -4.445597072760092416, 7.700000000000049916 ) ) ;
#114755 = AXIS2_PLACEMENT_3D ( 'NONE', #26584, #35756, #46873 ) ;
#114756 = ADVANCED_FACE ( 'NONE', ( #87728 ), #111465, .T. ) ;
#114757 = VERTEX_POINT ( 'NONE', #66795 ) ;
#114758 = FACE_OUTER_BOUND ( 'NONE', #83495, .T. ) ;
#114759 = ADVANCED_FACE ( 'NONE', ( #128986 ), #61305, .T. ) ;
#114761 = AXIS2_PLACEMENT_3D ( 'NONE', #111020, #100570, #60038 ) ;
#114760 = CIRCLE ( 'NONE', #43786, 0.09999999999999982514 ) ;
#114762 = ORIENTED_EDGE ( 'NONE', *, *, #114298, .F. ) ;
#114763 = EDGE_CURVE ( 'NONE', #48350, #70125, #58933, .T. ) ;
#114764 = VERTEX_POINT ( 'NONE', #119137 ) ;
#114765 = PLANE ( 'NONE',  #65166 ) ;
#114766 = CARTESIAN_POINT ( 'NONE',  ( 8.549999999999920774, 2.500000000000000000, -2.511473670974877948 ) ) ;
#114767 = EDGE_LOOP ( 'NONE', ( #62476, #81613, #54802, #31399 ) ) ;
#114768 = CARTESIAN_POINT ( 'NONE',  ( 3.349999999999945466, 12.50000000000000000, -2.230156782645139391 ) ) ;
#114769 = DIRECTION ( 'NONE',  ( 0.000000000000000000, 0.000000000000000000, -1.000000000000000000 ) ) ;
#114770 = VERTEX_POINT ( 'NONE', #98840 ) ;
#114771 = EDGE_CURVE ( 'NONE', #59538, #12415, #9182, .T. ) ;
#114772 = DIRECTION ( 'NONE',  ( 0.000000000000000000, 1.000000000000000000, 0.000000000000000000 ) ) ;
#114773 = DIRECTION ( 'NONE',  ( 0.000000000000000000, 0.000000000000000000, 1.000000000000000000 ) ) ;
#114774 = DIRECTION ( 'NONE',  ( -0.000000000000000000, -1.000000000000000000, -0.000000000000000000 ) ) ;
#114775 = CONICAL_SURFACE ( 'NONE', #49973, 0.1000000000000002554, 0.003490658503988666988 ) ;
#114776 = DIRECTION ( 'NONE',  ( -0.000000000000000000, 1.000000000000000000, -0.000000000000000000 ) ) ;
#114777 = DIRECTION ( 'NONE',  ( -4.274815082592931898E-19, -0.9999939076577903929, -0.003490651415223739937 ) ) ;
#114778 = CARTESIAN_POINT ( 'NONE',  ( 15.39999999999989200, 2.500000000000000000, 0.6928203230275494784 ) ) ;
#114779 = CIRCLE ( 'NONE', #33344, 0.1000000000000000472 ) ;
#114780 = AXIS2_PLACEMENT_3D ( 'NONE', #44513, #84448, #124377 ) ;
#114781 = ORIENTED_EDGE ( 'NONE', *, *, #10468, .T. ) ;
#114782 = VERTEX_POINT ( 'NONE', #19653 ) ;
#114783 = EDGE_LOOP ( 'NONE', ( #20885, #63961 ) ) ;
#114784 = ORIENTED_EDGE ( 'NONE', *, *, #62445, .F. ) ;
#114785 = CARTESIAN_POINT ( 'NONE',  ( -10.65000000000000391, 2.500000000000000000, -6.248780366869523206 ) ) ;
#114786 = CARTESIAN_POINT ( 'NONE',  ( 2.899999999999946620, 2.500000000000000000, -0.7928203230275543412 ) ) ;
#114787 = LINE ( 'NONE', #85336, #2972 ) ;
#114788 = VERTEX_POINT ( 'NONE', #79225 ) ;
#114789 = FACE_BOUND ( 'NONE', #81107, .T. ) ;
#114790 = ADVANCED_FACE ( 'NONE', ( #29471 ), #21587, .T. ) ;
#114791 = FACE_OUTER_BOUND ( 'NONE', #43788, .T. ) ;
#114792 = CARTESIAN_POINT ( 'NONE',  ( -1.850000000000033396, 2.500000000000000000, -6.741600689897077281 ) ) ;
#114793 = CIRCLE ( 'NONE', #70896, 0.06509327318403745899 ) ;
#114794 = AXIS2_PLACEMENT_3D ( 'NONE', #96640, #16786, #75724 ) ;
#114795 = CARTESIAN_POINT ( 'NONE',  ( -0.4500000000000397571, 12.50000000000000000, -2.230156782645139391 ) ) ;
#114796 = AXIS2_PLACEMENT_3D ( 'NONE', #43220, #33399, #81823 ) ;
#114797 = DIRECTION ( 'NONE',  ( 0.000000000000000000, -0.000000000000000000, 1.000000000000000000 ) ) ;
#114798 = CARTESIAN_POINT ( 'NONE',  ( 10.59999999999990905, 2.500000000000000000, 4.676537180435972552 ) ) ;
#114799 = CARTESIAN_POINT ( 'NONE',  ( -2.700000000000030376, 2.500000000000000000, 3.983716857408420964 ) ) ;
#114800 = FACE_OUTER_BOUND ( 'NONE', #56733, .T. ) ;
#114801 = DIRECTION ( 'NONE',  ( 0.000000000000000000, -0.000000000000000000, 1.000000000000000000 ) ) ;
#114802 = CARTESIAN_POINT ( 'NONE',  ( -0.2000000000000347888, 2.500000000000000000, 0.4464101615137758272 ) ) ;
#114803 = AXIS2_PLACEMENT_3D ( 'NONE', #85939, #18502, #77426 ) ;
#114804 = DIRECTION ( 'NONE',  ( -0.000000000000000000, 1.000000000000000000, -0.000000000000000000 ) ) ;
#114805 = AXIS2_PLACEMENT_3D ( 'NONE', #75124, #115032, #54826 ) ;
#114806 = ORIENTED_EDGE ( 'NONE', *, *, #22038, .T. ) ;
#114807 = ORIENTED_EDGE ( 'NONE', *, *, #52627, .F. ) ;
#114808 = EDGE_CURVE ( 'NONE', #22187, #76885, #30423, .T. ) ;
#114809 = EDGE_LOOP ( 'NONE', ( #76895, #121204 ) ) ;
#114810 = VERTEX_POINT ( 'NONE', #42531 ) ;
#114811 = DIRECTION ( 'NONE',  ( 0.000000000000000000, 0.000000000000000000, 1.000000000000000000 ) ) ;
#114812 = ORIENTED_EDGE ( 'NONE', *, *, #13342, .T. ) ;
#114813 = ORIENTED_EDGE ( 'NONE', *, *, #32775, .F. ) ;
#114814 = VERTEX_POINT ( 'NONE', #82454 ) ;
#114815 = FACE_OUTER_BOUND ( 'NONE', #77697, .T. ) ;
#114816 = DIRECTION ( 'NONE',  ( 0.000000000000000000, 1.000000000000000000, 0.000000000000000000 ) ) ;
#114817 = CARTESIAN_POINT ( 'NONE',  ( 12.89999999999990266, 2.500000000000000000, -3.637306695894650055 ) ) ;
#114818 = CIRCLE ( 'NONE', #104366, 0.1000000000000002554 ) ;
#114819 = DIRECTION ( 'NONE',  ( -0.000000000000000000, -1.000000000000000000, -0.000000000000000000 ) ) ;
#114820 = EDGE_CURVE ( 'NONE', #87351, #64508, #63360, .T. ) ;
#114821 = EDGE_LOOP ( 'NONE', ( #18087, #123051, #10028, #18211 ) ) ;
#114822 = ORIENTED_EDGE ( 'NONE', *, *, #33166, .T. ) ;
#114823 = ORIENTED_EDGE ( 'NONE', *, *, #4604, .T. ) ;
#114825 = EDGE_LOOP ( 'NONE', ( #112147, #1222 ) ) ;
#114824 = DIRECTION ( 'NONE',  ( 0.000000000000000000, 0.000000000000000000, 1.000000000000000000 ) ) ;
#114826 = DIRECTION ( 'NONE',  ( 0.000000000000000000, 1.000000000000000000, 0.000000000000000000 ) ) ;
#114827 = ORIENTED_EDGE ( 'NONE', *, *, #94095, .T. ) ;
#114828 = VERTEX_POINT ( 'NONE', #22884 ) ;
#114829 = AXIS2_PLACEMENT_3D ( 'NONE', #29694, #68968, #108878 ) ;
#114830 = CARTESIAN_POINT ( 'NONE',  ( 1.649999999999951505, 2.500000000000000000, 1.472243186433545459 ) ) ;
#114831 = DIRECTION ( 'NONE',  ( -0.000000000000000000, 1.000000000000000000, -0.000000000000000000 ) ) ;
#114832 = DIRECTION ( 'NONE',  ( -4.274815082592931898E-19, -0.9999939076577903929, -0.003490651415223739937 ) ) ;
#114833 = CARTESIAN_POINT ( 'NONE',  ( -5.600000000000020073, 2.500000000000000000, -0.3464101615137782364 ) ) ;
#114834 = CARTESIAN_POINT ( 'NONE',  ( 6.699999999999928235, 12.50000000000000000, -2.276824562219559311E-15 ) ) ;
#114835 = CIRCLE ( 'NONE', #62635, 0.1000000000000002554 ) ;
#114836 = ORIENTED_EDGE ( 'NONE', *, *, #123821, .T. ) ;
#114837 = CARTESIAN_POINT ( 'NONE',  ( 108.0000000000000142, 9.000000000000001776, -2.249999999999996891 ) ) ;
#114838 = ORIENTED_EDGE ( 'NONE', *, *, #16646, .T. ) ;
#114839 = DIRECTION ( 'NONE',  ( 0.000000000000000000, 1.000000000000000000, 0.000000000000000000 ) ) ;
#114840 = EDGE_CURVE ( 'NONE', #890, #59538, #71766, .T. ) ;
#114842 = AXIS2_PLACEMENT_3D ( 'NONE', #22064, #61982, #110423 ) ;
#114841 = AXIS2_PLACEMENT_3D ( 'NONE', #107805, #27296, #117593 ) ;
#114843 = EDGE_LOOP ( 'NONE', ( #94962, #3577 ) ) ;
#114844 = LINE ( 'NONE', #13424, #29603 ) ;
#114845 = DIRECTION ( 'NONE',  ( 0.000000000000000000, -0.9999939076577903929, 0.003490651415223739937 ) ) ;
#114846 = AXIS2_PLACEMENT_3D ( 'NONE', #11286, #128525, #80035 ) ;
#114847 = DIRECTION ( 'NONE',  ( 0.000000000000000000, 0.000000000000000000, 1.000000000000000000 ) ) ;
#114848 = DIRECTION ( 'NONE',  ( 0.000000000000000000, -0.000000000000000000, 1.000000000000000000 ) ) ;
#114849 = ORIENTED_EDGE ( 'NONE', *, *, #31583, .F. ) ;
#114850 = EDGE_CURVE ( 'NONE', #77606, #90795, #88475, .T. ) ;
#114851 = FACE_OUTER_BOUND ( 'NONE', #60833, .T. ) ;
#114853 = CIRCLE ( 'NONE', #45925, 0.1000000000000000472 ) ;
#114852 = VECTOR ( 'NONE', #78990, 1000.000000000000000 ) ;
#114854 = DIRECTION ( 'NONE',  ( 0.000000000000000000, 0.000000000000000000, -1.000000000000000000 ) ) ;
#114855 = EDGE_LOOP ( 'NONE', ( #56605, #46027 ) ) ;
#114856 = ORIENTED_EDGE ( 'NONE', *, *, #82991, .F. ) ;
#114857 = EDGE_CURVE ( 'NONE', #110459, #75028, #34116, .T. ) ;
#114859 = EDGE_LOOP ( 'NONE', ( #114990, #65128, #84259, #113399 ) ) ;
#114858 = ADVANCED_FACE ( 'NONE', ( #12395 ), #84278, .T. ) ;
#114860 = CARTESIAN_POINT ( 'NONE',  ( 12.09999999999990550, 2.500000000000000000, -5.022947341949754119 ) ) ;
#114861 = PLANE ( 'NONE',  #70089 ) ;
#114862 = EDGE_CURVE ( 'NONE', #30008, #115201, #70679, .T. ) ;
#114863 = CARTESIAN_POINT ( 'NONE',  ( 186.8593750003414016, 0.000000000000000000, 7.564683531250000925 ) ) ;
#114864 = EDGE_CURVE ( 'NONE', #59594, #3679, #27840, .T. ) ;
#114865 = DIRECTION ( 'NONE',  ( 0.000000000000000000, 0.000000000000000000, 1.000000000000000000 ) ) ;
#114866 = DIRECTION ( 'NONE',  ( -0.000000000000000000, -1.000000000000000000, -0.000000000000000000 ) ) ;
#114867 = DIRECTION ( 'NONE',  ( -0.000000000000000000, -1.000000000000000000, -0.000000000000000000 ) ) ;
#114868 = EDGE_CURVE ( 'NONE', #36662, #91613, #102701, .T. ) ;
#114869 = CIRCLE ( 'NONE', #89748, 0.09999999999999982514 ) ;
#114870 = EDGE_CURVE ( 'NONE', #87504, #18257, #1290, .T. ) ;
#114871 = EDGE_CURVE ( 'NONE', #50596, #103587, #71312, .T. ) ;
#114872 = ORIENTED_EDGE ( 'NONE', *, *, #60526, .F. ) ;
#114873 = ADVANCED_FACE ( 'NONE', ( #102079 ), #44574, .T. ) ;
#114874 = DIRECTION ( 'NONE',  ( -0.000000000000000000, -1.000000000000000000, -0.000000000000000000 ) ) ;
#114875 = EDGE_CURVE ( 'NONE', #6351, #77555, #92240, .T. ) ;
#114876 = AXIS2_PLACEMENT_3D ( 'NONE', #18115, #97968, #37771 ) ;
#114877 = ORIENTED_EDGE ( 'NONE', *, *, #87349, .F. ) ;
#114878 = DIRECTION ( 'NONE',  ( -0.000000000000000000, -1.000000000000000000, -0.000000000000000000 ) ) ;
#114879 = CARTESIAN_POINT ( 'NONE',  ( -6.050000000000020250, 2.500000000000000000, -2.611473670974877592 ) ) ;
#114880 = CARTESIAN_POINT ( 'NONE',  ( -0.8500000000000382805, 2.500000000000000000, -2.857883832488653741 ) ) ;
#114881 = EDGE_CURVE ( 'NONE', #97225, #9827, #96785, .T. ) ;
#114882 = VERTEX_POINT ( 'NONE', #111224 ) ;
#114884 = AXIS2_PLACEMENT_3D ( 'NONE', #78642, #79908, #70097 ) ;
#114883 = VECTOR ( 'NONE', #90053, 1000.000000000000000 ) ;
#114885 = VECTOR ( 'NONE', #35959, 1000.000000000000000 ) ;
#114886 = DIRECTION ( 'NONE',  ( -0.000000000000000000, -1.000000000000000000, -0.000000000000000000 ) ) ;
#114887 = DIRECTION ( 'NONE',  ( -4.274815082592931898E-19, -0.9999939076577903929, -0.003490651415223739937 ) ) ;
#114888 = CIRCLE ( 'NONE', #31302, 0.1000000000000002554 ) ;
#114889 = EDGE_LOOP ( 'NONE', ( #27502, #115228 ) ) ;
#114890 = CARTESIAN_POINT ( 'NONE',  ( 4.799999999999937650, 12.50000000000000000, -0.3464101615137782364 ) ) ;
#114891 = AXIS2_PLACEMENT_3D ( 'NONE', #109589, #8780, #118748 ) ;
#114892 = CIRCLE ( 'NONE', #75199, 0.06509327318403745899 ) ;
#114893 = ORIENTED_EDGE ( 'NONE', *, *, #70418, .F. ) ;
#114894 = VERTEX_POINT ( 'NONE', #70043 ) ;
#114895 = DIRECTION ( 'NONE',  ( 0.000000000000000000, 1.000000000000000000, 0.000000000000000000 ) ) ;
#114896 = VERTEX_POINT ( 'NONE', #62166 ) ;
#114897 = PLANE ( 'NONE',  #107095 ) ;
#114898 = CARTESIAN_POINT ( 'NONE',  ( -12.69999999999999396, 2.500000000000000000, 0.2464101615137776757 ) ) ;
#114899 = AXIS2_PLACEMENT_3D ( 'NONE', #85763, #66130, #6527 ) ;
#114900 = CARTESIAN_POINT ( 'NONE',  ( -4.999999999999990230, 12.50000000000000000, -4.330127018922201643 ) ) ;
#114901 = ORIENTED_EDGE ( 'NONE', *, *, #93885, .T. ) ;
#114902 = FACE_BOUND ( 'NONE', #126735, .T. ) ;
#114904 = VERTEX_POINT ( 'NONE', #121704 ) ;
#114903 = DIRECTION ( 'NONE',  ( 0.000000000000000000, 0.000000000000000000, -1.000000000000000000 ) ) ;
#114905 = CARTESIAN_POINT ( 'NONE',  ( -8.150000000000009237, 2.500000000000000000, 6.048780366869520364 ) ) ;
#114906 = DIRECTION ( 'NONE',  ( -0.000000000000000000, 1.000000000000000000, -0.000000000000000000 ) ) ;
#114907 = ORIENTED_EDGE ( 'NONE', *, *, #70691, .F. ) ;
#114908 = ADVANCED_FACE ( 'NONE', ( #2557 ), #32072, .T. ) ;
#114909 = ORIENTED_EDGE ( 'NONE', *, *, #29479, .T. ) ;
#114910 = EDGE_CURVE ( 'NONE', #1125, #103358, #80085, .T. ) ;
#114911 = ORIENTED_EDGE ( 'NONE', *, *, #45150, .F. ) ;
#114912 = CARTESIAN_POINT ( 'NONE',  ( -10.85000000000000142, 2.500000000000000000, -1.372243186433546036 ) ) ;
#114913 = CARTESIAN_POINT ( 'NONE',  ( 2.500000000000002220, 2.499999999999999556, 10.00000000000000533 ) ) ;
#114914 = ADVANCED_FACE ( 'NONE', ( #89678 ), #31753, .T. ) ;
#114915 = LINE ( 'NONE', #14762, #31662 ) ;
#114916 = FACE_BOUND ( 'NONE', #1934, .T. ) ;
#114917 = ORIENTED_EDGE ( 'NONE', *, *, #32708, .F. ) ;
#114918 = CARTESIAN_POINT ( 'NONE',  ( 185.0260416670080588, -6.551208109652273848, -3.782341765625003571 ) ) ;
#114919 = CARTESIAN_POINT ( 'NONE',  ( 10.79999999999991367, 12.50000000000000000, -0.06509327318403980434 ) ) ;
#114920 = CARTESIAN_POINT ( 'NONE',  ( 7.099999999999927702, 2.500000000000000000, -3.737306695894649700 ) ) ;
#114921 = ADVANCED_FACE ( 'NONE', ( #90298 ), #80391, .T. ) ;
#114923 = ADVANCED_FACE ( 'NONE', ( #85000 ), #115665, .T. ) ;
#114922 = DIRECTION ( 'NONE',  ( -0.000000000000000000, -1.000000000000000000, -0.000000000000000000 ) ) ;
#114924 = CARTESIAN_POINT ( 'NONE',  ( -2.499999999999996003, 2.500000000000000000, -4.230127018922201998 ) ) ;
#114925 = CARTESIAN_POINT ( 'NONE',  ( -10.60000000000000142, 2.500000000000000000, -0.2464101615137782308 ) ) ;
#114926 = CONICAL_SURFACE ( 'NONE', #6251, 0.1000000000000000472, 0.003490658503988666988 ) ;
#114927 = DIRECTION ( 'NONE',  ( 0.000000000000000000, 1.000000000000000000, 0.000000000000000000 ) ) ;
#114928 = CARTESIAN_POINT ( 'NONE',  ( -4.600000000000028955, 12.50000000000000000, -4.265033745738164406 ) ) ;
#114929 = CARTESIAN_POINT ( 'NONE',  ( 162.5000000000000000, 0.5000000000000000000, -7.500000000000005329 ) ) ;
#114931 = CONICAL_SURFACE ( 'NONE', #75236, 0.1000000000000002554, 0.003490658503988666988 ) ;
#114930 = CIRCLE ( 'NONE', #62736, 0.06509327318403745899 ) ;
#114932 = EDGE_LOOP ( 'NONE', ( #85544, #119324, #3422, #91862 ) ) ;
#114933 = VERTEX_POINT ( 'NONE', #5781 ) ;
#114934 = ORIENTED_EDGE ( 'NONE', *, *, #56333, .T. ) ;
#114935 = EDGE_LOOP ( 'NONE', ( #122074, #69014 ) ) ;
#114936 = ORIENTED_EDGE ( 'NONE', *, *, #67268, .F. ) ;
#114937 = DIRECTION ( 'NONE',  ( 0.000000000000000000, -1.846105847067148022E-16, 1.000000000000000000 ) ) ;
#114938 = CARTESIAN_POINT ( 'NONE',  ( -0.4000000000000331624, 2.500000000000000000, 0.1000000000000000056 ) ) ;
#114939 = ORIENTED_EDGE ( 'NONE', *, *, #25022, .T. ) ;
#114940 = FACE_BOUND ( 'NONE', #128797, .T. ) ;
#114941 = LINE ( 'NONE', #13521, #89640 ) ;
#114942 = AXIS2_PLACEMENT_3D ( 'NONE', #88336, #98173, #28156 ) ;
#114943 = DIRECTION ( 'NONE',  ( 0.000000000000000000, 1.000000000000000000, 0.000000000000000000 ) ) ;
#114944 = ORIENTED_EDGE ( 'NONE', *, *, #877, .F. ) ;
#114945 = CARTESIAN_POINT ( 'NONE',  ( -7.050000000000013145, 2.500000000000000000, 6.595190528383296780 ) ) ;
#114946 = DIRECTION ( 'NONE',  ( 0.000000000000000000, -0.9999939076577903929, 0.003490651415223739937 ) ) ;
#114947 = DIRECTION ( 'NONE',  ( -0.000000000000000000, 1.000000000000000000, -0.000000000000000000 ) ) ;
#114948 = ORIENTED_EDGE ( 'NONE', *, *, #103180, .F. ) ;
#114949 = CARTESIAN_POINT ( 'NONE',  ( 3.749999999999938716, 2.500000000000000000, 7.188010851410848723 ) ) ;
#114950 = EDGE_CURVE ( 'NONE', #69772, #118395, #9061, .T. ) ;
#114951 = ORIENTED_EDGE ( 'NONE', *, *, #26743, .T. ) ;
#114952 = EDGE_LOOP ( 'NONE', ( #92379, #33758, #15973, #56970 ) ) ;
#114953 = EDGE_LOOP ( 'NONE', ( #90641, #101779 ) ) ;
#114954 = CARTESIAN_POINT ( 'NONE',  ( 10.84999999999991260, 2.500000000000000000, -1.372243186433550033 ) ) ;
#114955 = LINE ( 'NONE', #33830, #14252 ) ;
#114956 = DIRECTION ( 'NONE',  ( 0.000000000000000000, 1.000000000000000000, 0.000000000000000000 ) ) ;
#114957 = ORIENTED_EDGE ( 'NONE', *, *, #70740, .T. ) ;
#114958 = CARTESIAN_POINT ( 'NONE',  ( 10.28037028461878855, 1.500000000000063283, -9.136909653556553934 ) ) ;
#114959 = CIRCLE ( 'NONE', #18825, 0.06509327318403745899 ) ;
#114960 = CARTESIAN_POINT ( 'NONE',  ( -0.6000000000000388356, 2.500000000000000000, 4.576537180435972019 ) ) ;
#114961 = CONICAL_SURFACE ( 'NONE', #58559, 0.1000000000000002554, 0.003490658503988666988 ) ;
#114962 = DIRECTION ( 'NONE',  ( -4.274815082592931898E-19, -0.9999939076577903929, -0.003490651415223739937 ) ) ;
#114963 = CARTESIAN_POINT ( 'NONE',  ( 184.7812500006828031, 0.000000000000000000, 7.700000000000000178 ) ) ;
#114964 = CARTESIAN_POINT ( 'NONE',  ( 6.249999999999934275, 2.500000000000000000, -7.088010851410853519 ) ) ;
#114965 = EDGE_CURVE ( 'NONE', #59645, #121477, #23750, .T. ) ;
#114966 = CARTESIAN_POINT ( 'NONE',  ( 3.949999999999939782, 2.500000000000000000, 2.511473670974873507 ) ) ;
#114967 = EDGE_CURVE ( 'NONE', #55845, #123356, #52975, .T. ) ;
#114968 = VERTEX_POINT ( 'NONE', #85652 ) ;
#114969 = CARTESIAN_POINT ( 'NONE',  ( -6.850000000000013856, 2.500000000000000000, 6.148780366869520897 ) ) ;
#114970 = CIRCLE ( 'NONE', #87783, 0.06509327318403745899 ) ;
#114971 = ORIENTED_EDGE ( 'NONE', *, *, #2226, .T. ) ;
#114972 = ORIENTED_EDGE ( 'NONE', *, *, #41562, .F. ) ;
#114973 = DIRECTION ( 'NONE',  ( 0.000000000000000000, 1.000000000000000000, 0.000000000000000000 ) ) ;
#114974 = DIRECTION ( 'NONE',  ( 0.000000000000000000, 0.000000000000000000, 1.000000000000000000 ) ) ;
#114975 = DIRECTION ( 'NONE',  ( 0.000000000000000000, 0.000000000000000000, -1.000000000000000000 ) ) ;
#114977 = ADVANCED_FACE ( 'NONE', ( #24160 ), #61406, .T. ) ;
#114976 = DIRECTION ( 'NONE',  ( -0.000000000000000000, 1.000000000000000000, -0.000000000000000000 ) ) ;
#114978 = DIRECTION ( 'NONE',  ( 0.000000000000000000, 1.000000000000000000, 0.000000000000000000 ) ) ;
#114979 = AXIS2_PLACEMENT_3D ( 'NONE', #112384, #113015, #33193 ) ;
#114980 = EDGE_LOOP ( 'NONE', ( #92543, #104202, #86294, #114408 ) ) ;
#114981 = ORIENTED_EDGE ( 'NONE', *, *, #70127, .F. ) ;
#114982 = AXIS2_PLACEMENT_3D ( 'NONE', #63709, #12014, #62427 ) ;
#114983 = DIRECTION ( 'NONE',  ( 0.000000000000000000, 0.000000000000000000, 1.000000000000000000 ) ) ;
#114984 = DIRECTION ( 'NONE',  ( 0.000000000000000000, 0.000000000000000000, -1.000000000000000000 ) ) ;
#114985 = CARTESIAN_POINT ( 'NONE',  ( -0.4000000000000392131, 2.500000000000000000, -4.230127018922201998 ) ) ;
#114986 = ORIENTED_EDGE ( 'NONE', *, *, #99826, .T. ) ;
#114987 = VERTEX_POINT ( 'NONE', #113834 ) ;
#114988 = LINE ( 'NONE', #6312, #106297 ) ;
#114989 = VECTOR ( 'NONE', #121675, 1000.000000000000000 ) ;
#114990 = ORIENTED_EDGE ( 'NONE', *, *, #41614, .F. ) ;
#114991 = CARTESIAN_POINT ( 'NONE',  ( -6.450000000000016165, 2.500000000000000000, 6.841600689897072485 ) ) ;
#114992 = DIRECTION ( 'NONE',  ( -0.000000000000000000, -1.000000000000000000, -0.000000000000000000 ) ) ;
#114993 = EDGE_LOOP ( 'NONE', ( #59138, #76530, #103512, #8253 ) ) ;
#114994 = FACE_OUTER_BOUND ( 'NONE', #127990, .T. ) ;
#114995 = CARTESIAN_POINT ( 'NONE',  ( 3.949999999999942446, 2.500000000000000000, -2.511473670974877948 ) ) ;
#114996 = AXIS2_PLACEMENT_3D ( 'NONE', #86433, #117817, #57635 ) ;
#114997 = CARTESIAN_POINT ( 'NONE',  ( -12.49999999999999467, 2.500000000000000000, -3.637306695894647390 ) ) ;
#114998 = CARTESIAN_POINT ( 'NONE',  ( -8.950000000000008171, 2.500000000000000000, -2.511473670974877948 ) ) ;
#114999 = ORIENTED_EDGE ( 'NONE', *, *, #1594, .T. ) ;
#115000 = EDGE_CURVE ( 'NONE', #3252, #47024, #64082, .T. ) ;
#115001 = CARTESIAN_POINT ( 'NONE',  ( 12.89999999999989733, 12.50000000000000000, 0.06509327318403504425 ) ) ;
#115002 = CARTESIAN_POINT ( 'NONE',  ( 1.849999999999950129, 12.50000000000000000, -6.906693963081115939 ) ) ;
#115003 = ORIENTED_EDGE ( 'NONE', *, *, #98575, .F. ) ;
#115004 = EDGE_LOOP ( 'NONE', ( #98176, #102447 ) ) ;
#115005 = EDGE_CURVE ( 'NONE', #2985, #53227, #73906, .T. ) ;
#115006 = CARTESIAN_POINT ( 'NONE',  ( 6.449999999999931788, 2.500000000000000000, -2.511473670974877948 ) ) ;
#115007 = CARTESIAN_POINT ( 'NONE',  ( 10.59999999999990905, 2.500000000000000000, 3.983716857408420076 ) ) ;
#115008 = ADVANCED_FACE ( 'NONE', ( #34647 ), #86416, .T. ) ;
#115009 = DIRECTION ( 'NONE',  ( -0.000000000000000000, -1.000000000000000000, -0.000000000000000000 ) ) ;
#115010 = ADVANCED_FACE ( 'NONE', ( #76490 ), #111561, .T. ) ;
#115011 = DIRECTION ( 'NONE',  ( 0.000000000000000000, -0.000000000000000000, 1.000000000000000000 ) ) ;
#115012 = CARTESIAN_POINT ( 'NONE',  ( 11.64999999999990621, 2.500000000000000000, 6.495190528383297135 ) ) ;
#115013 = LINE ( 'NONE', #93464, #90629 ) ;
#115014 = DIRECTION ( 'NONE',  ( 0.000000000000000000, -0.9999939076577903929, 0.003490651415223739937 ) ) ;
#115015 = DIRECTION ( 'NONE',  ( -0.000000000000000000, -1.000000000000000000, -0.000000000000000000 ) ) ;
#115016 = DIRECTION ( 'NONE',  ( 0.000000000000000000, 0.000000000000000000, 1.000000000000000000 ) ) ;
#115017 = EDGE_CURVE ( 'NONE', #89806, #82531, #105305, .T. ) ;
#115018 = VECTOR ( 'NONE', #45637, 1000.000000000000000 ) ;
#115019 = EDGE_CURVE ( 'NONE', #120570, #89280, #16871, .T. ) ;
#115020 = AXIS2_PLACEMENT_3D ( 'NONE', #45634, #85539, #125463 ) ;
#115021 = EDGE_CURVE ( 'NONE', #3965, #76244, #57185, .T. ) ;
#115022 = DIRECTION ( 'NONE',  ( 0.000000000000000000, 0.000000000000000000, -1.000000000000000000 ) ) ;
#115023 = VERTEX_POINT ( 'NONE', #96112 ) ;
#115026 = EDGE_CURVE ( 'NONE', #88347, #115125, #107868, .T. ) ;
#115025 = AXIS2_PLACEMENT_3D ( 'NONE', #42180, #12690, #82096 ) ;
#115024 = CONICAL_SURFACE ( 'NONE', #125499, 0.1000000000000002554, 0.003490658503988666988 ) ;
#115027 = VERTEX_POINT ( 'NONE', #57490 ) ;
#115028 = EDGE_LOOP ( 'NONE', ( #65537, #79290 ) ) ;
#115029 = ADVANCED_FACE ( 'NONE', ( #128166 ), #87576, .T. ) ;
#115030 = DIRECTION ( 'NONE',  ( -1.000000000000000000, -0.000000000000000000, -0.000000000000000000 ) ) ;
#115031 = DIRECTION ( 'NONE',  ( 0.000000000000000000, 0.000000000000000000, 1.000000000000000000 ) ) ;
#115032 = DIRECTION ( 'NONE',  ( -0.000000000000000000, 1.000000000000000000, -0.000000000000000000 ) ) ;
#115033 = ADVANCED_FACE ( 'NONE', ( #127517 ), #96883, .T. ) ;
#115034 = ORIENTED_EDGE ( 'NONE', *, *, #62798, .F. ) ;
#115035 = DIRECTION ( 'NONE',  ( 0.000000000000000000, 1.000000000000000000, 0.000000000000000000 ) ) ;
#115036 = CARTESIAN_POINT ( 'NONE',  ( -6.050000000000018474, 2.500000000000000000, 6.841600689897072485 ) ) ;
#115038 = ORIENTED_EDGE ( 'NONE', *, *, #90945, .F. ) ;
#115037 = PLANE ( 'NONE',  #14632 ) ;
#115039 = DIRECTION ( 'NONE',  ( -0.000000000000000000, 1.000000000000000000, -0.000000000000000000 ) ) ;
#115040 = ORIENTED_EDGE ( 'NONE', *, *, #71569, .F. ) ;
#115041 = EDGE_LOOP ( 'NONE', ( #71079, #36887, #88203, #47472 ) ) ;
#115042 = EDGE_LOOP ( 'NONE', ( #102555, #117138 ) ) ;
#115043 = VERTEX_POINT ( 'NONE', #98048 ) ;
#115044 = CARTESIAN_POINT ( 'NONE',  ( -8.100000000000013856, 2.500000000000000000, -4.776537180435977525 ) ) ;
#115045 = CARTESIAN_POINT ( 'NONE',  ( 9.599999999999917932, 12.50000000000000000, 0.06509327318403515528 ) ) ;
#115046 = DIRECTION ( 'NONE',  ( 0.000000000000000000, -0.000000000000000000, 1.000000000000000000 ) ) ;
#115047 = DIRECTION ( 'NONE',  ( 0.000000000000000000, 0.000000000000000000, 1.000000000000000000 ) ) ;
#115048 = CIRCLE ( 'NONE', #64972, 0.1000000000000002554 ) ;
#115049 = EDGE_LOOP ( 'NONE', ( #30869, #99677, #86748, #12670 ) ) ;
#115050 = FACE_OUTER_BOUND ( 'NONE', #95035, .T. ) ;
#115051 = ORIENTED_EDGE ( 'NONE', *, *, #108109, .T. ) ;
#115052 = CARTESIAN_POINT ( 'NONE',  ( 65.34954526983784717, -3.515384427023117819, -5.621991122718144496 ) ) ;
#115053 = CARTESIAN_POINT ( 'NONE',  ( -6.249999999999981348, 12.50000000000000000, 6.495190528383297135 ) ) ;
#115054 = CARTESIAN_POINT ( 'NONE',  ( 2.499999999999981792, 2.500000000000000000, 4.330127018922196314 ) ) ;
#115055 = CARTESIAN_POINT ( 'NONE',  ( 17.84432265422780262, -2.533187527835756736, 5.021315468709310892 ) ) ;
#115056 = CONICAL_SURFACE ( 'NONE', #27321, 0.1000000000000002554, 0.003490658503988666988 ) ;
#115057 = ORIENTED_EDGE ( 'NONE', *, *, #111689, .T. ) ;
#115058 = ADVANCED_FACE ( 'NONE', ( #126223 ), #121943, .T. ) ;
#115059 = VERTEX_POINT ( 'NONE', #96745 ) ;
#115060 = EDGE_CURVE ( 'NONE', #120460, #125434, #90630, .T. ) ;
#115061 = EDGE_LOOP ( 'NONE', ( #123370, #89244 ) ) ;
#115062 = FACE_OUTER_BOUND ( 'NONE', #61606, .T. ) ;
#115063 = LINE ( 'NONE', #84974, #5940 ) ;
#115064 = LINE ( 'NONE', #37186, #50348 ) ;
#115065 = FACE_BOUND ( 'NONE', #91454, .T. ) ;
#115066 = DIRECTION ( 'NONE',  ( 0.000000000000000000, 0.000000000000000000, 1.000000000000000000 ) ) ;
#115067 = FACE_OUTER_BOUND ( 'NONE', #40434, .T. ) ;
#115068 = DIRECTION ( 'NONE',  ( 0.000000000000000000, 1.000000000000000000, 0.000000000000000000 ) ) ;
#115069 = AXIS2_PLACEMENT_3D ( 'NONE', #74012, #83819, #31510 ) ;
#115070 = AXIS2_PLACEMENT_3D ( 'NONE', #5120, #124908, #25393 ) ;
#115071 = CARTESIAN_POINT ( 'NONE',  ( 14.14999999999989377, 12.50000000000000000, -2.792790559304616504 ) ) ;
#115072 = CYLINDRICAL_SURFACE ( 'NONE', #21729, 7.700000000000000178 ) ;
#115073 = DIRECTION ( 'NONE',  ( 0.000000000000000000, 0.000000000000000000, 1.000000000000000000 ) ) ;
#115074 = ORIENTED_EDGE ( 'NONE', *, *, #8775, .F. ) ;
#115075 = VECTOR ( 'NONE', #65982, 1000.000000000000000 ) ;
#115076 = CARTESIAN_POINT ( 'NONE',  ( -3.749999999999991562, 2.500000000000000000, 6.595190528383296780 ) ) ;
#115077 = ORIENTED_EDGE ( 'NONE', *, *, #65780, .T. ) ;
#115078 = AXIS2_PLACEMENT_3D ( 'NONE', #19973, #59270, #58615 ) ;
#115079 = ORIENTED_EDGE ( 'NONE', *, *, #70845, .T. ) ;
#115080 = ORIENTED_EDGE ( 'NONE', *, *, #104918, .T. ) ;
#115081 = ORIENTED_EDGE ( 'NONE', *, *, #58667, .T. ) ;
#115082 = CARTESIAN_POINT ( 'NONE',  ( 8.949999999999919353, 2.500000000000000000, 2.511473670974873507 ) ) ;
#115083 = FACE_BOUND ( 'NONE', #2031, .T. ) ;
#115084 = DIRECTION ( 'NONE',  ( 0.000000000000000000, 0.000000000000000000, 1.000000000000000000 ) ) ;
#115085 = EDGE_LOOP ( 'NONE', ( #29868, #73136, #78240, #88526 ) ) ;
#115086 = CARTESIAN_POINT ( 'NONE',  ( 81.97673105886440226, 3.779183627794353573, 6.223416391359812394 ) ) ;
#115087 = DIRECTION ( 'NONE',  ( 0.000000000000000000, -0.9999939076577903929, 0.003490651415223739937 ) ) ;
#115088 = ORIENTED_EDGE ( 'NONE', *, *, #18228, .T. ) ;
#115089 = DIRECTION ( 'NONE',  ( 0.000000000000000000, 1.000000000000000000, 0.000000000000000000 ) ) ;
#115090 = CARTESIAN_POINT ( 'NONE',  ( -1.450000000000035927, 12.50000000000000000, -1.818653347947326138 ) ) ;
#115091 = EDGE_CURVE ( 'NONE', #74901, #67778, #28027, .T. ) ;
#115092 = ORIENTED_EDGE ( 'NONE', *, *, #111637, .T. ) ;
#115093 = AXIS2_PLACEMENT_3D ( 'NONE', #95074, #115992, #6642 ) ;
#115094 = DIRECTION ( 'NONE',  ( 0.000000000000000000, 1.000000000000000000, 0.000000000000000000 ) ) ;
#115095 = VECTOR ( 'NONE', #128725, 1000.000000000000000 ) ;
#115096 = DIRECTION ( 'NONE',  ( -0.000000000000000000, 1.000000000000000000, -0.000000000000000000 ) ) ;
#115097 = ADVANCED_FACE ( 'NONE', ( #67939 ), #25789, .T. ) ;
#115098 = ORIENTED_EDGE ( 'NONE', *, *, #102451, .F. ) ;
#115099 = DIRECTION ( 'NONE',  ( -4.274815082592931898E-19, -0.9999939076577903929, -0.003490651415223739937 ) ) ;
#115100 = VECTOR ( 'NONE', #84484, 1000.000000000000000 ) ;
#115101 = DIRECTION ( 'NONE',  ( 0.000000000000000000, 0.000000000000000000, -1.000000000000000000 ) ) ;
#115102 = FACE_OUTER_BOUND ( 'NONE', #89416, .T. ) ;
#115103 = ORIENTED_EDGE ( 'NONE', *, *, #35881, .T. ) ;
#115105 = ADVANCED_FACE ( 'NONE', ( #117660 ), #741, .T. ) ;
#115104 = CONICAL_SURFACE ( 'NONE', #8506, 0.1000000000000002554, 0.003490658503988666988 ) ;
#115106 = ORIENTED_EDGE ( 'NONE', *, *, #51546, .F. ) ;
#115107 = ADVANCED_FACE ( 'NONE', ( #48307 ), #113618, .T. ) ;
#115108 = CARTESIAN_POINT ( 'NONE',  ( 8.549999999999918998, 12.50000000000000000, -1.753560074763288679 ) ) ;
#115109 = ORIENTED_EDGE ( 'NONE', *, *, #107055, .T. ) ;
#115110 = CARTESIAN_POINT ( 'NONE',  ( -5.850000000000022737, 2.500000000000000000, -6.595190528383302109 ) ) ;
#115111 = DIRECTION ( 'NONE',  ( -0.000000000000000000, 1.000000000000000000, -0.000000000000000000 ) ) ;
#115112 = VERTEX_POINT ( 'NONE', #39161 ) ;
#115113 = DIRECTION ( 'NONE',  ( 0.000000000000000000, 0.000000000000000000, 1.000000000000000000 ) ) ;
#115114 = LINE ( 'NONE', #124970, #110396 ) ;
#115115 = FACE_OUTER_BOUND ( 'NONE', #17184, .T. ) ;
#115116 = DIRECTION ( 'NONE',  ( 0.000000000000000000, 0.000000000000000000, -1.000000000000000000 ) ) ;
#115117 = ADVANCED_FACE ( 'NONE', ( #66645 ), #29321, .T. ) ;
#115118 = CARTESIAN_POINT ( 'NONE',  ( 108.0000000000000142, 8.500000000000000000, -0.2500000000000000000 ) ) ;
#115119 = ORIENTED_EDGE ( 'NONE', *, *, #121970, .F. ) ;
#115120 = ORIENTED_EDGE ( 'NONE', *, *, #50010, .T. ) ;
#115121 = LINE ( 'NONE', #105978, #3497 ) ;
#115122 = CARTESIAN_POINT ( 'NONE',  ( 10.39999999999991154, 12.50000000000000000, 3.637306695894644726 ) ) ;
#115123 = CARTESIAN_POINT ( 'NONE',  ( -4.150000000000027889, 12.50000000000000000, -7.188010851410854052 ) ) ;
#115125 = VERTEX_POINT ( 'NONE', #7070 ) ;
#115124 = VERTEX_POINT ( 'NONE', #106574 ) ;
#115126 = VERTEX_POINT ( 'NONE', #47033 ) ;
#115127 = DIRECTION ( 'NONE',  ( -0.000000000000000000, -1.000000000000000000, -0.000000000000000000 ) ) ;
#115128 = VECTOR ( 'NONE', #56901, 1000.000000000000000 ) ;
#115129 = DIRECTION ( 'NONE',  ( -0.000000000000000000, 1.000000000000000000, -0.000000000000000000 ) ) ;
#115130 = CONICAL_SURFACE ( 'NONE', #83849, 0.1000000000000000056, 0.003490658503988666988 ) ;
#115131 = DIRECTION ( 'NONE',  ( 0.000000000000000000, -0.9999939076577903929, 0.003490651415223739937 ) ) ;
#115132 = DIRECTION ( 'NONE',  ( 0.000000000000000000, 1.000000000000000000, 0.000000000000000000 ) ) ;
#115133 = DIRECTION ( 'NONE',  ( 0.000000000000000000, 1.000000000000000000, 0.000000000000000000 ) ) ;
#115134 = LINE ( 'NONE', #65413, #10977 ) ;
#115135 = CARTESIAN_POINT ( 'NONE',  ( -7.100000000000013856, 2.500000000000000000, 3.637306695894644726 ) ) ;
#115136 = CARTESIAN_POINT ( 'NONE',  ( 5.649999999999932854, 12.50000000000000000, 1.818653347947321475 ) ) ;
#115137 = DIRECTION ( 'NONE',  ( 0.000000000000000000, 1.000000000000000000, 0.000000000000000000 ) ) ;
#115138 = AXIS2_PLACEMENT_3D ( 'NONE', #113239, #63517, #103437 ) ;
#115139 = EDGE_LOOP ( 'NONE', ( #62479, #118445, #90380, #122303 ) ) ;
#115140 = EDGE_CURVE ( 'NONE', #948, #105841, #37214, .T. ) ;
#115141 = DIRECTION ( 'NONE',  ( 0.000000000000000000, 0.000000000000000000, -1.000000000000000000 ) ) ;
#115142 = VERTEX_POINT ( 'NONE', #29971 ) ;
#115143 = ORIENTED_EDGE ( 'NONE', *, *, #96294, .F. ) ;
#115144 = ADVANCED_FACE ( 'NONE', ( #59443 ), #44675, .T. ) ;
#115145 = CARTESIAN_POINT ( 'NONE',  ( 5.449999999999936229, 2.500000000000000000, 6.495190528383297135 ) ) ;
#115146 = CARTESIAN_POINT ( 'NONE',  ( -13.34999999999999076, 2.500000000000000000, -2.065063509461099844 ) ) ;
#115147 = CARTESIAN_POINT ( 'NONE',  ( 6.449999999999931788, 2.500000000000000000, 6.148780366869520009 ) ) ;
#115148 = EDGE_CURVE ( 'NONE', #68264, #47076, #60715, .T. ) ;
#115149 = VECTOR ( 'NONE', #3823, 1000.000000000000000 ) ;
#115150 = DIRECTION ( 'NONE',  ( 0.000000000000000000, 0.000000000000000000, 1.000000000000000000 ) ) ;
#115151 = AXIS2_PLACEMENT_3D ( 'NONE', #49585, #67911, #89493 ) ;
#115152 = DIRECTION ( 'NONE',  ( 0.000000000000000000, 0.000000000000000000, -1.000000000000000000 ) ) ;
#115153 = CARTESIAN_POINT ( 'NONE',  ( -8.750000000000008882, 12.50000000000000000, 1.472243186433545459 ) ) ;
#115154 = DIRECTION ( 'NONE',  ( 0.000000000000000000, 0.000000000000000000, 1.000000000000000000 ) ) ;
#115155 = ORIENTED_EDGE ( 'NONE', *, *, #75461, .F. ) ;
#115156 = CARTESIAN_POINT ( 'NONE',  ( 8.749999999999923617, 2.500000000000000000, -7.188010851410854052 ) ) ;
#115157 = ADVANCED_FACE ( 'NONE', ( #50250 ), #42538, .T. ) ;
#115158 = ADVANCED_FACE ( 'NONE', ( #91450 ), #13257, .T. ) ;
#115159 = EDGE_CURVE ( 'NONE', #94964, #53612, #69219, .T. ) ;
#115161 = ADVANCED_FACE ( 'NONE', ( #80993 ), #6985, .T. ) ;
#115160 = CONICAL_SURFACE ( 'NONE', #4431, 0.09999999999999982514, 0.003490658503988666988 ) ;
#115162 = CARTESIAN_POINT ( 'NONE',  ( 142.3152275665817115, 2.500000000000000000, 1.374601720185641973 ) ) ;
#115163 = ORIENTED_EDGE ( 'NONE', *, *, #31695, .T. ) ;
#115164 = EDGE_LOOP ( 'NONE', ( #71434, #118470, #41283, #100440 ) ) ;
#115165 = ADVANCED_FACE ( 'NONE', ( #20787 ), #38430, .T. ) ;
#115166 = CIRCLE ( 'NONE', #29524, 0.1000000000000002554 ) ;
#115167 = ORIENTED_EDGE ( 'NONE', *, *, #81644, .T. ) ;
#115168 = ORIENTED_EDGE ( 'NONE', *, *, #93178, .F. ) ;
#115169 = CARTESIAN_POINT ( 'NONE',  ( 3.949999999999942446, 12.50000000000000000, -2.511473670974877948 ) ) ;
#115170 = CARTESIAN_POINT ( 'NONE',  ( -11.84999999999999787, 12.50000000000000000, -2.511473670974873951 ) ) ;
#115171 = EDGE_CURVE ( 'NONE', #91471, #75085, #79695, .T. ) ;
#115172 = DIRECTION ( 'NONE',  ( 0.000000000000000000, 1.000000000000000000, 0.000000000000000000 ) ) ;
#115173 = CARTESIAN_POINT ( 'NONE',  ( -8.750000000000007105, 2.500000000000000000, 7.188010851410848723 ) ) ;
#115174 = CARTESIAN_POINT ( 'NONE',  ( -5.400000000000019895, 2.500000000000000000, -0.5928203230275541635 ) ) ;
#115175 = ORIENTED_EDGE ( 'NONE', *, *, #12200, .T. ) ;
#115176 = DIRECTION ( 'NONE',  ( 0.000000000000000000, 0.000000000000000000, -1.000000000000000000 ) ) ;
#115177 = DIRECTION ( 'NONE',  ( 0.000000000000000000, 1.000000000000000000, 0.000000000000000000 ) ) ;
#115178 = DIRECTION ( 'NONE',  ( -0.000000000000000000, 1.000000000000000000, -0.000000000000000000 ) ) ;
#115179 = EDGE_LOOP ( 'NONE', ( #86132, #122226, #26839, #16844 ) ) ;
#115180 = ORIENTED_EDGE ( 'NONE', *, *, #58411, .F. ) ;
#115181 = ORIENTED_EDGE ( 'NONE', *, *, #117636, .F. ) ;
#115182 = AXIS2_PLACEMENT_3D ( 'NONE', #24225, #64141, #104075 ) ;
#115183 = DIRECTION ( 'NONE',  ( 0.000000000000000000, -0.000000000000000000, 1.000000000000000000 ) ) ;
#115184 = VECTOR ( 'NONE', #14242, 1000.000000000000000 ) ;
#115185 = AXIS2_PLACEMENT_3D ( 'NONE', #106317, #4875, #86008 ) ;
#115186 = DIRECTION ( 'NONE',  ( 0.000000000000000000, 0.000000000000000000, 1.000000000000000000 ) ) ;
#115187 = DIRECTION ( 'NONE',  ( -0.000000000000000000, 1.000000000000000000, -0.000000000000000000 ) ) ;
#115188 = AXIS2_PLACEMENT_3D ( 'NONE', #34099, #12508, #72733 ) ;
#115189 = AXIS2_PLACEMENT_3D ( 'NONE', #114969, #105813, #3737 ) ;
#115191 = ORIENTED_EDGE ( 'NONE', *, *, #87515, .T. ) ;
#115190 = AXIS2_PLACEMENT_3D ( 'NONE', #103741, #115455, #123369 ) ;
#115192 = CARTESIAN_POINT ( 'NONE',  ( 12.09999999999990550, 2.500000000000000000, 3.537306695894645081 ) ) ;
#115193 = CARTESIAN_POINT ( 'NONE',  ( -10.65000000000000391, 2.500000000000000000, -1.818653347947322141 ) ) ;
#115194 = DIRECTION ( 'NONE',  ( 0.000000000000000000, -0.000000000000000000, 1.000000000000000000 ) ) ;
#115195 = FACE_OUTER_BOUND ( 'NONE', #49246, .T. ) ;
#115196 = CARTESIAN_POINT ( 'NONE',  ( 2.099999999999950351, 2.500000000000000000, 0.09999999999999772959 ) ) ;
#115197 = VERTEX_POINT ( 'NONE', #10929 ) ;
#115198 = DIRECTION ( 'NONE',  ( 0.000000000000000000, 1.000000000000000000, 0.000000000000000000 ) ) ;
#115199 = EDGE_CURVE ( 'NONE', #92765, #44902, #49617, .T. ) ;
#115200 = VERTEX_POINT ( 'NONE', #50892 ) ;
#115201 = VERTEX_POINT ( 'NONE', #89519 ) ;
#115202 = ORIENTED_EDGE ( 'NONE', *, *, #57135, .T. ) ;
#115203 = DIRECTION ( 'NONE',  ( 0.000000000000000000, -0.000000000000000000, 1.000000000000000000 ) ) ;
#115204 = FACE_BOUND ( 'NONE', #127965, .T. ) ;
#115205 = FACE_OUTER_BOUND ( 'NONE', #13057, .T. ) ;
#115206 = DIRECTION ( 'NONE',  ( -0.000000000000000000, -1.000000000000000000, -0.000000000000000000 ) ) ;
#115207 = CARTESIAN_POINT ( 'NONE',  ( -12.89999999999999325, 2.500000000000000000, 0.7928203230275536750 ) ) ;
#115208 = ADVANCED_FACE ( 'NONE', ( #111739 ), #69803, .T. ) ;
#115209 = EDGE_LOOP ( 'NONE', ( #125604, #32938, #42093, #29558 ) ) ;
#115210 = FACE_OUTER_BOUND ( 'NONE', #94390, .T. ) ;
#115211 = DIRECTION ( 'NONE',  ( -0.000000000000000000, -1.000000000000000000, -0.000000000000000000 ) ) ;
#115212 = DIRECTION ( 'NONE',  ( 0.000000000000000000, 0.000000000000000000, 1.000000000000000000 ) ) ;
#115213 = CARTESIAN_POINT ( 'NONE',  ( -7.100000000000013856, 2.500000000000000000, 5.022947341949748790 ) ) ;
#115214 = ORIENTED_EDGE ( 'NONE', *, *, #65642, .F. ) ;
#115215 = AXIS2_PLACEMENT_3D ( 'NONE', #99445, #569, #42460 ) ;
#115216 = FACE_OUTER_BOUND ( 'NONE', #18422, .T. ) ;
#115217 = VECTOR ( 'NONE', #80747, 1000.000000000000000 ) ;
#115218 = CARTESIAN_POINT ( 'NONE',  ( -5.200000000000025935, 2.500000000000000000, -3.983716857408426293 ) ) ;
#115219 = ORIENTED_EDGE ( 'NONE', *, *, #50196, .F. ) ;
#115220 = PLANE ( 'NONE',  #41868 ) ;
#115221 = EDGE_LOOP ( 'NONE', ( #117694, #42939, #108008, #47467 ) ) ;
#115222 = FACE_BOUND ( 'NONE', #116914, .T. ) ;
#115223 = DIRECTION ( 'NONE',  ( 0.000000000000000000, -0.9999939076577903929, 0.003490651415223739937 ) ) ;
#115224 = AXIS2_PLACEMENT_3D ( 'NONE', #109884, #87643, #37909 ) ;
#115225 = VERTEX_POINT ( 'NONE', #119615 ) ;
#115226 = DIRECTION ( 'NONE',  ( 0.000000000000000000, 0.000000000000000000, 1.000000000000000000 ) ) ;
#115227 = CARTESIAN_POINT ( 'NONE',  ( 2.899999999999944844, 2.500000000000000000, 3.537306695894645081 ) ) ;
#115228 = ORIENTED_EDGE ( 'NONE', *, *, #66677, .F. ) ;
#115229 = ORIENTED_EDGE ( 'NONE', *, *, #102393, .F. ) ;
#115230 = CARTESIAN_POINT ( 'NONE',  ( 185.2135416670080872, 4.367472073101518859, -7.564683531249999149 ) ) ;
#115231 = VERTEX_POINT ( 'NONE', #69886 ) ;
#115233 = CARTESIAN_POINT ( 'NONE',  ( 184.9218750003414016, 0.000000000000000000, 7.564683531250000925 ) ) ;
#115232 = VECTOR ( 'NONE', #69835, 1000.000000000000000 ) ;
#115234 = DIRECTION ( 'NONE',  ( 0.000000000000000000, 0.000000000000000000, 1.000000000000000000 ) ) ;
#115235 = CIRCLE ( 'NONE', #102655, 0.06509327318403745899 ) ;
#115236 = EDGE_CURVE ( 'NONE', #9888, #80502, #109809, .T. ) ;
#115237 = DIRECTION ( 'NONE',  ( -4.274815082592931898E-19, -0.9999939076577903929, -0.003490651415223739937 ) ) ;
#115238 = VECTOR ( 'NONE', #28616, 1000.000000000000000 ) ;
#115239 = FACE_OUTER_BOUND ( 'NONE', #120181, .T. ) ;
#115240 = CARTESIAN_POINT ( 'NONE',  ( -9.999999999999969802, 2.500000000000000000, 4.430127018922196847 ) ) ;
#115241 = AXIS2_PLACEMENT_3D ( 'NONE', #105092, #5595, #6238 ) ;
#115242 = ADVANCED_FACE ( 'NONE', ( #30622 ), #32266, .T. ) ;
#115243 = ORIENTED_EDGE ( 'NONE', *, *, #104113, .T. ) ;
#115244 = ORIENTED_EDGE ( 'NONE', *, *, #47334, .F. ) ;
#115245 = DIRECTION ( 'NONE',  ( -4.274815082592931898E-19, -0.9999939076577903929, -0.003490651415223739937 ) ) ;
#115246 = VECTOR ( 'NONE', #93076, 1000.000000000000000 ) ;
#115247 = AXIS2_PLACEMENT_3D ( 'NONE', #48206, #8909, #86170 ) ;
#115248 = DIRECTION ( 'NONE',  ( 0.000000000000000000, 0.000000000000000000, -1.000000000000000000 ) ) ;
#115249 = DIRECTION ( 'NONE',  ( -0.000000000000000000, 1.000000000000000000, -0.000000000000000000 ) ) ;
#115250 = CARTESIAN_POINT ( 'NONE',  ( 11.84999999999990372, 12.50000000000000000, -6.841600689897078702 ) ) ;
#115252 = VERTEX_POINT ( 'NONE', #90809 ) ;
#115251 = ORIENTED_EDGE ( 'NONE', *, *, #86845, .T. ) ;
#115253 = EDGE_CURVE ( 'NONE', #4247, #28898, #41093, .T. ) ;
#115254 = FACE_BOUND ( 'NONE', #49739, .T. ) ;
#115255 = ORIENTED_EDGE ( 'NONE', *, *, #93928, .T. ) ;
#115256 = EDGE_CURVE ( 'NONE', #11947, #64157, #48979, .T. ) ;
#115257 = DIRECTION ( 'NONE',  ( 0.000000000000000000, 0.000000000000000000, 1.000000000000000000 ) ) ;
#115258 = DIRECTION ( 'NONE',  ( -0.000000000000000000, -1.000000000000000000, -0.000000000000000000 ) ) ;
#115259 = ORIENTED_EDGE ( 'NONE', *, *, #102696, .F. ) ;
#115260 = DIRECTION ( 'NONE',  ( 0.000000000000000000, -0.000000000000000000, 1.000000000000000000 ) ) ;
#115261 = CARTESIAN_POINT ( 'NONE',  ( -10.40000000000000213, 2.500000000000000000, 3.637306695894644726 ) ) ;
#115262 = CARTESIAN_POINT ( 'NONE',  ( 7.499999999999925393, 2.500000000000000000, -3.737306695894649700 ) ) ;
#115263 = CARTESIAN_POINT ( 'NONE',  ( 12.89999999999990266, 2.500000000000000000, 3.537306695894645081 ) ) ;
#115264 = EDGE_CURVE ( 'NONE', #116433, #74234, #65591, .T. ) ;
#115265 = CARTESIAN_POINT ( 'NONE',  ( 185.7500000000000000, 9.429780353434619030E-16, -7.700000000000000178 ) ) ;
#115266 = CARTESIAN_POINT ( 'NONE',  ( 115.5000000000000000, 2.449293598294706414E-16, 2.000000000000000000 ) ) ;
#115267 = CARTESIAN_POINT ( 'NONE',  ( 186.7760416670080588, 6.551208109652274736, 3.782341765625001351 ) ) ;
#115268 = DIRECTION ( 'NONE',  ( -0.000000000000000000, -1.000000000000000000, -0.000000000000000000 ) ) ;
#115269 = ADVANCED_FACE ( 'NONE', ( #69653 ), #57278, .T. ) ;
#115270 = DIRECTION ( 'NONE',  ( -0.000000000000000000, 1.000000000000000000, -0.000000000000000000 ) ) ;
#115271 = VERTEX_POINT ( 'NONE', #78857 ) ;
#115272 = ORIENTED_EDGE ( 'NONE', *, *, #122252, .T. ) ;
#115273 = CARTESIAN_POINT ( 'NONE',  ( -0.6000000000000383915, 2.500000000000000000, -4.676537180435977881 ) ) ;
#115274 = ORIENTED_EDGE ( 'NONE', *, *, #11097, .T. ) ;
#115275 = CIRCLE ( 'NONE', #94455, 0.06509327318403745899 ) ;
#115276 = CARTESIAN_POINT ( 'NONE',  ( 7.899999999999924860, 12.50000000000000000, 5.022947341949748790 ) ) ;
#115277 = VECTOR ( 'NONE', #31818, 1000.000000000000000 ) ;
#115278 = AXIS2_PLACEMENT_3D ( 'NONE', #108734, #17773, #77991 ) ;
#115280 = VERTEX_POINT ( 'NONE', #29111 ) ;
#115279 = EDGE_LOOP ( 'NONE', ( #119979, #56370 ) ) ;
#115281 = ORIENTED_EDGE ( 'NONE', *, *, #47899, .T. ) ;
#115282 = CARTESIAN_POINT ( 'NONE',  ( -4.150000000000025224, 2.500000000000000000, 6.495190528383297135 ) ) ;
#115283 = CONICAL_SURFACE ( 'NONE', #10827, 0.09999999999999982514, 0.003490658503988666988 ) ;
#115284 = CARTESIAN_POINT ( 'NONE',  ( 6.649999999999928413, 12.50000000000000000, 2.857883832488649301 ) ) ;
#115285 = AXIS2_PLACEMENT_3D ( 'NONE', #18716, #49492, #87447 ) ;
#115286 =( LENGTH_UNIT ( ) NAMED_UNIT ( * ) SI_UNIT ( .MILLI., .METRE. ) );
#115287 = LINE ( 'NONE', #15818, #47294 ) ;
#115288 = CARTESIAN_POINT ( 'NONE',  ( -11.84999999999999609, 2.500000000000000000, 2.511473670974873507 ) ) ;
#115289 = AXIS2_PLACEMENT_3D ( 'NONE', #37707, #27880, #67801 ) ;
#115290 = CARTESIAN_POINT ( 'NONE',  ( 179.5000000000000000, 0.6250000000000028866, -7.634788798650556707 ) ) ;
#115291 = ORIENTED_EDGE ( 'NONE', *, *, #116470, .F. ) ;
#115292 = CARTESIAN_POINT ( 'NONE',  ( -6.650000000000015454, 2.500000000000000000, 2.757883832488649656 ) ) ;
#115294 = ORIENTED_EDGE ( 'NONE', *, *, #60971, .F. ) ;
#115293 = AXIS2_PLACEMENT_3D ( 'NONE', #95955, #43653, #83574 ) ;
#115295 = ORIENTED_EDGE ( 'NONE', *, *, #28056, .F. ) ;
#115296 = VERTEX_POINT ( 'NONE', #8147 ) ;
#115297 = VERTEX_POINT ( 'NONE', #57265 ) ;
#115298 = CARTESIAN_POINT ( 'NONE',  ( -0.8000000000000315747, 2.500000000000000000, 0.000000000000000000 ) ) ;
#115299 = ORIENTED_EDGE ( 'NONE', *, *, #94102, .T. ) ;
#115300 = VERTEX_POINT ( 'NONE', #9455 ) ;
#115301 = FACE_OUTER_BOUND ( 'NONE', #68284, .T. ) ;
#115302 = CARTESIAN_POINT ( 'NONE',  ( 185.0000000000000000, 0.000000000000000000, 7.700000000000000178 ) ) ;
#115303 = DIRECTION ( 'NONE',  ( -0.000000000000000000, 1.000000000000000000, -0.000000000000000000 ) ) ;
#115304 = CARTESIAN_POINT ( 'NONE',  ( 2.049999999999950084, 12.50000000000000000, -6.495190528383302464 ) ) ;
#115305 = FACE_OUTER_BOUND ( 'NONE', #20652, .T. ) ;
#115306 = EDGE_CURVE ( 'NONE', #111256, #109372, #106986, .T. ) ;
#115307 = FACE_OUTER_BOUND ( 'NONE', #100863, .T. ) ;
#115308 = EDGE_LOOP ( 'NONE', ( #102558, #127293, #123723, #99003 ) ) ;
#115309 = EDGE_CURVE ( 'NONE', #54837, #123253, #87985, .T. ) ;
#115310 = EDGE_CURVE ( 'NONE', #122488, #37002, #59360, .T. ) ;
#115311 = FACE_OUTER_BOUND ( 'NONE', #119654, .T. ) ;
#115312 = ADVANCED_FACE ( 'NONE', ( #17971 ), #2906, .T. ) ;
#115313 = AXIS2_PLACEMENT_3D ( 'NONE', #69305, #109232, #101369 ) ;
#115314 = AXIS2_PLACEMENT_3D ( 'NONE', #9264, #28260, #100221 ) ;
#115315 = EDGE_LOOP ( 'NONE', ( #117012, #43035 ) ) ;
#115316 = CARTESIAN_POINT ( 'NONE',  ( -3.350000000000028511, 12.50000000000000000, -2.792790559304616504 ) ) ;
#115317 = ORIENTED_EDGE ( 'NONE', *, *, #99876, .F. ) ;
#115318 = CARTESIAN_POINT ( 'NONE',  ( -4.150000000000025224, 12.50000000000000000, 2.857883832488649301 ) ) ;
#115319 = ADVANCED_FACE ( 'NONE', ( #108288 ), #61502, .T. ) ;
#115320 = ORIENTED_EDGE ( 'NONE', *, *, #31233, .T. ) ;
#115321 = EDGE_LOOP ( 'NONE', ( #34368, #103575 ) ) ;
#115322 = CONICAL_SURFACE ( 'NONE', #121697, 0.1000000000000002554, 0.003490658503988666988 ) ;
#115323 = CARTESIAN_POINT ( 'NONE',  ( 10.44999999999991402, 12.50000000000000000, 6.560283801567334372 ) ) ;
#115324 = DIRECTION ( 'NONE',  ( 0.000000000000000000, 0.000000000000000000, 1.000000000000000000 ) ) ;
#115325 = CONICAL_SURFACE ( 'NONE', #44338, 0.1000000000000000472, 0.003490658503988666988 ) ;
#115326 = EDGE_CURVE ( 'NONE', #36772, #121481, #9159, .T. ) ;
#115327 = VECTOR ( 'NONE', #87171, 1000.000000000000000 ) ;
#115328 = ADVANCED_FACE ( 'NONE', ( #96515 ), #37635, .T. ) ;
#115329 = CARTESIAN_POINT ( 'NONE',  ( 12.29999999999990301, 12.50000000000000000, -0.3464101615137782364 ) ) ;
#115330 = AXIS2_PLACEMENT_3D ( 'NONE', #97973, #86862, #8938 ) ;
#115331 = AXIS2_PLACEMENT_3D ( 'NONE', #51882, #91797, #42058 ) ;
#115332 = CARTESIAN_POINT ( 'NONE',  ( 1.649999999999948841, 2.500000000000000000, 6.495190528383297135 ) ) ;
#115333 = CARTESIAN_POINT ( 'NONE',  ( -10.40000000000000213, 12.50000000000000000, 0.06509327318403515528 ) ) ;
#115334 = EDGE_LOOP ( 'NONE', ( #67804, #9772 ) ) ;
#115335 = DIRECTION ( 'NONE',  ( 0.000000000000000000, 1.000000000000000000, 0.000000000000000000 ) ) ;
#115336 = FACE_OUTER_BOUND ( 'NONE', #52882, .T. ) ;
#115337 = CARTESIAN_POINT ( 'NONE',  ( 4.399999999999940847, 2.500000000000000000, -4.776537180435977525 ) ) ;
#115338 = DIRECTION ( 'NONE',  ( 0.000000000000000000, 0.000000000000000000, -1.000000000000000000 ) ) ;
#115339 = EDGE_CURVE ( 'NONE', #66080, #97447, #76901, .T. ) ;
#115340 = AXIS2_PLACEMENT_3D ( 'NONE', #108164, #66311, #58448 ) ;
#115341 = FACE_OUTER_BOUND ( 'NONE', #117491, .T. ) ;
#115342 = ORIENTED_EDGE ( 'NONE', *, *, #100296, .F. ) ;
#115343 = AXIS2_PLACEMENT_3D ( 'NONE', #60394, #797, #28342 ) ;
#115344 = CIRCLE ( 'NONE', #46403, 0.1000000000000000056 ) ;
#115345 = AXIS2_PLACEMENT_3D ( 'NONE', #105798, #63290, #92766 ) ;
#115346 = VERTEX_POINT ( 'NONE', #46804 ) ;
#115347 = CIRCLE ( 'NONE', #40071, 0.1000000000000002554 ) ;
#115348 = ORIENTED_EDGE ( 'NONE', *, *, #65088, .T. ) ;
#115349 = DIRECTION ( 'NONE',  ( -4.274815082592931898E-19, -0.9999939076577903929, -0.003490651415223739937 ) ) ;
#115350 = DIRECTION ( 'NONE',  ( 0.000000000000000000, 0.000000000000000000, 1.000000000000000000 ) ) ;
#115351 = CARTESIAN_POINT ( 'NONE',  ( 185.0052083336747444, -6.551208109652278289, 3.782341765624995134 ) ) ;
#115352 = DIRECTION ( 'NONE',  ( 0.000000000000000000, -0.000000000000000000, 1.000000000000000000 ) ) ;
#115353 = DIRECTION ( 'NONE',  ( -0.000000000000000000, 1.000000000000000000, -0.000000000000000000 ) ) ;
#115354 = DIRECTION ( 'NONE',  ( 0.000000000000000000, 0.000000000000000000, 1.000000000000000000 ) ) ;
#115355 = DIRECTION ( 'NONE',  ( 0.000000000000000000, 0.000000000000000000, 1.000000000000000000 ) ) ;
#115356 = ORIENTED_EDGE ( 'NONE', *, *, #53163, .T. ) ;
#115357 = DIRECTION ( 'NONE',  ( -4.274815082592931898E-19, -0.9999939076577903929, -0.003490651415223739937 ) ) ;
#115358 = CARTESIAN_POINT ( 'NONE',  ( -13.34999999999999076, 2.500000000000000000, -2.857883832488651521 ) ) ;
#115359 = EDGE_LOOP ( 'NONE', ( #79063, #53062 ) ) ;
#115360 = DIRECTION ( 'NONE',  ( 0.000000000000000000, -1.000000000000000000, 0.000000000000000000 ) ) ;
#115361 = CARTESIAN_POINT ( 'NONE',  ( 14.54999999999989591, 2.500000000000000000, 2.165063509461097713 ) ) ;
#115362 = CARTESIAN_POINT ( 'NONE',  ( 14.34999999999989306, 12.50000000000000000, -1.818653347947326138 ) ) ;
#115363 = EDGE_CURVE ( 'NONE', #92822, #13065, #53078, .T. ) ;
#115364 = ORIENTED_EDGE ( 'NONE', *, *, #115766, .T. ) ;
#115365 = CARTESIAN_POINT ( 'NONE',  ( 3.349999999999944578, 12.50000000000000000, -1.472243186433550122 ) ) ;
#115366 = CONICAL_SURFACE ( 'NONE', #21396, 0.1000000000000000472, 0.003490658503988666988 ) ;
#115367 = AXIS2_PLACEMENT_3D ( 'NONE', #97681, #45380, #66919 ) ;
#115368 = CONICAL_SURFACE ( 'NONE', #23459, 0.1000000000000002554, 0.003490658503988666988 ) ;
#115369 = EDGE_LOOP ( 'NONE', ( #24894, #90111 ) ) ;
#115370 = DIRECTION ( 'NONE',  ( 0.000000000000000000, 0.000000000000000000, 1.000000000000000000 ) ) ;
#115371 = DIRECTION ( 'NONE',  ( -0.000000000000000000, 1.000000000000000000, -0.000000000000000000 ) ) ;
#115372 = EDGE_LOOP ( 'NONE', ( #2947, #116738, #14972, #109754 ) ) ;
#115374 = PLANE ( 'NONE',  #105368 ) ;
#115373 = AXIS2_PLACEMENT_3D ( 'NONE', #13967, #53910, #72907 ) ;
#115375 = AXIS2_PLACEMENT_3D ( 'NONE', #56905, #7816, #66094 ) ;
#115376 = AXIS2_PLACEMENT_3D ( 'NONE', #89398, #8245, #39040 ) ;
#115377 = DIRECTION ( 'NONE',  ( 0.000000000000000000, 0.000000000000000000, -1.000000000000000000 ) ) ;
#115378 = AXIS2_PLACEMENT_3D ( 'NONE', #38877, #117362, #118680 ) ;
#115379 = AXIS2_PLACEMENT_3D ( 'NONE', #23141, #123280, #42143 ) ;
#115380 = VERTEX_POINT ( 'NONE', #77534 ) ;
#115381 = CONICAL_SURFACE ( 'NONE', #90363, 0.09999999999999982514, 0.003490658503988666988 ) ;
#115382 = DIRECTION ( 'NONE',  ( -0.000000000000000000, 1.000000000000000000, -0.000000000000000000 ) ) ;
#115383 = ORIENTED_EDGE ( 'NONE', *, *, #93067, .T. ) ;
#115384 = ORIENTED_EDGE ( 'NONE', *, *, #82356, .F. ) ;
#115385 = FACE_OUTER_BOUND ( 'NONE', #71013, .T. ) ;
#115386 = CARTESIAN_POINT ( 'NONE',  ( 9.599999999999917932, 12.50000000000000000, -2.276824562219559311E-15 ) ) ;
#115387 = EDGE_LOOP ( 'NONE', ( #77019, #68892, #27168, #48781 ) ) ;
#115388 = EDGE_CURVE ( 'NONE', #3164, #22492, #128612, .T. ) ;
#115389 = DIRECTION ( 'NONE',  ( -4.274815082592931898E-19, -0.9999939076577903929, -0.003490651415223739937 ) ) ;
#115390 = CARTESIAN_POINT ( 'NONE',  ( -8.300000000000011369, 2.500000000000000000, -2.276824562219559311E-15 ) ) ;
#115391 = ORIENTED_EDGE ( 'NONE', *, *, #72991, .T. ) ;
#115392 = CARTESIAN_POINT ( 'NONE',  ( -13.74999999999998934, 12.50000000000000000, -1.472243186433547901 ) ) ;
#115393 = CARTESIAN_POINT ( 'NONE',  ( 11.04999999999990656, 2.500000000000000000, 2.611473670974873151 ) ) ;
#115394 = DIRECTION ( 'NONE',  ( 0.000000000000000000, 1.000000000000000000, 0.000000000000000000 ) ) ;
#115395 = LINE ( 'NONE', #25112, #50872 ) ;
#115396 = CARTESIAN_POINT ( 'NONE',  ( -13.09999999999999076, 2.500000000000000000, 4.676537180435972552 ) ) ;
#115397 = CARTESIAN_POINT ( 'NONE',  ( 185.2812500006828031, 0.000000000000000000, 7.700000000000000178 ) ) ;
#115398 = AXIS2_PLACEMENT_3D ( 'NONE', #3646, #62583, #63863 ) ;
#115399 = EDGE_CURVE ( 'NONE', #39135, #113969, #82333, .T. ) ;
#115400 = ORIENTED_EDGE ( 'NONE', *, *, #18974, .F. ) ;
#115401 = ORIENTED_EDGE ( 'NONE', *, *, #94095, .F. ) ;
#115402 = ORIENTED_EDGE ( 'NONE', *, *, #62445, .T. ) ;
#115403 = ORIENTED_EDGE ( 'NONE', *, *, #128649, .T. ) ;
#115404 = CARTESIAN_POINT ( 'NONE',  ( 11.04999999999990834, 2.500000000000000000, -6.941600689897077459 ) ) ;
#115405 = CARTESIAN_POINT ( 'NONE',  ( -4.200000000000025935, 2.500000000000000000, 0.09999999999999761857 ) ) ;
#115406 = CARTESIAN_POINT ( 'NONE',  ( -5.400000000000019895, 2.500000000000000000, -0.5928203230275541635 ) ) ;
#115407 = ORIENTED_EDGE ( 'NONE', *, *, #111064, .F. ) ;
#115408 = EDGE_CURVE ( 'NONE', #62336, #21966, #17300, .T. ) ;
#115409 = FACE_BOUND ( 'NONE', #43114, .T. ) ;
#115410 = VECTOR ( 'NONE', #12824, 1000.000000000000000 ) ;
#115411 = EDGE_CURVE ( 'NONE', #91335, #115443, #71964, .T. ) ;
#115412 = DIRECTION ( 'NONE',  ( 0.000000000000000000, -0.9999939076577903929, 0.003490651415223739937 ) ) ;
#115413 = LINE ( 'NONE', #17209, #35450 ) ;
#115414 = AXIS2_PLACEMENT_3D ( 'NONE', #17930, #48693, #19201 ) ;
#115416 = DIRECTION ( 'NONE',  ( 0.000000000000000000, 0.000000000000000000, 1.000000000000000000 ) ) ;
#115415 = CONICAL_SURFACE ( 'NONE', #8816, 0.1000000000000002554, 0.003490658503988666988 ) ;
#115417 = AXIS2_PLACEMENT_3D ( 'NONE', #103780, #44874, #54656 ) ;
#115418 = DIRECTION ( 'NONE',  ( 0.000000000000000000, 0.000000000000000000, -1.000000000000000000 ) ) ;
#115419 = CARTESIAN_POINT ( 'NONE',  ( 7.499999999999925393, 2.500000000000000000, 5.122947341949749323 ) ) ;
#115420 = EDGE_CURVE ( 'NONE', #122603, #114300, #87346, .T. ) ;
#115421 = DIRECTION ( 'NONE',  ( 0.000000000000000000, 0.000000000000000000, 1.000000000000000000 ) ) ;
#115422 = EDGE_CURVE ( 'NONE', #79598, #9494, #25882, .T. ) ;
#115423 = CARTESIAN_POINT ( 'NONE',  ( 1.649999999999951505, 2.500000000000000000, -1.472243186433550122 ) ) ;
#115424 = CARTESIAN_POINT ( 'NONE',  ( 3.749999999999975131, 2.500000000000000000, 6.595190528383296780 ) ) ;
#115425 = ADVANCED_FACE ( 'NONE', ( #80126 ), #61129, .T. ) ;
#115426 = DIRECTION ( 'NONE',  ( -0.000000000000000000, -1.000000000000000000, -0.000000000000000000 ) ) ;
#115427 = EDGE_CURVE ( 'NONE', #18575, #49224, #92796, .T. ) ;
#115428 = EDGE_CURVE ( 'NONE', #106677, #14404, #88670, .T. ) ;
#115429 = DIRECTION ( 'NONE',  ( -0.000000000000000000, -1.000000000000000000, -0.000000000000000000 ) ) ;
#115430 = VECTOR ( 'NONE', #54403, 1000.000000000000000 ) ;
#115431 = ORIENTED_EDGE ( 'NONE', *, *, #541, .F. ) ;
#115432 = ORIENTED_EDGE ( 'NONE', *, *, #17478, .T. ) ;
#115433 = ORIENTED_EDGE ( 'NONE', *, *, #110417, .F. ) ;
#115435 = ORIENTED_EDGE ( 'NONE', *, *, #25517, .F. ) ;
#115434 = VECTOR ( 'NONE', #28733, 1000.000000000000000 ) ;
#115436 = AXIS2_PLACEMENT_3D ( 'NONE', #95544, #73306, #4540 ) ;
#115437 = AXIS2_PLACEMENT_3D ( 'NONE', #122558, #13870, #44000 ) ;
#115438 = DIRECTION ( 'NONE',  ( 0.000000000000000000, 0.000000000000000000, -1.000000000000000000 ) ) ;
#115439 = EDGE_LOOP ( 'NONE', ( #64030, #100649 ) ) ;
#115440 = DIRECTION ( 'NONE',  ( -0.000000000000000000, 1.000000000000000000, -0.000000000000000000 ) ) ;
#115441 = ORIENTED_EDGE ( 'NONE', *, *, #74111, .T. ) ;
#115442 = EDGE_CURVE ( 'NONE', #10889, #104716, #22515, .T. ) ;
#115443 = VERTEX_POINT ( 'NONE', #42809 ) ;
#115444 = AXIS2_PLACEMENT_3D ( 'NONE', #127029, #33644, #97546 ) ;
#115445 = CARTESIAN_POINT ( 'NONE',  ( 0.5999999999999547917, 12.50000000000000000, 3.983716857408420076 ) ) ;
#115446 = AXIS2_PLACEMENT_3D ( 'NONE', #100158, #50397, #123636 ) ;
#115447 = CARTESIAN_POINT ( 'NONE',  ( 0.1999999999999567124, 2.500000000000000000, -3.883716857408426648 ) ) ;
#115448 = DIRECTION ( 'NONE',  ( 1.000000000000000000, 0.000000000000000000, 0.000000000000000000 ) ) ;
#115449 = CARTESIAN_POINT ( 'NONE',  ( -2.700000000000029932, 2.500000000000000000, -0.2464101615137782308 ) ) ;
#115450 = DIRECTION ( 'NONE',  ( -4.274815082592931898E-19, -0.9999939076577903929, -0.003490651415223739937 ) ) ;
#115451 = EDGE_LOOP ( 'NONE', ( #71831, #12497 ) ) ;
#115452 = ORIENTED_EDGE ( 'NONE', *, *, #54434, .T. ) ;
#115453 = ORIENTED_EDGE ( 'NONE', *, *, #117137, .T. ) ;
#115454 = EDGE_LOOP ( 'NONE', ( #114519, #69620 ) ) ;
#115455 = DIRECTION ( 'NONE',  ( -0.000000000000000000, -1.000000000000000000, -0.000000000000000000 ) ) ;
#115456 = CIRCLE ( 'NONE', #7081, 0.06509327318403745899 ) ;
#115457 = ORIENTED_EDGE ( 'NONE', *, *, #59026, .F. ) ;
#115458 = ORIENTED_EDGE ( 'NONE', *, *, #124328, .T. ) ;
#115459 = CARTESIAN_POINT ( 'NONE',  ( -9.350000000000006750, 2.500000000000000000, -2.611473670974877592 ) ) ;
#115460 = PLANE ( 'NONE',  #89373 ) ;
#115461 = LINE ( 'NONE', #75555, #62537 ) ;
#115463 = CARTESIAN_POINT ( 'NONE',  ( -8.350000000000012079, 12.50000000000000000, 1.472243186433545459 ) ) ;
#115462 = VECTOR ( 'NONE', #94483, 1000.000000000000000 ) ;
#115464 = CIRCLE ( 'NONE', #31874, 0.1000000000000002554 ) ;
#115465 = VECTOR ( 'NONE', #103441, 1000.000000000000000 ) ;
#115466 = CARTESIAN_POINT ( 'NONE',  ( -11.64999999999999680, 12.50000000000000000, 5.802370205355744659 ) ) ;
#115467 = CARTESIAN_POINT ( 'NONE',  ( -5.650000000000023448, 2.500000000000000000, -1.918653347947326004 ) ) ;
#115468 = ADVANCED_FACE ( 'NONE', ( #122630 ), #10094, .T. ) ;
#115469 = EDGE_LOOP ( 'NONE', ( #4410, #59881 ) ) ;
#115470 = ADVANCED_FACE ( 'NONE', ( #51333 ), #50048, .T. ) ;
#115471 = CARTESIAN_POINT ( 'NONE',  ( 4.149999999999941735, 2.500000000000000000, -7.088010851410853519 ) ) ;
#115472 = VECTOR ( 'NONE', #4545, 1000.000000000000000 ) ;
#115474 = ORIENTED_EDGE ( 'NONE', *, *, #34554, .T. ) ;
#115473 = AXIS2_PLACEMENT_3D ( 'NONE', #58237, #39253, #49061 ) ;
#115476 = ADVANCED_FACE ( 'NONE', ( #72255 ), #113718, .T. ) ;
#115475 = CARTESIAN_POINT ( 'NONE',  ( -0.8500000000000386136, 2.500000000000000000, 5.802370205355744659 ) ) ;
#115477 = CONICAL_SURFACE ( 'NONE', #23472, 0.09999999999999982514, 0.003490658503988666988 ) ;
#115478 = ORIENTED_EDGE ( 'NONE', *, *, #80608, .T. ) ;
#115479 = DIRECTION ( 'NONE',  ( 0.000000000000000000, 1.000000000000000000, 0.000000000000000000 ) ) ;
#115480 = FACE_OUTER_BOUND ( 'NONE', #103999, .T. ) ;
#115481 = AXIS2_PLACEMENT_3D ( 'NONE', #126259, #117059, #113372 ) ;
#115482 = EDGE_LOOP ( 'NONE', ( #122857, #25105, #14328, #20534 ) ) ;
#115483 = AXIS2_PLACEMENT_3D ( 'NONE', #78485, #118378, #28729 ) ;
#115484 = DIRECTION ( 'NONE',  ( -0.000000000000000000, 1.000000000000000000, -0.000000000000000000 ) ) ;
#115485 = EDGE_CURVE ( 'NONE', #70366, #93927, #32976, .T. ) ;
#115486 = PLANE ( 'NONE',  #22787 ) ;
#115487 = EDGE_LOOP ( 'NONE', ( #63206, #87385, #27455, #60055 ) ) ;
#115488 = AXIS2_PLACEMENT_3D ( 'NONE', #59357, #67182, #109051 ) ;
#115489 = EDGE_CURVE ( 'NONE', #69025, #90022, #102351, .T. ) ;
#115490 = DIRECTION ( 'NONE',  ( -0.000000000000000000, -1.000000000000000000, -0.000000000000000000 ) ) ;
#115491 = ADVANCED_FACE ( 'NONE', ( #2191 ), #257, .T. ) ;
#115492 = ADVANCED_FACE ( 'NONE', ( #89933 ), #30111, .T. ) ;
#115493 = CARTESIAN_POINT ( 'NONE',  ( 13.29999999999990301, 12.50000000000000000, -4.330127018922201643 ) ) ;
#115494 = ORIENTED_EDGE ( 'NONE', *, *, #92577, .T. ) ;
#115495 = ORIENTED_EDGE ( 'NONE', *, *, #84163, .T. ) ;
#115496 = DIRECTION ( 'NONE',  ( 0.000000000000000000, 0.000000000000000000, -1.000000000000000000 ) ) ;
#115497 = CARTESIAN_POINT ( 'NONE',  ( 6.849999999999927702, 12.50000000000000000, 1.818653347947321475 ) ) ;
#115498 = CARTESIAN_POINT ( 'NONE',  ( 184.1093750003413732, 9.264065473108010111E-16, -7.564683531250000925 ) ) ;
#115499 = CARTESIAN_POINT ( 'NONE',  ( 133.2169897921533845, 2.500000000000000000, -2.337293474289257933 ) ) ;
#115500 = EDGE_CURVE ( 'NONE', #52365, #96763, #107451, .T. ) ;
#115501 = AXIS2_PLACEMENT_3D ( 'NONE', #19268, #940, #40893 ) ;
#115502 = DIRECTION ( 'NONE',  ( 0.000000000000000000, 0.000000000000000000, 1.000000000000000000 ) ) ;
#115503 = CARTESIAN_POINT ( 'NONE',  ( -1.650000000000034328, 2.500000000000000000, -7.088010851410853519 ) ) ;
#115504 = AXIS2_PLACEMENT_3D ( 'NONE', #7506, #15378, #46805 ) ;
#115505 = ORIENTED_EDGE ( 'NONE', *, *, #17863, .T. ) ;
#115506 = AXIS2_PLACEMENT_3D ( 'NONE', #55381, #27196, #26566 ) ;
#115507 = CARTESIAN_POINT ( 'NONE',  ( -8.550000000000007816, 2.500000000000000000, 6.248780366869520542 ) ) ;
#115508 = AXIS2_PLACEMENT_3D ( 'NONE', #44613, #55076, #96268 ) ;
#115509 = ORIENTED_EDGE ( 'NONE', *, *, #76204, .T. ) ;
#115510 = PLANE ( 'NONE',  #7832 ) ;
#115511 = EDGE_CURVE ( 'NONE', #37234, #38808, #82047, .T. ) ;
#115512 = DIRECTION ( 'NONE',  ( -0.000000000000000000, -1.000000000000000000, -0.000000000000000000 ) ) ;
#115513 = CARTESIAN_POINT ( 'NONE',  ( -3.749999999999991562, 12.50000000000000000, 6.495190528383297135 ) ) ;
#115514 = CIRCLE ( 'NONE', #42293, 0.1000000000000002554 ) ;
#115515 = AXIS2_PLACEMENT_3D ( 'NONE', #18259, #58837, #45966 ) ;
#115516 = EDGE_LOOP ( 'NONE', ( #123212, #45958 ) ) ;
#115517 = CIRCLE ( 'NONE', #109168, 0.1000000000000002554 ) ;
#115518 = CIRCLE ( 'NONE', #123845, 0.06509327318403745899 ) ;
#115519 = CARTESIAN_POINT ( 'NONE',  ( 3.099999999999943245, 12.50000000000000000, 4.048810130592458201 ) ) ;
#115520 = CARTESIAN_POINT ( 'NONE',  ( -3.550000000000027356, 2.500000000000000000, -2.611473670974877592 ) ) ;
#115521 = AXIS2_PLACEMENT_3D ( 'NONE', #95603, #5906, #49101 ) ;
#115522 = ORIENTED_EDGE ( 'NONE', *, *, #44030, .T. ) ;
#115524 = AXIS2_PLACEMENT_3D ( 'NONE', #108661, #10460, #68740 ) ;
#115523 = PLANE ( 'NONE',  #32216 ) ;
#115525 = EDGE_CURVE ( 'NONE', #67710, #104178, #103254, .T. ) ;
#115526 = EDGE_LOOP ( 'NONE', ( #75928, #121548 ) ) ;
#115527 = AXIS2_PLACEMENT_3D ( 'NONE', #59505, #99407, #70578 ) ;
#115529 = VERTEX_POINT ( 'NONE', #52591 ) ;
#115528 = VECTOR ( 'NONE', #3620, 1000.000000000000000 ) ;
#115530 = AXIS2_PLACEMENT_3D ( 'NONE', #13051, #60889, #100797 ) ;
#115531 = CARTESIAN_POINT ( 'NONE',  ( 14.39999999999989555, 12.50000000000000000, -0.3464101615137782364 ) ) ;
#115533 = EDGE_LOOP ( 'NONE', ( #56599, #23680 ) ) ;
#115532 = AXIS2_PLACEMENT_3D ( 'NONE', #74539, #65345, #37834 ) ;
#115534 = CARTESIAN_POINT ( 'NONE',  ( -13.74999999999998757, 12.50000000000000000, 1.537336459617586915 ) ) ;
#115535 = CARTESIAN_POINT ( 'NONE',  ( -0.8500000000000395017, 12.50000000000000000, 6.430097255199259010 ) ) ;
#115536 = DIRECTION ( 'NONE',  ( 0.000000000000000000, 1.000000000000000000, 0.000000000000000000 ) ) ;
#115537 = ORIENTED_EDGE ( 'NONE', *, *, #63871, .F. ) ;
#115538 = FACE_BOUND ( 'NONE', #11946, .T. ) ;
#115540 = ORIENTED_EDGE ( 'NONE', *, *, #97026, .F. ) ;
#115539 = DIRECTION ( 'NONE',  ( -0.000000000000000000, 1.000000000000000000, -0.000000000000000000 ) ) ;
#115541 = LINE ( 'NONE', #63888, #29761 ) ;
#115542 = EDGE_CURVE ( 'NONE', #86677, #46500, #30406, .T. ) ;
#115543 = CARTESIAN_POINT ( 'NONE',  ( -0.2000000000000347888, 2.500000000000000000, 0.4464101615137758272 ) ) ;
#115544 = ORIENTED_EDGE ( 'NONE', *, *, #83711, .F. ) ;
#115545 = EDGE_LOOP ( 'NONE', ( #73564, #105849, #61834, #40883 ) ) ;
#115546 = ORIENTED_EDGE ( 'NONE', *, *, #110600, .T. ) ;
#115547 = DIRECTION ( 'NONE',  ( -0.000000000000000000, -1.000000000000000000, -0.000000000000000000 ) ) ;
#115548 = DIRECTION ( 'NONE',  ( -0.000000000000000000, -1.000000000000000000, -0.000000000000000000 ) ) ;
#115550 = DIRECTION ( 'NONE',  ( 0.000000000000000000, 0.000000000000000000, 1.000000000000000000 ) ) ;
#115549 = CONICAL_SURFACE ( 'NONE', #67527, 0.1000000000000002554, 0.003490658503988666988 ) ;
#115551 = AXIS2_PLACEMENT_3D ( 'NONE', #83180, #94267, #94921 ) ;
#115552 = FACE_BOUND ( 'NONE', #32717, .T. ) ;
#115553 = ORIENTED_EDGE ( 'NONE', *, *, #102627, .T. ) ;
#115554 = CARTESIAN_POINT ( 'NONE',  ( 185.0677083336747160, -4.367472073101514418, -7.564683531250002702 ) ) ;
#115555 = CARTESIAN_POINT ( 'NONE',  ( 97.50000000000000000, 9.184850993605147944E-16, -7.500000000000000000 ) ) ;
#115556 = CARTESIAN_POINT ( 'NONE',  ( 7.099999999999928590, 12.50000000000000000, 4.330127018922196314 ) ) ;
#115558 = FACE_OUTER_BOUND ( 'NONE', #122075, .T. ) ;
#115557 = AXIS2_PLACEMENT_3D ( 'NONE', #118930, #57438, #97354 ) ;
#115559 = AXIS2_PLACEMENT_3D ( 'NONE', #58297, #18986, #98200 ) ;
#115560 = AXIS2_PLACEMENT_3D ( 'NONE', #35941, #75851, #107898 ) ;
#115562 = VECTOR ( 'NONE', #106964, 1000.000000000000000 ) ;
#115561 = LINE ( 'NONE', #6888, #27637 ) ;
#115563 = CARTESIAN_POINT ( 'NONE',  ( -6.700000000000019718, 12.50000000000000000, -4.265033745738164406 ) ) ;
#115564 = DIRECTION ( 'NONE',  ( 0.000000000000000000, -0.9999939076577903929, 0.003490651415223739937 ) ) ;
#115565 = CARTESIAN_POINT ( 'NONE',  ( -2.100000000000033396, 2.500000000000000000, 0.6928203230275494784 ) ) ;
#115566 = CONICAL_SURFACE ( 'NONE', #17365, 0.09999999999999982514, 0.003490658503988666988 ) ;
#115568 = FACE_OUTER_BOUND ( 'NONE', #69697, .T. ) ;
#115567 = AXIS2_PLACEMENT_3D ( 'NONE', #117595, #9605, #79014 ) ;
#115570 = EDGE_CURVE ( 'NONE', #77506, #70902, #15590, .T. ) ;
#115569 = CONICAL_SURFACE ( 'NONE', #94649, 0.09999999999999982514, 0.003490658503988666988 ) ;
#115571 = ORIENTED_EDGE ( 'NONE', *, *, #43973, .F. ) ;
#115572 = VERTEX_POINT ( 'NONE', #71591 ) ;
#115573 = EDGE_LOOP ( 'NONE', ( #129138, #77263, #42401, #110933 ) ) ;
#115574 = VERTEX_POINT ( 'NONE', #111509 ) ;
#115576 = ORIENTED_EDGE ( 'NONE', *, *, #19091, .F. ) ;
#115575 = VECTOR ( 'NONE', #108551, 1000.000000000000000 ) ;
#115577 = DIRECTION ( 'NONE',  ( -0.000000000000000000, -1.000000000000000000, -0.000000000000000000 ) ) ;
#115578 = AXIS2_PLACEMENT_3D ( 'NONE', #19534, #59501, #60759 ) ;
#115579 = LINE ( 'NONE', #26579, #2783 ) ;
#115580 = EDGE_LOOP ( 'NONE', ( #115683, #33611 ) ) ;
#115581 = FACE_BOUND ( 'NONE', #97834, .T. ) ;
#115582 = CIRCLE ( 'NONE', #124006, 0.06509327318403745899 ) ;
#115583 = CARTESIAN_POINT ( 'NONE',  ( -13.09999999999999076, 12.50000000000000000, 4.676537180435972552 ) ) ;
#115584 = CARTESIAN_POINT ( 'NONE',  ( -3.100000000000028511, 12.50000000000000000, -4.676537180435977881 ) ) ;
#115585 = EDGE_CURVE ( 'NONE', #107896, #104107, #11393, .T. ) ;
#115586 = DIRECTION ( 'NONE',  ( -0.000000000000000000, -1.000000000000000000, -0.000000000000000000 ) ) ;
#115587 = EDGE_CURVE ( 'NONE', #57456, #98705, #19727, .T. ) ;
#115588 = DIRECTION ( 'NONE',  ( 0.000000000000000000, 0.000000000000000000, 1.000000000000000000 ) ) ;
#115589 = EDGE_CURVE ( 'NONE', #106720, #43544, #65769, .T. ) ;
#115590 = FACE_OUTER_BOUND ( 'NONE', #76815, .T. ) ;
#115591 = EDGE_CURVE ( 'NONE', #121302, #1776, #43442, .T. ) ;
#115592 = ORIENTED_EDGE ( 'NONE', *, *, #114546, .F. ) ;
#115593 = FACE_OUTER_BOUND ( 'NONE', #79179, .T. ) ;
#115594 = VERTEX_POINT ( 'NONE', #125833 ) ;
#115595 = ORIENTED_EDGE ( 'NONE', *, *, #108084, .T. ) ;
#115596 = VERTEX_POINT ( 'NONE', #95746 ) ;
#115597 = CARTESIAN_POINT ( 'NONE',  ( -4.150000000000025224, 12.50000000000000000, -1.537336459617587581 ) ) ;
#115598 = DIRECTION ( 'NONE',  ( 0.000000000000000000, -0.9999939076577903929, 0.003490651415223739937 ) ) ;
#115599 = FACE_OUTER_BOUND ( 'NONE', #111868, .T. ) ;
#115600 = ORIENTED_EDGE ( 'NONE', *, *, #79761, .F. ) ;
#115601 = ADVANCED_FACE ( 'NONE', ( #85272 ), #23936, .T. ) ;
#115602 = CARTESIAN_POINT ( 'NONE',  ( 15.50772381592150850, 1.500000000000000888, -6.996973294590575598 ) ) ;
#115603 = VECTOR ( 'NONE', #49081, 1000.000000000000000 ) ;
#115605 = EDGE_CURVE ( 'NONE', #86614, #34741, #104899, .T. ) ;
#115604 = CIRCLE ( 'NONE', #27884, 0.1000000000000002554 ) ;
#115607 = FACE_OUTER_BOUND ( 'NONE', #69928, .T. ) ;
#115606 = CIRCLE ( 'NONE', #691, 0.1000000000000000056 ) ;
#115608 = ADVANCED_FACE ( 'NONE', ( #93182 ), #65630, .T. ) ;
#115609 = DIRECTION ( 'NONE',  ( 0.000000000000000000, 0.000000000000000000, -1.000000000000000000 ) ) ;
#115610 = CARTESIAN_POINT ( 'NONE',  ( 186.5260416670080588, -6.551208109652273848, -3.782341765625003571 ) ) ;
#115611 = FACE_OUTER_BOUND ( 'NONE', #100787, .T. ) ;
#115612 = PRODUCT_RELATED_PRODUCT_CATEGORY ( 'part', '', ( #111975 ) ) ;
#115613 = DIRECTION ( 'NONE',  ( -0.000000000000000000, 1.000000000000000000, -0.000000000000000000 ) ) ;
#115614 = CIRCLE ( 'NONE', #27791, 0.06509327318403745899 ) ;
#115615 = ORIENTED_EDGE ( 'NONE', *, *, #15703, .T. ) ;
#115616 = FACE_OUTER_BOUND ( 'NONE', #44048, .T. ) ;
#115617 = AXIS2_PLACEMENT_3D ( 'NONE', #108414, #117565, #58684 ) ;
#115618 = AXIS2_PLACEMENT_3D ( 'NONE', #125124, #95023, #65551 ) ;
#115619 = VERTEX_POINT ( 'NONE', #85904 ) ;
#115620 = AXIS2_PLACEMENT_3D ( 'NONE', #15213, #65624, #125199 ) ;
#115621 = VERTEX_POINT ( 'NONE', #5417 ) ;
#115622 = DIRECTION ( 'NONE',  ( 0.000000000000000000, 0.000000000000000000, 1.000000000000000000 ) ) ;
#115623 = DIRECTION ( 'NONE',  ( 0.000000000000000000, -0.000000000000000000, 1.000000000000000000 ) ) ;
#115624 = DIRECTION ( 'NONE',  ( 0.000000000000000000, 0.000000000000000000, -1.000000000000000000 ) ) ;
#115625 = CIRCLE ( 'NONE', #11069, 0.09999999999999982514 ) ;
#115626 = VERTEX_POINT ( 'NONE', #103638 ) ;
#115627 = ORIENTED_EDGE ( 'NONE', *, *, #53880, .F. ) ;
#115628 = DIRECTION ( 'NONE',  ( 0.000000000000000000, 0.000000000000000000, 1.000000000000000000 ) ) ;
#115630 = AXIS2_PLACEMENT_3D ( 'NONE', #61155, #62460, #112189 ) ;
#115629 = DIRECTION ( 'NONE',  ( -4.274815082592931898E-19, -0.9999939076577903929, -0.003490651415223739937 ) ) ;
#115631 = AXIS2_PLACEMENT_3D ( 'NONE', #128583, #47423, #118727 ) ;
#115632 = CONICAL_SURFACE ( 'NONE', #2778, 0.1000000000000002554, 0.003490658503988666988 ) ;
#115633 = CARTESIAN_POINT ( 'NONE',  ( -6.650000000000019007, 2.500000000000000000, -5.902370205355750521 ) ) ;
#115634 = VERTEX_POINT ( 'NONE', #15222 ) ;
#115635 = ORIENTED_EDGE ( 'NONE', *, *, #25797, .T. ) ;
#115636 = CARTESIAN_POINT ( 'NONE',  ( -14.14999999999998614, 2.500000000000000000, 2.065063509461101621 ) ) ;
#115637 = VECTOR ( 'NONE', #19475, 1000.000000000000000 ) ;
#115638 = VERTEX_POINT ( 'NONE', #36195 ) ;
#115639 = CARTESIAN_POINT ( 'NONE',  ( -5.600000000000023626, 12.50000000000000000, -4.611443907251939756 ) ) ;
#115640 = CARTESIAN_POINT ( 'NONE',  ( -5.650000000000019895, 12.50000000000000000, 2.511473670974873507 ) ) ;
#115641 = ORIENTED_EDGE ( 'NONE', *, *, #99841, .F. ) ;
#115642 = AXIS2_PLACEMENT_3D ( 'NONE', #48168, #56671, #88056 ) ;
#115643 = CARTESIAN_POINT ( 'NONE',  ( 5.649999999999932854, 12.50000000000000000, 2.576566944158910744 ) ) ;
#115644 = DIRECTION ( 'NONE',  ( 0.000000000000000000, -0.9999939076577903929, 0.003490651415223739937 ) ) ;
#115645 = CARTESIAN_POINT ( 'NONE',  ( -0.8500000000000395017, 2.500000000000000000, 6.495190528383297135 ) ) ;
#115646 = PLANE ( 'NONE',  #100233 ) ;
#115647 = ORIENTED_EDGE ( 'NONE', *, *, #29308, .F. ) ;
#115648 = EDGE_CURVE ( 'NONE', #120245, #62516, #74816, .T. ) ;
#115649 = FACE_OUTER_BOUND ( 'NONE', #85096, .T. ) ;
#115651 = EDGE_CURVE ( 'NONE', #18238, #91316, #13947, .T. ) ;
#115650 = CARTESIAN_POINT ( 'NONE',  ( -6.071532165918824830E-15, 2.500000000000000000, -4.330127018922201643 ) ) ;
#115652 = ORIENTED_EDGE ( 'NONE', *, *, #52665, .T. ) ;
#115653 = ORIENTED_EDGE ( 'NONE', *, *, #39365, .F. ) ;
#115654 = AXIS2_PLACEMENT_3D ( 'NONE', #120332, #60143, #38571 ) ;
#115655 = VECTOR ( 'NONE', #27889, 1000.000000000000000 ) ;
#115656 = CARTESIAN_POINT ( 'NONE',  ( 184.9635416670080872, -4.367472073101519747, 7.564683531249999149 ) ) ;
#115657 = CARTESIAN_POINT ( 'NONE',  ( -13.54999999999998828, 2.500000000000000000, -2.511473670974875727 ) ) ;
#115658 = CARTESIAN_POINT ( 'NONE',  ( 6.249999999999930722, 2.500000000000000000, 1.372243186433545370 ) ) ;
#115659 = DIRECTION ( 'NONE',  ( 0.000000000000000000, 0.000000000000000000, -1.000000000000000000 ) ) ;
#115660 = LINE ( 'NONE', #87485, #53170 ) ;
#115661 = EDGE_CURVE ( 'NONE', #129597, #109041, #4120, .T. ) ;
#115662 = CARTESIAN_POINT ( 'NONE',  ( 11.64999999999990443, 2.500000000000000000, -5.902370205355750521 ) ) ;
#115663 = CIRCLE ( 'NONE', #82229, 0.1000000000000002554 ) ;
#115664 = PLANE ( 'NONE',  #19628 ) ;
#115665 = CONICAL_SURFACE ( 'NONE', #63450, 0.1000000000000000472, 0.003490658503988666988 ) ;
#115666 = DIRECTION ( 'NONE',  ( 0.000000000000000000, 0.000000000000000000, 1.000000000000000000 ) ) ;
#115668 = CONICAL_SURFACE ( 'NONE', #23753, 0.09999999999999982514, 0.003490658503988666988 ) ;
#115667 = CARTESIAN_POINT ( 'NONE',  ( 3.749999999999942268, 12.50000000000000000, -5.802370205355749988 ) ) ;
#115669 = CIRCLE ( 'NONE', #46730, 0.06509327318403745899 ) ;
#115670 = DIRECTION ( 'NONE',  ( -0.000000000000000000, 1.000000000000000000, -0.000000000000000000 ) ) ;
#115671 = ORIENTED_EDGE ( 'NONE', *, *, #66093, .F. ) ;
#115672 = AXIS2_PLACEMENT_3D ( 'NONE', #44547, #84475, #74644 ) ;
#115673 = CIRCLE ( 'NONE', #63457, 0.1000000000000000472 ) ;
#115674 = CIRCLE ( 'NONE', #128222, 0.06509327318403745899 ) ;
#115675 = ORIENTED_EDGE ( 'NONE', *, *, #100691, .T. ) ;
#115676 = CIRCLE ( 'NONE', #30027, 0.06509327318403745899 ) ;
#115677 = AXIS2_PLACEMENT_3D ( 'NONE', #31480, #90373, #71375 ) ;
#115678 = VERTEX_POINT ( 'NONE', #13297 ) ;
#115679 = FACE_OUTER_BOUND ( 'NONE', #106915, .T. ) ;
#115680 = DIRECTION ( 'NONE',  ( -0.000000000000000000, 1.000000000000000000, -0.000000000000000000 ) ) ;
#115681 = CARTESIAN_POINT ( 'NONE',  ( 10.39999999999990976, 2.500000000000000000, -4.330127018922201643 ) ) ;
#115682 = CIRCLE ( 'NONE', #23465, 0.09999999999999982514 ) ;
#115683 = ORIENTED_EDGE ( 'NONE', *, *, #45304, .F. ) ;
#115684 = CARTESIAN_POINT ( 'NONE',  ( 19.95908882845301235, -2.629614671951224114, -2.273431397254409791 ) ) ;
#115685 = DIRECTION ( 'NONE',  ( 0.000000000000000000, 0.000000000000000000, -1.000000000000000000 ) ) ;
#115687 = ORIENTED_EDGE ( 'NONE', *, *, #93150, .F. ) ;
#115686 = DIRECTION ( 'NONE',  ( 0.000000000000000000, -0.000000000000000000, 1.000000000000000000 ) ) ;
#115689 = CARTESIAN_POINT ( 'NONE',  ( -9.150000000000011013, 2.500000000000000000, -5.902370205355745192 ) ) ;
#115688 = CIRCLE ( 'NONE', #13284, 0.06509327318403745899 ) ;
#115690 = ORIENTED_EDGE ( 'NONE', *, *, #53732, .T. ) ;
#115692 = EDGE_LOOP ( 'NONE', ( #56603, #15874 ) ) ;
#115691 = EDGE_CURVE ( 'NONE', #10004, #127025, #105566, .T. ) ;
#115693 = VERTEX_POINT ( 'NONE', #44064 ) ;
#115694 = ORIENTED_EDGE ( 'NONE', *, *, #124345, .T. ) ;
#115695 = DIRECTION ( 'NONE',  ( -4.274815082592931898E-19, -0.9999939076577903929, -0.003490651415223739937 ) ) ;
#115697 = VECTOR ( 'NONE', #80473, 1000.000000000000000 ) ;
#115696 = DIRECTION ( 'NONE',  ( -0.000000000000000000, 1.000000000000000000, -0.000000000000000000 ) ) ;
#115698 = DIRECTION ( 'NONE',  ( 0.000000000000000000, 1.000000000000000000, 0.000000000000000000 ) ) ;
#115699 = VECTOR ( 'NONE', #40099, 1000.000000000000000 ) ;
#115700 = FACE_OUTER_BOUND ( 'NONE', #14478, .T. ) ;
#115701 = AXIS2_PLACEMENT_3D ( 'NONE', #74351, #114271, #104453 ) ;
#115702 = EDGE_LOOP ( 'NONE', ( #16212, #7519 ) ) ;
#115703 = CARTESIAN_POINT ( 'NONE',  ( 11.84999999999990727, 2.500000000000000000, -1.818653347947326138 ) ) ;
#115705 = ORIENTED_EDGE ( 'NONE', *, *, #51746, .F. ) ;
#115704 = EDGE_CURVE ( 'NONE', #74258, #94015, #3002, .T. ) ;
#115706 = CARTESIAN_POINT ( 'NONE',  ( 17.50000000000000000, 2.500000000000000000, 0.000000000000000000 ) ) ;
#115707 = CARTESIAN_POINT ( 'NONE',  ( 16.31259999906291114, -2.499999999999869882, -6.357732693022873249 ) ) ;
#115708 = LINE ( 'NONE', #96077, #123791 ) ;
#115709 = CARTESIAN_POINT ( 'NONE',  ( 16.86689433361524237, -2.548103353433781137, 5.776876940645016667 ) ) ;
#115710 = EDGE_CURVE ( 'NONE', #106656, #71464, #97079, .T. ) ;
#115711 = AXIS2_PLACEMENT_3D ( 'NONE', #72604, #11737, #43799 ) ;
#115712 = AXIS2_PLACEMENT_3D ( 'NONE', #112297, #90715, #80259 ) ;
#115713 = AXIS2_PLACEMENT_3D ( 'NONE', #60883, #68766, #125445 ) ;
#115714 = EDGE_LOOP ( 'NONE', ( #5744, #103608, #79253, #43291 ) ) ;
#115715 = AXIS2_PLACEMENT_3D ( 'NONE', #59391, #66112, #39103 ) ;
#115716 = VERTEX_POINT ( 'NONE', #53886 ) ;
#115717 = ORIENTED_EDGE ( 'NONE', *, *, #84449, .F. ) ;
#115718 = CARTESIAN_POINT ( 'NONE',  ( -2.700000000000030820, 12.50000000000000000, 0.2813168883297361700 ) ) ;
#115719 = DIRECTION ( 'NONE',  ( 0.000000000000000000, 0.000000000000000000, 1.000000000000000000 ) ) ;
#115720 = ADVANCED_FACE ( 'NONE', ( #93815 ), #74103, .T. ) ;
#115721 = CARTESIAN_POINT ( 'NONE',  ( 1.249999999999952038, 2.500000000000000000, 2.957883832488649389 ) ) ;
#115722 = FACE_BOUND ( 'NONE', #98642, .T. ) ;
#115723 = DIRECTION ( 'NONE',  ( 0.000000000000000000, 0.000000000000000000, -1.000000000000000000 ) ) ;
#115724 = DIRECTION ( 'NONE',  ( 0.000000000000000000, 0.000000000000000000, 1.000000000000000000 ) ) ;
#115725 = CARTESIAN_POINT ( 'NONE',  ( -3.350000000000028511, 12.50000000000000000, -1.407149913249512663 ) ) ;
#115726 = DIRECTION ( 'NONE',  ( -0.000000000000000000, -1.000000000000000000, -0.000000000000000000 ) ) ;
#115727 = CIRCLE ( 'NONE', #119943, 0.1000000000000002554 ) ;
#115728 = CONICAL_SURFACE ( 'NONE', #105275, 0.09999999999999982514, 0.003490658503988666988 ) ;
#115729 = CIRCLE ( 'NONE', #59334, 0.06509327318403745899 ) ;
#115730 = CARTESIAN_POINT ( 'NONE',  ( 186.3802083336747444, 4.367472073101515306, 7.564683531250000925 ) ) ;
#115731 = CARTESIAN_POINT ( 'NONE',  ( 7.099999999999927702, 12.50000000000000000, 5.088040615133786027 ) ) ;
#115732 = CIRCLE ( 'NONE', #117772, 0.09999999999999982514 ) ;
#115733 = CARTESIAN_POINT ( 'NONE',  ( 2.099999999999950351, 12.50000000000000000, -4.330127018922201643 ) ) ;
#115734 = AXIS2_PLACEMENT_3D ( 'NONE', #84017, #15258, #123941 ) ;
#115735 = DIRECTION ( 'NONE',  ( -0.000000000000000000, -1.000000000000000000, -0.000000000000000000 ) ) ;
#115736 = EDGE_CURVE ( 'NONE', #61169, #91540, #123905, .T. ) ;
#115737 = ORIENTED_EDGE ( 'NONE', *, *, #66565, .T. ) ;
#115738 = EDGE_LOOP ( 'NONE', ( #43554, #8274 ) ) ;
#115739 = ORIENTED_EDGE ( 'NONE', *, *, #66586, .T. ) ;
#115740 = ORIENTED_EDGE ( 'NONE', *, *, #58889, .F. ) ;
#115741 = DIRECTION ( 'NONE',  ( -0.000000000000000000, 1.000000000000000000, -0.000000000000000000 ) ) ;
#115742 = FACE_BOUND ( 'NONE', #114445, .T. ) ;
#115743 = DIRECTION ( 'NONE',  ( 0.000000000000000000, 1.000000000000000000, 0.000000000000000000 ) ) ;
#115744 = EDGE_CURVE ( 'NONE', #90590, #93494, #74173, .T. ) ;
#115746 = ORIENTED_EDGE ( 'NONE', *, *, #120603, .T. ) ;
#115745 = VECTOR ( 'NONE', #86836, 1000.000000000000000 ) ;
#115747 = EDGE_CURVE ( 'NONE', #110840, #24259, #4760, .T. ) ;
#115749 = AXIS2_PLACEMENT_3D ( 'NONE', #48322, #79087, #89534 ) ;
#115748 = CARTESIAN_POINT ( 'NONE',  ( 81.97643238330996951, 3.858501987875655903, 6.173828415102756928 ) ) ;
#115750 = EDGE_CURVE ( 'NONE', #47076, #51861, #72054, .T. ) ;
#115751 = CARTESIAN_POINT ( 'NONE',  ( -0.4500000000000397571, 2.500000000000000000, -2.165063509461101710 ) ) ;
#115752 = EDGE_CURVE ( 'NONE', #53951, #78167, #10825, .T. ) ;
#115753 = EDGE_CURVE ( 'NONE', #98217, #78977, #88766, .T. ) ;
#115754 = VERTEX_POINT ( 'NONE', #21309 ) ;
#115755 = CARTESIAN_POINT ( 'NONE',  ( 9.149999999999920419, 2.500000000000000000, 2.957883832488649389 ) ) ;
#115756 = DIRECTION ( 'NONE',  ( 0.000000000000000000, 0.000000000000000000, 1.000000000000000000 ) ) ;
#115757 = AXIS2_PLACEMENT_3D ( 'NONE', #23420, #43744, #55476 ) ;
#115758 = VECTOR ( 'NONE', #58563, 1000.000000000000000 ) ;
#115759 = CONICAL_SURFACE ( 'NONE', #84473, 0.1000000000000002554, 0.003490658503988666988 ) ;
#115760 = ADVANCED_FACE ( 'NONE', ( #101175 ), #112289, .T. ) ;
#115761 = ORIENTED_EDGE ( 'NONE', *, *, #37728, .F. ) ;
#115762 = DIRECTION ( 'NONE',  ( 0.000000000000000000, 0.000000000000000000, 1.000000000000000000 ) ) ;
#115763 = EDGE_CURVE ( 'NONE', #5094, #6351, #99144, .T. ) ;
#115764 = CARTESIAN_POINT ( 'NONE',  ( 3.549999999999942091, 2.500000000000000000, 2.511473670974873507 ) ) ;
#115765 = AXIS2_PLACEMENT_3D ( 'NONE', #43132, #50347, #31365 ) ;
#115766 = EDGE_CURVE ( 'NONE', #103538, #48968, #69324, .T. ) ;
#115768 = ORIENTED_EDGE ( 'NONE', *, *, #91526, .F. ) ;
#115767 = CIRCLE ( 'NONE', #80279, 0.1000000000000002554 ) ;
#115769 = AXIS2_PLACEMENT_3D ( 'NONE', #22557, #62480, #63758 ) ;
#115770 = DIRECTION ( 'NONE',  ( 0.000000000000000000, -0.9999939076577903929, 0.003490651415223739937 ) ) ;
#115771 = EDGE_CURVE ( 'NONE', #85218, #97290, #86604, .T. ) ;
#115772 = CARTESIAN_POINT ( 'NONE',  ( -7.050000000000013145, 12.50000000000000000, 6.495190528383297135 ) ) ;
#115773 = ORIENTED_EDGE ( 'NONE', *, *, #44067, .T. ) ;
#115774 = DIRECTION ( 'NONE',  ( 0.000000000000000000, 0.000000000000000000, 1.000000000000000000 ) ) ;
#115776 = EDGE_LOOP ( 'NONE', ( #23042, #11811, #69255, #53947 ) ) ;
#115775 = AXIS2_PLACEMENT_3D ( 'NONE', #13747, #53691, #74619 ) ;
#115777 = ORIENTED_EDGE ( 'NONE', *, *, #55873, .F. ) ;
#115778 = FACE_OUTER_BOUND ( 'NONE', #40641, .T. ) ;
#115779 = ADVANCED_FACE ( 'NONE', ( #33714 ), #109609, .T. ) ;
#115780 = EDGE_LOOP ( 'NONE', ( #41209, #98694, #68289, #18278 ) ) ;
#115781 = DIRECTION ( 'NONE',  ( -0.000000000000000000, 1.000000000000000000, -0.000000000000000000 ) ) ;
#115782 = DIRECTION ( 'NONE',  ( 0.000000000000000000, 0.000000000000000000, -1.000000000000000000 ) ) ;
#115783 = EDGE_LOOP ( 'NONE', ( #105116, #32240 ) ) ;
#115784 = DIRECTION ( 'NONE',  ( 0.000000000000000000, 1.000000000000000000, 0.000000000000000000 ) ) ;
#115785 = CARTESIAN_POINT ( 'NONE',  ( 8.749999999999923617, 2.500000000000000000, 1.472243186433545459 ) ) ;
#115786 = DIRECTION ( 'NONE',  ( -4.274815082592931898E-19, -0.9999939076577903929, -0.003490651415223739937 ) ) ;
#115787 = FACE_OUTER_BOUND ( 'NONE', #1042, .T. ) ;
#115788 = DIRECTION ( 'NONE',  ( -0.000000000000000000, 1.000000000000000000, -0.000000000000000000 ) ) ;
#115789 = CARTESIAN_POINT ( 'NONE',  ( 6.049999999999934097, 2.500000000000000000, 6.148780366869520897 ) ) ;
#115790 = AXIS2_PLACEMENT_3D ( 'NONE', #10446, #18327, #98178 ) ;
#115791 = ORIENTED_EDGE ( 'NONE', *, *, #52066, .T. ) ;
#115792 = VERTEX_POINT ( 'NONE', #71707 ) ;
#115793 = DIRECTION ( 'NONE',  ( 0.000000000000000000, 0.000000000000000000, -1.000000000000000000 ) ) ;
#115794 = PLANE ( 'NONE',  #80792 ) ;
#115795 = DIRECTION ( 'NONE',  ( 0.000000000000000000, 0.000000000000000000, 1.000000000000000000 ) ) ;
#115797 = VERTEX_POINT ( 'NONE', #3612 ) ;
#115796 = EDGE_LOOP ( 'NONE', ( #67292, #76898, #19503, #78747 ) ) ;
#115798 = ORIENTED_EDGE ( 'NONE', *, *, #51059, .T. ) ;
#115799 = DIRECTION ( 'NONE',  ( 0.000000000000000000, 1.000000000000000000, 0.000000000000000000 ) ) ;
#115800 = VECTOR ( 'NONE', #42365, 1000.000000000000000 ) ;
#115801 = DIRECTION ( 'NONE',  ( -0.000000000000000000, 1.000000000000000000, -0.000000000000000000 ) ) ;
#115802 = AXIS2_PLACEMENT_3D ( 'NONE', #106078, #16375, #25563 ) ;
#115803 = DIRECTION ( 'NONE',  ( -0.000000000000000000, -1.000000000000000000, -0.000000000000000000 ) ) ;
#115804 = CARTESIAN_POINT ( 'NONE',  ( 107.5000000000000142, 0.000000000000000000, 0.000000000000000000 ) ) ;
#115805 = CARTESIAN_POINT ( 'NONE',  ( 0.3999999999999559464, 2.500000000000000000, -4.330127018922201643 ) ) ;
#115806 = DIRECTION ( 'NONE',  ( -4.274815082592931898E-19, -0.9999939076577903929, -0.003490651415223739937 ) ) ;
#115807 = DIRECTION ( 'NONE',  ( 0.000000000000000000, 0.000000000000000000, 1.000000000000000000 ) ) ;
#115808 = DIRECTION ( 'NONE',  ( 0.000000000000000000, 1.000000000000000000, 0.000000000000000000 ) ) ;
#115809 = DIRECTION ( 'NONE',  ( 0.000000000000000000, 1.000000000000000000, 0.000000000000000000 ) ) ;
#115810 = AXIS2_PLACEMENT_3D ( 'NONE', #92066, #112371, #52795 ) ;
#115811 = FACE_OUTER_BOUND ( 'NONE', #39532, .T. ) ;
#115812 = AXIS2_PLACEMENT_3D ( 'NONE', #53980, #23216, #65064 ) ;
#115813 = ORIENTED_EDGE ( 'NONE', *, *, #128049, .F. ) ;
#115814 = CIRCLE ( 'NONE', #4987, 0.09999999999999982514 ) ;
#115815 = EDGE_CURVE ( 'NONE', #62716, #83439, #11500, .T. ) ;
#115816 = EDGE_CURVE ( 'NONE', #62036, #58504, #57373, .T. ) ;
#115817 = DIRECTION ( 'NONE',  ( 0.000000000000000000, 1.000000000000000000, 0.000000000000000000 ) ) ;
#115818 = VERTEX_POINT ( 'NONE', #92636 ) ;
#115819 = EDGE_LOOP ( 'NONE', ( #102808, #50786 ) ) ;
#115820 = FACE_OUTER_BOUND ( 'NONE', #98242, .T. ) ;
#115821 = FACE_OUTER_BOUND ( 'NONE', #109333, .T. ) ;
#115822 = DIRECTION ( 'NONE',  ( 0.000000000000000000, 0.000000000000000000, 1.000000000000000000 ) ) ;
#115823 = DIRECTION ( 'NONE',  ( 0.000000000000000000, 0.000000000000000000, 1.000000000000000000 ) ) ;
#115824 = CARTESIAN_POINT ( 'NONE',  ( 10.39999999999990976, 2.500000000000000000, -4.230127018922201998 ) ) ;
#115825 = CIRCLE ( 'NONE', #80334, 0.1000000000000002554 ) ;
#115826 = CARTESIAN_POINT ( 'NONE',  ( 4.149999999999939959, 2.500000000000000000, -2.165063509461101710 ) ) ;
#115827 = CIRCLE ( 'NONE', #30168, 0.06509327318403745899 ) ;
#115828 = CONICAL_SURFACE ( 'NONE', #7148, 0.1000000000000002554, 0.003490658503988666988 ) ;
#115829 = DIRECTION ( 'NONE',  ( 0.000000000000000000, 0.000000000000000000, -1.000000000000000000 ) ) ;
#115830 = ORIENTED_EDGE ( 'NONE', *, *, #13667, .T. ) ;
#115831 = DIRECTION ( 'NONE',  ( 0.000000000000000000, 0.000000000000000000, 1.000000000000000000 ) ) ;
#115832 = CIRCLE ( 'NONE', #36437, 0.06509327318403745899 ) ;
#115833 = AXIS2_PLACEMENT_3D ( 'NONE', #117640, #71139, #83557 ) ;
#115834 = FACE_OUTER_BOUND ( 'NONE', #122729, .T. ) ;
#115835 = EDGE_LOOP ( 'NONE', ( #34215, #66693 ) ) ;
#115836 = VERTEX_POINT ( 'NONE', #61906 ) ;
#115837 = EDGE_LOOP ( 'NONE', ( #28086, #35267 ) ) ;
#115838 = EDGE_LOOP ( 'NONE', ( #118218, #9975, #90747, #124286 ) ) ;
#115839 = CARTESIAN_POINT ( 'NONE',  ( 1.849999999999951017, 2.500000000000000000, -6.248780366869526759 ) ) ;
#115840 = DIRECTION ( 'NONE',  ( -4.274815082592931898E-19, -0.9999939076577903929, -0.003490651415223739937 ) ) ;
#115841 = DIRECTION ( 'NONE',  ( 0.000000000000000000, 0.000000000000000000, -1.000000000000000000 ) ) ;
#115842 = FACE_OUTER_BOUND ( 'NONE', #95464, .T. ) ;
#115843 = VECTOR ( 'NONE', #96656, 1000.000000000000000 ) ;
#115844 = CARTESIAN_POINT ( 'NONE',  ( 0.6499999999999566125, 2.500000000000000000, -6.741600689897077281 ) ) ;
#115845 = ORIENTED_EDGE ( 'NONE', *, *, #41648, .F. ) ;
#115846 = AXIS2_PLACEMENT_3D ( 'NONE', #43563, #80900, #91350 ) ;
#115847 = AXIS2_PLACEMENT_3D ( 'NONE', #22754, #30635, #43048 ) ;
#115848 = DIRECTION ( 'NONE',  ( -0.000000000000000000, 1.000000000000000000, -0.000000000000000000 ) ) ;
#115849 = CARTESIAN_POINT ( 'NONE',  ( 187.0729166673494603, 4.445597072760113733, -7.700000000000009948 ) ) ;
#115850 = EDGE_CURVE ( 'NONE', #74354, #71030, #101820, .T. ) ;
#115851 = EDGE_LOOP ( 'NONE', ( #48925, #8596 ) ) ;
#115852 = CIRCLE ( 'NONE', #59451, 0.1000000000000002554 ) ;
#115853 = AXIS2_PLACEMENT_3D ( 'NONE', #110343, #71066, #81532 ) ;
#115854 = ORIENTED_EDGE ( 'NONE', *, *, #68302, .T. ) ;
#115855 = AXIS2_PLACEMENT_3D ( 'NONE', #40003, #10510, #90359 ) ;
#115856 = ORIENTED_EDGE ( 'NONE', *, *, #87035, .T. ) ;
#115857 = CARTESIAN_POINT ( 'NONE',  ( 3.349999999999941913, 2.500000000000000000, 6.495190528383297135 ) ) ;
#115858 = EDGE_CURVE ( 'NONE', #86174, #90407, #82175, .T. ) ;
#115859 = DIRECTION ( 'NONE',  ( 0.000000000000000000, 0.000000000000000000, 1.000000000000000000 ) ) ;
#115860 = CARTESIAN_POINT ( 'NONE',  ( 0.4499999999999552136, 2.500000000000000000, 6.395190528383296602 ) ) ;
#115861 = AXIS2_PLACEMENT_3D ( 'NONE', #60033, #122167, #91396 ) ;
#115862 = CIRCLE ( 'NONE', #38620, 0.1000000000000002554 ) ;
#115863 = AXIS2_PLACEMENT_3D ( 'NONE', #26896, #115910, #64867 ) ;
#115864 = AXIS2_PLACEMENT_3D ( 'NONE', #29400, #71235, #50317 ) ;
#115866 = ORIENTED_EDGE ( 'NONE', *, *, #71010, .T. ) ;
#115865 = EDGE_CURVE ( 'NONE', #6379, #84904, #30203, .T. ) ;
#115867 = DIRECTION ( 'NONE',  ( 0.000000000000000000, 0.000000000000000000, 1.000000000000000000 ) ) ;
#115868 = LINE ( 'NONE', #26205, #95618 ) ;
#115869 = FACE_OUTER_BOUND ( 'NONE', #104635, .T. ) ;
#115870 = CARTESIAN_POINT ( 'NONE',  ( -11.84999999999999609, 2.500000000000000000, 1.818653347947321475 ) ) ;
#115871 = EDGE_CURVE ( 'NONE', #101758, #121980, #126619, .T. ) ;
#115872 = DIRECTION ( 'NONE',  ( -0.000000000000000000, 1.000000000000000000, -0.000000000000000000 ) ) ;
#115873 = EDGE_LOOP ( 'NONE', ( #422, #122323, #29165, #79588 ) ) ;
#115874 = PLANE ( 'NONE',  #1877 ) ;
#115875 = VERTEX_POINT ( 'NONE', #84752 ) ;
#115876 = ORIENTED_EDGE ( 'NONE', *, *, #73089, .F. ) ;
#115877 = VERTEX_POINT ( 'NONE', #125319 ) ;
#115878 = EDGE_CURVE ( 'NONE', #9138, #107707, #120070, .T. ) ;
#115879 = DIRECTION ( 'NONE',  ( -0.000000000000000000, -1.000000000000000000, -0.000000000000000000 ) ) ;
#115880 = FACE_BOUND ( 'NONE', #67145, .T. ) ;
#115881 = DIRECTION ( 'NONE',  ( -0.000000000000000000, 1.000000000000000000, -0.000000000000000000 ) ) ;
#115882 = CIRCLE ( 'NONE', #957, 0.06509327318403745899 ) ;
#115883 = FACE_OUTER_BOUND ( 'NONE', #56713, .T. ) ;
#115884 = CARTESIAN_POINT ( 'NONE',  ( -8.950000000000008171, 2.500000000000000000, 1.918653347947321564 ) ) ;
#115885 = ORIENTED_EDGE ( 'NONE', *, *, #39578, .T. ) ;
#115886 = PLANE ( 'NONE',  #127524 ) ;
#115887 = CARTESIAN_POINT ( 'NONE',  ( 11.84999999999990727, 2.500000000000000000, 6.248780366869520542 ) ) ;
#115888 = CARTESIAN_POINT ( 'NONE',  ( 16.32066102237049066, 2.500000000000000000, 4.877377760480499980 ) ) ;
#115889 = CARTESIAN_POINT ( 'NONE',  ( -14.99999999999994671, 12.50000000000000000, 0.06509327318403743123 ) ) ;
#115890 = VERTEX_POINT ( 'NONE', #35031 ) ;
#115891 = AXIS2_PLACEMENT_3D ( 'NONE', #123613, #33965, #105282 ) ;
#115892 = CARTESIAN_POINT ( 'NONE',  ( -1.650000000000034772, 2.500000000000000000, 2.165063509461097713 ) ) ;
#115893 = DIRECTION ( 'NONE',  ( -0.000000000000000000, -1.000000000000000000, -0.000000000000000000 ) ) ;
#115894 = ORIENTED_EDGE ( 'NONE', *, *, #49119, .F. ) ;
#115895 = CARTESIAN_POINT ( 'NONE',  ( 8.749999999999953815, 2.500000000000000000, -2.165063509461101710 ) ) ;
#115896 = FACE_BOUND ( 'NONE', #57843, .T. ) ;
#115897 = DIRECTION ( 'NONE',  ( 0.000000000000000000, 0.000000000000000000, 1.000000000000000000 ) ) ;
#115898 = AXIS2_PLACEMENT_3D ( 'NONE', #1566, #21878, #29748 ) ;
#115899 = EDGE_CURVE ( 'NONE', #124866, #79421, #14053, .T. ) ;
#115900 = EDGE_LOOP ( 'NONE', ( #52924, #26252, #123393, #112561 ) ) ;
#115901 = CARTESIAN_POINT ( 'NONE',  ( 4.799999999999934097, 2.500000000000000000, 4.676537180435972552 ) ) ;
#115902 = CARTESIAN_POINT ( 'NONE',  ( 12.04999999999990834, 12.50000000000000000, 6.495190528383297135 ) ) ;
#115903 = AXIS2_PLACEMENT_3D ( 'NONE', #119142, #39326, #79230 ) ;
#115904 = ORIENTED_EDGE ( 'NONE', *, *, #57587, .T. ) ;
#115905 = ORIENTED_EDGE ( 'NONE', *, *, #49612, .T. ) ;
#115906 = EDGE_CURVE ( 'NONE', #17226, #85840, #113813, .T. ) ;
#115907 = CARTESIAN_POINT ( 'NONE',  ( 187.4166666666666856, 6.668395609140176816, 3.850000000000000977 ) ) ;
#115908 = EDGE_CURVE ( 'NONE', #48001, #26422, #6797, .T. ) ;
#115909 = ORIENTED_EDGE ( 'NONE', *, *, #112829, .F. ) ;
#115910 = DIRECTION ( 'NONE',  ( -0.000000000000000000, 1.000000000000000000, -0.000000000000000000 ) ) ;
#115911 = DIRECTION ( 'NONE',  ( -0.000000000000000000, -1.000000000000000000, -0.000000000000000000 ) ) ;
#115912 = AXIS2_PLACEMENT_3D ( 'NONE', #128314, #129613, #39931 ) ;
#115913 = CONICAL_SURFACE ( 'NONE', #92951, 0.1000000000000002554, 0.003490658503988666988 ) ;
#115914 = DIRECTION ( 'NONE',  ( -0.000000000000000000, 1.000000000000000000, -0.000000000000000000 ) ) ;
#115915 = DIRECTION ( 'NONE',  ( 0.000000000000000000, 0.000000000000000000, 1.000000000000000000 ) ) ;
#115916 = ADVANCED_FACE ( 'NONE', ( #86680 ), #117998, .T. ) ;
#115917 = EDGE_CURVE ( 'NONE', #50837, #30524, #56561, .T. ) ;
#115918 = CONICAL_SURFACE ( 'NONE', #59525, 0.1000000000000002554, 0.003490658503988666988 ) ;
#115919 = CARTESIAN_POINT ( 'NONE',  ( 8.949999999999915801, 2.500000000000000000, -1.818653347947326138 ) ) ;
#115920 = EDGE_CURVE ( 'NONE', #73436, #104132, #78319, .T. ) ;
#115921 = AXIS2_PLACEMENT_3D ( 'NONE', #76949, #68401, #129294 ) ;
#115922 = ORIENTED_EDGE ( 'NONE', *, *, #96650, .F. ) ;
#115923 = DIRECTION ( 'NONE',  ( 0.000000000000000000, 0.000000000000000000, 1.000000000000000000 ) ) ;
#115924 = ADVANCED_FACE ( 'NONE', ( #65745 ), #11492, .T. ) ;
#115925 = PLANE ( 'NONE',  #9993 ) ;
#115926 = FACE_OUTER_BOUND ( 'NONE', #101314, .T. ) ;
#115927 = PLANE ( 'NONE',  #109674 ) ;
#115929 = EDGE_LOOP ( 'NONE', ( #88818, #18552 ) ) ;
#115928 = ORIENTED_EDGE ( 'NONE', *, *, #17985, .T. ) ;
#115930 = FACE_OUTER_BOUND ( 'NONE', #31750, .T. ) ;
#115931 = VERTEX_POINT ( 'NONE', #114837 ) ;
#115932 = CARTESIAN_POINT ( 'NONE',  ( 0.3999999999999628852, 2.500000000000000000, -0.6928203230275520319 ) ) ;
#115933 = CARTESIAN_POINT ( 'NONE',  ( 3.549999999999942979, 12.50000000000000000, 1.818653347947321475 ) ) ;
#115934 = EDGE_CURVE ( 'NONE', #89926, #83615, #38614, .T. ) ;
#115935 = ORIENTED_EDGE ( 'NONE', *, *, #57203, .F. ) ;
#115936 = CARTESIAN_POINT ( 'NONE',  ( 7.299999999999927880, 2.500000000000000000, -4.576537180435977348 ) ) ;
#115937 = CARTESIAN_POINT ( 'NONE',  ( 10.19999999999991402, 2.500000000000000000, 0.4464101615137735513 ) ) ;
#115938 = DIRECTION ( 'NONE',  ( 0.000000000000000000, 0.000000000000000000, -1.000000000000000000 ) ) ;
#115939 = CARTESIAN_POINT ( 'NONE',  ( -10.84999999999999964, 12.50000000000000000, 5.867463478539781896 ) ) ;
#115940 = ORIENTED_EDGE ( 'NONE', *, *, #91041, .F. ) ;
#115941 = AXIS2_PLACEMENT_3D ( 'NONE', #39076, #391, #8286 ) ;
#115942 = DIRECTION ( 'NONE',  ( 0.000000000000000000, 0.000000000000000000, 1.000000000000000000 ) ) ;
#115943 = DIRECTION ( 'NONE',  ( 0.000000000000000000, 0.000000000000000000, 1.000000000000000000 ) ) ;
#115944 = CONICAL_SURFACE ( 'NONE', #105489, 0.1000000000000002554, 0.003490658503988666988 ) ;
#115945 = CIRCLE ( 'NONE', #122214, 0.06509327318403741736 ) ;
#115946 = CARTESIAN_POINT ( 'NONE',  ( 11.44999999999991047, 2.500000000000000000, 6.048780366869520364 ) ) ;
#115947 = DIRECTION ( 'NONE',  ( 0.000000000000000000, -1.000000000000000000, 0.000000000000000000 ) ) ;
#115948 = CARTESIAN_POINT ( 'NONE',  ( -0.8500000000000386136, 2.500000000000000000, 2.957883832488649389 ) ) ;
#115949 = AXIS2_PLACEMENT_3D ( 'NONE', #10366, #119667, #48358 ) ;
#115950 = EDGE_LOOP ( 'NONE', ( #83967, #56717 ) ) ;
#115952 = ORIENTED_EDGE ( 'NONE', *, *, #124515, .T. ) ;
#115951 = CONICAL_SURFACE ( 'NONE', #34497, 0.1000000000000002554, 0.003490658503988666988 ) ;
#115954 = CARTESIAN_POINT ( 'NONE',  ( -9.200000000000009948, 2.500000000000000000, -4.430127018922197735 ) ) ;
#115953 = VECTOR ( 'NONE', #124024, 1000.000000000000000 ) ;
#115955 = VERTEX_POINT ( 'NONE', #105685 ) ;
#115956 = CARTESIAN_POINT ( 'NONE',  ( -9.800000000000004263, 2.500000000000000000, -0.3464101615137783474 ) ) ;
#115959 = VERTEX_POINT ( 'NONE', #75563 ) ;
#115958 = VERTEX_POINT ( 'NONE', #63829 ) ;
#115957 = CIRCLE ( 'NONE', #19819, 0.06509327318403743123 ) ;
#115960 = ORIENTED_EDGE ( 'NONE', *, *, #71614, .F. ) ;
#115961 = DIRECTION ( 'NONE',  ( 0.000000000000000000, 0.000000000000000000, 1.000000000000000000 ) ) ;
#115962 = CARTESIAN_POINT ( 'NONE',  ( -12.29999999999999361, 12.50000000000000000, 3.983716857408420076 ) ) ;
#115963 = DIRECTION ( 'NONE',  ( -4.274815082592931898E-19, -0.9999939076577903929, -0.003490651415223739937 ) ) ;
#115964 = DIRECTION ( 'NONE',  ( 0.000000000000000000, -0.9999939076577903929, 0.003490651415223739937 ) ) ;
#115965 = CARTESIAN_POINT ( 'NONE',  ( 6.249999999999967137, 2.500000000000000000, 6.495190528383297135 ) ) ;
#115966 = CIRCLE ( 'NONE', #5143, 0.1000000000000002554 ) ;
#115967 = DIRECTION ( 'NONE',  ( 0.000000000000000000, 0.000000000000000000, 1.000000000000000000 ) ) ;
#115968 = EDGE_LOOP ( 'NONE', ( #101173, #61800, #88242, #111748 ) ) ;
#115969 = FACE_OUTER_BOUND ( 'NONE', #31752, .T. ) ;
#115970 = EDGE_LOOP ( 'NONE', ( #99188, #12535, #24038, #124744 ) ) ;
#115971 = ORIENTED_EDGE ( 'NONE', *, *, #78087, .T. ) ;
#115972 = ORIENTED_EDGE ( 'NONE', *, *, #5263, .T. ) ;
#115973 = EDGE_CURVE ( 'NONE', #97073, #28400, #105017, .T. ) ;
#115974 = ORIENTED_EDGE ( 'NONE', *, *, #115511, .T. ) ;
#115975 = FACE_OUTER_BOUND ( 'NONE', #65566, .T. ) ;
#115976 = ORIENTED_EDGE ( 'NONE', *, *, #8623, .T. ) ;
#115977 = VERTEX_POINT ( 'NONE', #115471 ) ;
#115978 = VECTOR ( 'NONE', #108187, 1000.000000000000000 ) ;
#115979 = EDGE_CURVE ( 'NONE', #122022, #74917, #122321, .T. ) ;
#115980 = CARTESIAN_POINT ( 'NONE',  ( 142.3152275665817115, 2.500000000000000000, 2.763522878056728693 ) ) ;
#115981 = CARTESIAN_POINT ( 'NONE',  ( -5.400000000000023448, 2.500000000000000000, -4.430127018922202176 ) ) ;
#115982 = CARTESIAN_POINT ( 'NONE',  ( -11.89999999999999680, 12.50000000000000000, -4.048810130592460865 ) ) ;
#115983 = LINE ( 'NONE', #77353, #43009 ) ;
#115984 = CARTESIAN_POINT ( 'NONE',  ( 12.94999999999990337, 2.500000000000000000, 2.165063509461097713 ) ) ;
#115985 = ORIENTED_EDGE ( 'NONE', *, *, #16984, .T. ) ;
#115986 = CARTESIAN_POINT ( 'NONE',  ( 8.299999999999922551, 2.500000000000000000, -4.330127018922201643 ) ) ;
#115987 = CIRCLE ( 'NONE', #120202, 0.09999999999999982514 ) ;
#115988 = CONICAL_SURFACE ( 'NONE', #47043, 0.1000000000000002554, 0.003490658503988666988 ) ;
#115989 = ORIENTED_EDGE ( 'NONE', *, *, #125628, .T. ) ;
#115990 = DIRECTION ( 'NONE',  ( -4.274815082592931898E-19, -0.9999939076577903929, -0.003490651415223739937 ) ) ;
#115991 = ORIENTED_EDGE ( 'NONE', *, *, #9375, .F. ) ;
#115992 = DIRECTION ( 'NONE',  ( -0.000000000000000000, 1.000000000000000000, -0.000000000000000000 ) ) ;
#115993 = ORIENTED_EDGE ( 'NONE', *, *, #124639, .F. ) ;
#115994 = VERTEX_POINT ( 'NONE', #25832 ) ;
#115995 = DIRECTION ( 'NONE',  ( 0.000000000000000000, 0.000000000000000000, 1.000000000000000000 ) ) ;
#115996 = CARTESIAN_POINT ( 'NONE',  ( 4.999999999999973355, 2.500000000000000000, -4.430127018922202176 ) ) ;
#115997 = DIRECTION ( 'NONE',  ( 0.000000000000000000, 0.000000000000000000, 1.000000000000000000 ) ) ;
#115998 = DIRECTION ( 'NONE',  ( 0.000000000000000000, 0.000000000000000000, 1.000000000000000000 ) ) ;
#115999 = CONICAL_SURFACE ( 'NONE', #103483, 0.1000000000000002554, 0.003490658503988666988 ) ;
#116000 = DIRECTION ( 'NONE',  ( -0.000000000000000000, -1.000000000000000000, -0.000000000000000000 ) ) ;
#116001 = EDGE_LOOP ( 'NONE', ( #96217, #718, #68025, #123484 ) ) ;
#116002 = DIRECTION ( 'NONE',  ( 0.000000000000000000, 0.000000000000000000, 1.000000000000000000 ) ) ;
#116003 = CARTESIAN_POINT ( 'NONE',  ( 6.699999999999930012, 2.500000000000000000, -4.330127018922201643 ) ) ;
#116004 = CARTESIAN_POINT ( 'NONE',  ( -6.250000000000021316, 2.500000000000000000, -1.372243186433550033 ) ) ;
#116005 = DIRECTION ( 'NONE',  ( 0.000000000000000000, 1.000000000000000000, 0.000000000000000000 ) ) ;
#116006 = DIRECTION ( 'NONE',  ( 0.000000000000000000, 1.000000000000000000, 0.000000000000000000 ) ) ;
#116007 = EDGE_CURVE ( 'NONE', #55407, #19872, #114215, .T. ) ;
#116008 = ORIENTED_EDGE ( 'NONE', *, *, #5841, .F. ) ;
#116009 = CONICAL_SURFACE ( 'NONE', #59609, 0.09999999999999982514, 0.003490658503988666988 ) ;
#116010 = AXIS2_PLACEMENT_3D ( 'NONE', #99198, #38348, #58634 ) ;
#116011 = ORIENTED_EDGE ( 'NONE', *, *, #66694, .F. ) ;
#116012 = PLANE ( 'NONE',  #90294 ) ;
#116013 = VERTEX_POINT ( 'NONE', #103752 ) ;
#116014 = CARTESIAN_POINT ( 'NONE',  ( 10.39999999999991331, 2.500000000000000000, -2.385244779468109755E-15 ) ) ;
#116016 = ADVANCED_FACE ( 'NONE', ( #44840 ), #65863, .T. ) ;
#116015 = FACE_OUTER_BOUND ( 'NONE', #8704, .T. ) ;
#116018 = VERTEX_POINT ( 'NONE', #116134 ) ;
#116017 = ADVANCED_FACE ( 'NONE', ( #85393 ), #86709, .T. ) ;
#116019 = CARTESIAN_POINT ( 'NONE',  ( 185.7500000000000000, 9.429780353434619030E-16, -7.700000000000000178 ) ) ;
#116020 = DIRECTION ( 'NONE',  ( 0.000000000000000000, 0.000000000000000000, 1.000000000000000000 ) ) ;
#116021 = DIRECTION ( 'NONE',  ( 0.000000000000000000, 0.000000000000000000, 1.000000000000000000 ) ) ;
#116022 = DIRECTION ( 'NONE',  ( 0.000000000000000000, 0.000000000000000000, 1.000000000000000000 ) ) ;
#116023 = EDGE_CURVE ( 'NONE', #22314, #107468, #6171, .T. ) ;
#116024 = CIRCLE ( 'NONE', #124438, 0.06509327318403745899 ) ;
#116025 = FACE_OUTER_BOUND ( 'NONE', #44148, .T. ) ;
#116026 = ORIENTED_EDGE ( 'NONE', *, *, #26445, .T. ) ;
#116028 = DIRECTION ( 'NONE',  ( -0.000000000000000000, 1.000000000000000000, -0.000000000000000000 ) ) ;
#116027 = AXIS2_PLACEMENT_3D ( 'NONE', #49467, #42213, #79553 ) ;
#116029 = LINE ( 'NONE', #26376, #106170 ) ;
#116030 = ADVANCED_FACE ( 'NONE', ( #66393 ), #49170, .T. ) ;
#116031 = AXIS2_PLACEMENT_3D ( 'NONE', #88639, #78187, #128594 ) ;
#116032 = ORIENTED_EDGE ( 'NONE', *, *, #6084, .T. ) ;
#116033 = AXIS2_PLACEMENT_3D ( 'NONE', #115273, #26932, #74748 ) ;
#116034 = EDGE_CURVE ( 'NONE', #71376, #76654, #15675, .T. ) ;
#116035 = DIRECTION ( 'NONE',  ( 0.000000000000000000, 1.000000000000000000, 0.000000000000000000 ) ) ;
#116036 = CARTESIAN_POINT ( 'NONE',  ( -15.39999999999998082, 12.50000000000000000, 0.6928203230275518099 ) ) ;
#116037 = DIRECTION ( 'NONE',  ( -0.000000000000000000, -1.000000000000000000, -0.000000000000000000 ) ) ;
#116038 = CIRCLE ( 'NONE', #36648, 0.06509327318403745899 ) ;
#116039 = EDGE_LOOP ( 'NONE', ( #80690, #113045 ) ) ;
#116040 = CIRCLE ( 'NONE', #1112, 0.1000000000000002554 ) ;
#116041 = FACE_OUTER_BOUND ( 'NONE', #6063, .T. ) ;
#116042 = AXIS2_PLACEMENT_3D ( 'NONE', #104584, #44372, #72567 ) ;
#116043 = VERTEX_POINT ( 'NONE', #109552 ) ;
#116044 = DIRECTION ( 'NONE',  ( 0.000000000000000000, -0.9999939076577903929, 0.003490651415223739937 ) ) ;
#116045 = DIRECTION ( 'NONE',  ( -0.000000000000000000, -1.000000000000000000, -0.000000000000000000 ) ) ;
#116046 = CARTESIAN_POINT ( 'NONE',  ( 4.399999999999939071, 2.500000000000000000, 0.3464101615137736845 ) ) ;
#116047 = ORIENTED_EDGE ( 'NONE', *, *, #22113, .T. ) ;
#116048 = AXIS2_PLACEMENT_3D ( 'NONE', #50171, #61925, #120191 ) ;
#116049 = AXIS2_PLACEMENT_3D ( 'NONE', #85968, #76819, #115416 ) ;
#116050 = DIRECTION ( 'NONE',  ( 0.000000000000000000, 0.000000000000000000, -1.000000000000000000 ) ) ;
#116051 = CARTESIAN_POINT ( 'NONE',  ( 13.29999999999990301, 12.50000000000000000, -4.330127018922201643 ) ) ;
#116052 = AXIS2_PLACEMENT_3D ( 'NONE', #4737, #125187, #74801 ) ;
#116053 = VERTEX_POINT ( 'NONE', #19889 ) ;
#116054 = ORIENTED_EDGE ( 'NONE', *, *, #117221, .F. ) ;
#116055 = CARTESIAN_POINT ( 'NONE',  ( 4.599999999999935696, 2.500000000000000000, 5.022947341949748790 ) ) ;
#116056 = EDGE_LOOP ( 'NONE', ( #39866, #37562 ) ) ;
#116057 = DIRECTION ( 'NONE',  ( -1.000000000000000000, -0.000000000000000000, -0.000000000000000000 ) ) ;
#116058 = CARTESIAN_POINT ( 'NONE',  ( -11.64999999999999680, 2.500000000000000000, -6.495190528383298911 ) ) ;
#116059 = ORIENTED_EDGE ( 'NONE', *, *, #43261, .F. ) ;
#116060 = PLANE ( 'NONE',  #48866 ) ;
#116061 = FACE_OUTER_BOUND ( 'NONE', #89622, .T. ) ;
#116062 = AXIS2_PLACEMENT_3D ( 'NONE', #119298, #109491, #19828 ) ;
#116063 = ORIENTED_EDGE ( 'NONE', *, *, #123702, .F. ) ;
#116064 = EDGE_CURVE ( 'NONE', #54722, #29933, #27752, .T. ) ;
#116065 = DIRECTION ( 'NONE',  ( 0.000000000000000000, 0.000000000000000000, 1.000000000000000000 ) ) ;
#116066 = DIRECTION ( 'NONE',  ( 0.000000000000000000, 0.000000000000000000, 1.000000000000000000 ) ) ;
#116067 = EDGE_CURVE ( 'NONE', #110791, #63955, #82606, .T. ) ;
#116068 = DIRECTION ( 'NONE',  ( 0.000000000000000000, 0.000000000000000000, -1.000000000000000000 ) ) ;
#116069 = DIRECTION ( 'NONE',  ( 0.000000000000000000, 1.000000000000000000, 0.000000000000000000 ) ) ;
#116070 = EDGE_CURVE ( 'NONE', #36428, #116703, #97150, .T. ) ;
#116071 = CARTESIAN_POINT ( 'NONE',  ( 11.24999999999994493, 12.50000000000000000, 6.430097255199259010 ) ) ;
#116072 = CONICAL_SURFACE ( 'NONE', #59677, 0.1000000000000000472, 0.003490658503988666988 ) ;
#116073 = CARTESIAN_POINT ( 'NONE',  ( 7.499999999999925393, 12.50000000000000000, -0.6928203230275541413 ) ) ;
#116074 = EDGE_CURVE ( 'NONE', #4955, #99447, #10061, .T. ) ;
#116075 = EDGE_CURVE ( 'NONE', #54276, #7138, #109703, .T. ) ;
#116076 = AXIS2_PLACEMENT_3D ( 'NONE', #29788, #300, #118807 ) ;
#116077 = ORIENTED_EDGE ( 'NONE', *, *, #62030, .F. ) ;
#116078 = EDGE_LOOP ( 'NONE', ( #119807, #79443, #8060, #92655 ) ) ;
#116080 = ORIENTED_EDGE ( 'NONE', *, *, #23827, .T. ) ;
#116079 = EDGE_CURVE ( 'NONE', #105882, #126334, #34498, .T. ) ;
#116081 = ORIENTED_EDGE ( 'NONE', *, *, #58817, .T. ) ;
#116082 = CARTESIAN_POINT ( 'NONE',  ( 87.50000000000001421, 3.975350567648425759, 6.360562287258741065 ) ) ;
#116083 = CARTESIAN_POINT ( 'NONE',  ( 107.5000000000000142, 0.000000000000000000, 0.000000000000000000 ) ) ;
#116084 = CARTESIAN_POINT ( 'NONE',  ( 12.94999999999989981, 2.500000000000000000, -2.165063509461101710 ) ) ;
#116085 = VERTEX_POINT ( 'NONE', #118718 ) ;
#116086 = FACE_BOUND ( 'NONE', #114632, .T. ) ;
#116087 = DIRECTION ( 'NONE',  ( 0.000000000000000000, 1.000000000000000000, 0.000000000000000000 ) ) ;
#116088 = DIRECTION ( 'NONE',  ( 0.000000000000000000, -0.9999939076577903929, 0.003490651415223739937 ) ) ;
#116089 = EDGE_CURVE ( 'NONE', #55907, #64926, #120161, .T. ) ;
#116090 = DIRECTION ( 'NONE',  ( -0.000000000000000000, -1.000000000000000000, -0.000000000000000000 ) ) ;
#116091 = EDGE_CURVE ( 'NONE', #96832, #46254, #61680, .T. ) ;
#116092 = LINE ( 'NONE', #34983, #26227 ) ;
#116093 = CIRCLE ( 'NONE', #59692, 0.09999999999999982514 ) ;
#116094 = CARTESIAN_POINT ( 'NONE',  ( 17.49862860983166257, -2.500000000000000000, -4.081131818001380474 ) ) ;
#116095 = DIRECTION ( 'NONE',  ( 0.000000000000000000, 1.000000000000000000, 0.000000000000000000 ) ) ;
#116096 = DIRECTION ( 'NONE',  ( -0.000000000000000000, -1.000000000000000000, -0.000000000000000000 ) ) ;
#116097 = CARTESIAN_POINT ( 'NONE',  ( -10.84999999999999964, 12.50000000000000000, 5.802370205355744659 ) ) ;
#116098 = CARTESIAN_POINT ( 'NONE',  ( 4.599999999999938360, 2.500000000000000000, -0.6928203230275541413 ) ) ;
#116099 = DIRECTION ( 'NONE',  ( 0.000000000000000000, 0.000000000000000000, 1.000000000000000000 ) ) ;
#116100 = ORIENTED_EDGE ( 'NONE', *, *, #115710, .T. ) ;
#116101 = VERTEX_POINT ( 'NONE', #79456 ) ;
#116102 = CIRCLE ( 'NONE', #111906, 0.06509327318403745899 ) ;
#116103 = ORIENTED_EDGE ( 'NONE', *, *, #113396, .F. ) ;
#116104 = EDGE_LOOP ( 'NONE', ( #55111, #86880 ) ) ;
#116105 = DIRECTION ( 'NONE',  ( 0.000000000000000000, 0.000000000000000000, -1.000000000000000000 ) ) ;
#116106 = ORIENTED_EDGE ( 'NONE', *, *, #95109, .T. ) ;
#116107 = CARTESIAN_POINT ( 'NONE',  ( 5.449999999999936229, 2.500000000000000000, 6.595190528383296780 ) ) ;
#116108 = ORIENTED_EDGE ( 'NONE', *, *, #45132, .F. ) ;
#116109 = ORIENTED_EDGE ( 'NONE', *, *, #113546, .F. ) ;
#116110 = DIRECTION ( 'NONE',  ( 0.000000000000000000, 1.000000000000000000, 0.000000000000000000 ) ) ;
#116112 = DIRECTION ( 'NONE',  ( 0.000000000000000000, -0.9999939076577903929, 0.003490651415223739937 ) ) ;
#116111 = PRODUCT_DEFINITION_CONTEXT ( 'detailed design', #125709, 'design' ) ;
#116113 = LINE ( 'NONE', #118045, #83477 ) ;
#116114 = CARTESIAN_POINT ( 'NONE',  ( 184.5000000000000000, 9.429780353434619030E-16, 7.699999999999999289 ) ) ;
#116115 = CARTESIAN_POINT ( 'NONE',  ( -4.600000000000028066, 12.50000000000000000, -3.572213422710612374 ) ) ;
#116116 = ORIENTED_EDGE ( 'NONE', *, *, #93787, .F. ) ;
#116117 = EDGE_LOOP ( 'NONE', ( #91118, #125305 ) ) ;
#116119 = ORIENTED_EDGE ( 'NONE', *, *, #30396, .F. ) ;
#116118 = VECTOR ( 'NONE', #40124, 1000.000000000000000 ) ;
#116120 = ORIENTED_EDGE ( 'NONE', *, *, #17796, .F. ) ;
#116121 = AXIS2_PLACEMENT_3D ( 'NONE', #81412, #112152, #121318 ) ;
#116122 = CARTESIAN_POINT ( 'NONE',  ( 5.599999999999934808, 12.50000000000000000, -4.611443907251940644 ) ) ;
#116123 = ORIENTED_EDGE ( 'NONE', *, *, #104545, .F. ) ;
#116124 = ORIENTED_EDGE ( 'NONE', *, *, #105266, .F. ) ;
#116125 = LINE ( 'NONE', #8106, #86079 ) ;
#116126 = AXIS2_PLACEMENT_3D ( 'NONE', #96327, #127733, #48539 ) ;
#116127 = EDGE_CURVE ( 'NONE', #53696, #53628, #57220, .T. ) ;
#116128 = CARTESIAN_POINT ( 'NONE',  ( -4.800000000000024691, 2.500000000000000000, 0.3464101615137735735 ) ) ;
#116129 = DIRECTION ( 'NONE',  ( -0.000000000000000000, 1.000000000000000000, -0.000000000000000000 ) ) ;
#116130 = CARTESIAN_POINT ( 'NONE',  ( -5.000000000000022204, 2.500000000000000000, -0.6928203230275541413 ) ) ;
#116131 = CARTESIAN_POINT ( 'NONE',  ( 187.3906250003414016, 0.000000000000000000, 7.564683531250000925 ) ) ;
#116132 = DIRECTION ( 'NONE',  ( 0.000000000000000000, 1.000000000000000000, 0.000000000000000000 ) ) ;
#116133 = EDGE_LOOP ( 'NONE', ( #4502, #36592 ) ) ;
#116134 = CARTESIAN_POINT ( 'NONE',  ( -12.29999999999999716, 2.500000000000000000, -4.083716857408424161 ) ) ;
#116135 = AXIS2_PLACEMENT_3D ( 'NONE', #8131, #87965, #37617 ) ;
#116136 = CIRCLE ( 'NONE', #9543, 0.09999999999999982514 ) ;
#116137 = ORIENTED_EDGE ( 'NONE', *, *, #119170, .F. ) ;
#116138 = FACE_OUTER_BOUND ( 'NONE', #29433, .T. ) ;
#116139 = ORIENTED_EDGE ( 'NONE', *, *, #86183, .F. ) ;
#116140 = CARTESIAN_POINT ( 'NONE',  ( 108.6700850095774626, 7.143942430811406119, -4.965926407314869451 ) ) ;
#116141 = CYLINDRICAL_SURFACE ( 'NONE', #80453, 1.000000000000000888 ) ;
#116142 = CIRCLE ( 'NONE', #78520, 0.1000000000000000472 ) ;
#116143 = ORIENTED_EDGE ( 'NONE', *, *, #39093, .T. ) ;
#116144 = PLANE ( 'NONE',  #88537 ) ;
#116145 = LINE ( 'NONE', #75574, #64518 ) ;
#116146 = ORIENTED_EDGE ( 'NONE', *, *, #106619, .T. ) ;
#116147 = DIRECTION ( 'NONE',  ( 0.000000000000000000, 1.000000000000000000, 0.000000000000000000 ) ) ;
#116148 = EDGE_LOOP ( 'NONE', ( #110825, #111422 ) ) ;
#116149 = ORIENTED_EDGE ( 'NONE', *, *, #22743, .T. ) ;
#116150 = CARTESIAN_POINT ( 'NONE',  ( 8.349999999999923261, 2.500000000000000000, -5.902370205355750521 ) ) ;
#116151 = CARTESIAN_POINT ( 'NONE',  ( -3.950000000000026379, 12.50000000000000000, -1.883746621131363597 ) ) ;
#116152 = CARTESIAN_POINT ( 'NONE',  ( 187.1718750003414016, 9.264065473108010111E-16, -7.564683531250000925 ) ) ;
#116153 = AXIS2_PLACEMENT_3D ( 'NONE', #108034, #118497, #1306 ) ;
#116154 = CARTESIAN_POINT ( 'NONE',  ( -1.450000000000035927, 2.500000000000000000, -1.818653347947326138 ) ) ;
#116155 = DIRECTION ( 'NONE',  ( 0.000000000000000000, 0.000000000000000000, 1.000000000000000000 ) ) ;
#116156 = DIRECTION ( 'NONE',  ( 0.000000000000000000, 0.000000000000000000, -1.000000000000000000 ) ) ;
#116157 = VECTOR ( 'NONE', #19003, 1000.000000000000000 ) ;
#116158 = CONICAL_SURFACE ( 'NONE', #63948, 0.1000000000000000472, 0.003490658503988666988 ) ;
#116159 = ORIENTED_EDGE ( 'NONE', *, *, #14034, .F. ) ;
#116160 = AXIS2_PLACEMENT_3D ( 'NONE', #102400, #123320, #71643 ) ;
#116161 = DIRECTION ( 'NONE',  ( 0.000000000000000000, 0.000000000000000000, 1.000000000000000000 ) ) ;
#116162 = EDGE_CURVE ( 'NONE', #104463, #20844, #72137, .T. ) ;
#116163 = AXIS2_PLACEMENT_3D ( 'NONE', #24305, #122510, #14460 ) ;
#116164 = ORIENTED_EDGE ( 'NONE', *, *, #5105, .F. ) ;
#116165 = EDGE_CURVE ( 'NONE', #31641, #32791, #99241, .T. ) ;
#116166 = CARTESIAN_POINT ( 'NONE',  ( 9.349999999999916156, 12.50000000000000000, 6.213873640053558134 ) ) ;
#116167 = DIRECTION ( 'NONE',  ( 0.000000000000000000, 1.000000000000000000, 0.000000000000000000 ) ) ;
#116168 = DIRECTION ( 'NONE',  ( 0.000000000000000000, 0.000000000000000000, 1.000000000000000000 ) ) ;
#116169 = ADVANCED_FACE ( 'NONE', ( #88617 ), #107615, .T. ) ;
#116170 = ORIENTED_EDGE ( 'NONE', *, *, #40699, .T. ) ;
#116171 = VECTOR ( 'NONE', #103987, 1000.000000000000000 ) ;
#116172 = AXIS2_PLACEMENT_3D ( 'NONE', #67116, #107062, #47524 ) ;
#116173 = CARTESIAN_POINT ( 'NONE',  ( -4.150000000000027889, 2.500000000000000000, -7.288010851410854585 ) ) ;
#116174 = CARTESIAN_POINT ( 'NONE',  ( -9.150000000000009237, 12.50000000000000000, -6.560283801567334372 ) ) ;
#116175 = EDGE_CURVE ( 'NONE', #62091, #94991, #29701, .T. ) ;
#116176 = EDGE_CURVE ( 'NONE', #60290, #38624, #111850, .T. ) ;
#116177 = ADVANCED_FACE ( 'NONE', ( #98416 ), #76256, .T. ) ;
#116178 = EDGE_CURVE ( 'NONE', #49457, #54499, #103440, .T. ) ;
#116179 = ORIENTED_EDGE ( 'NONE', *, *, #61725, .F. ) ;
#116180 = DIRECTION ( 'NONE',  ( -0.000000000000000000, -1.000000000000000000, -0.000000000000000000 ) ) ;
#116181 = CIRCLE ( 'NONE', #99486, 0.1000000000000002554 ) ;
#116182 = CIRCLE ( 'NONE', #126665, 0.09999999999999982514 ) ;
#116183 = ORIENTED_EDGE ( 'NONE', *, *, #28434, .T. ) ;
#116184 = B_SPLINE_CURVE_WITH_KNOTS ( 'NONE', 3,
 ( #6101, #76801, #105618, #125877, #76157, #6728, #94485, #84678 ),
 .UNSPECIFIED., .F., .F.,
 ( 4, 2, 2, 4 ),
 ( -1.045402497998345297E-05, 0.001241257413632291563, 0.001867113132938430118, 0.002492968852244568673 ),
 .UNSPECIFIED. ) ;
#116185 = ORIENTED_EDGE ( 'NONE', *, *, #57850, .T. ) ;
#116186 = CYLINDRICAL_SURFACE ( 'NONE', #63543, 7.699999999999999289 ) ;
#116187 = EDGE_CURVE ( 'NONE', #98794, #109646, #88856, .T. ) ;
#116188 = VERTEX_POINT ( 'NONE', #121301 ) ;
#116189 = DIRECTION ( 'NONE',  ( 0.000000000000000000, 1.000000000000000000, 0.000000000000000000 ) ) ;
#116190 = CARTESIAN_POINT ( 'NONE',  ( 13.29999999999989946, 12.50000000000000000, -2.385244779468109755E-15 ) ) ;
#116191 = CARTESIAN_POINT ( 'NONE',  ( 10.64999999999990976, 2.500000000000000000, -6.048780366869526581 ) ) ;
#116192 = ORIENTED_EDGE ( 'NONE', *, *, #94940, .T. ) ;
#116193 = FACE_BOUND ( 'NONE', #34665, .T. ) ;
#116195 = VERTEX_POINT ( 'NONE', #120015 ) ;
#116194 = DIRECTION ( 'NONE',  ( -0.000000000000000000, 1.000000000000000000, -0.000000000000000000 ) ) ;
#116196 = LINE ( 'NONE', #44235, #67376 ) ;
#116197 = CARTESIAN_POINT ( 'NONE',  ( -10.20000000000000462, 2.500000000000000000, 0.4464101615137735513 ) ) ;
#116198 = ORIENTED_EDGE ( 'NONE', *, *, #51175, .T. ) ;
#116199 = CONICAL_SURFACE ( 'NONE', #112118, 0.09999999999999982514, 0.003490658503988666988 ) ;
#116200 = VERTEX_POINT ( 'NONE', #22481 ) ;
#116201 = CONICAL_SURFACE ( 'NONE', #105756, 0.1000000000000002554, 0.003490658503988666988 ) ;
#116202 = EDGE_LOOP ( 'NONE', ( #63800, #106341, #113522, #105478 ) ) ;
#116203 = DIRECTION ( 'NONE',  ( 0.000000000000000000, 0.000000000000000000, 1.000000000000000000 ) ) ;
#116204 = CARTESIAN_POINT ( 'NONE',  ( -9.999999999999971578, 12.50000000000000000, -4.395220292106235327 ) ) ;
#116205 = DIRECTION ( 'NONE',  ( 0.000000000000000000, 0.000000000000000000, 1.000000000000000000 ) ) ;
#116206 = EDGE_CURVE ( 'NONE', #105571, #28898, #126425, .T. ) ;
#116207 = FACE_BOUND ( 'NONE', #51364, .T. ) ;
#116208 = ORIENTED_EDGE ( 'NONE', *, *, #52512, .T. ) ;
#116209 = CARTESIAN_POINT ( 'NONE',  ( 185.7343750003414016, 8.734944146203032389, 5.348610694689227483E-16 ) ) ;
#116210 = CARTESIAN_POINT ( 'NONE',  ( -8.550000000000011369, 2.500000000000000000, -2.511473670974877948 ) ) ;
#116211 = DIRECTION ( 'NONE',  ( 0.000000000000000000, 0.000000000000000000, 1.000000000000000000 ) ) ;
#116212 = CIRCLE ( 'NONE', #11957, 0.06509327318403745899 ) ;
#116213 = CARTESIAN_POINT ( 'NONE',  ( 6.449999999999928235, 2.500000000000000000, 2.511473670974873507 ) ) ;
#116215 = EDGE_CURVE ( 'NONE', #1788, #26160, #55409, .T. ) ;
#116214 = PLANE ( 'NONE',  #54935 ) ;
#116216 = PLANE ( 'NONE',  #15447 ) ;
#116217 = ADVANCED_FACE ( 'NONE', ( #21157 ), #80464, .T. ) ;
#116218 = FACE_OUTER_BOUND ( 'NONE', #96111, .T. ) ;
#116219 = DIRECTION ( 'NONE',  ( 0.000000000000000000, 0.000000000000000000, -1.000000000000000000 ) ) ;
#116220 = EDGE_CURVE ( 'NONE', #58440, #27222, #12623, .T. ) ;
#116221 = AXIS2_PLACEMENT_3D ( 'NONE', #82702, #104880, #73493 ) ;
#116222 = FACE_OUTER_BOUND ( 'NONE', #102064, .T. ) ;
#116223 = EDGE_CURVE ( 'NONE', #112402, #122474, #7271, .T. ) ;
#116224 = VECTOR ( 'NONE', #76045, 1000.000000000000000 ) ;
#116225 = ORIENTED_EDGE ( 'NONE', *, *, #3858, .T. ) ;
#116226 = ORIENTED_EDGE ( 'NONE', *, *, #27193, .T. ) ;
#116227 = ORIENTED_EDGE ( 'NONE', *, *, #57930, .F. ) ;
#116228 = VERTEX_POINT ( 'NONE', #110197 ) ;
#116229 = ORIENTED_EDGE ( 'NONE', *, *, #11331, .T. ) ;
#116230 = CARTESIAN_POINT ( 'NONE',  ( -8.300000000000009592, 2.500000000000000000, 4.330127018922196314 ) ) ;
#116231 = LINE ( 'NONE', #114305, #40364 ) ;
#116233 = ADVANCED_FACE ( 'NONE', ( #62393 ), #28224, .T. ) ;
#116232 = ORIENTED_EDGE ( 'NONE', *, *, #31583, .T. ) ;
#116234 = FACE_BOUND ( 'NONE', #81820, .T. ) ;
#116235 = CARTESIAN_POINT ( 'NONE',  ( -1.900000000000034106, 2.500000000000000000, -3.983716857408426293 ) ) ;
#116236 = EDGE_CURVE ( 'NONE', #14247, #105063, #44950, .T. ) ;
#116237 = EDGE_CURVE ( 'NONE', #67840, #122473, #91195, .T. ) ;
#116238 = EDGE_CURVE ( 'NONE', #22180, #31609, #7363, .T. ) ;
#116239 = CARTESIAN_POINT ( 'NONE',  ( 8.299999999999922551, 2.500000000000000000, 4.330127018922196314 ) ) ;
#116240 = FACE_OUTER_BOUND ( 'NONE', #93767, .T. ) ;
#116241 = DIRECTION ( 'NONE',  ( 0.000000000000000000, 0.000000000000000000, 1.000000000000000000 ) ) ;
#116243 = ORIENTED_EDGE ( 'NONE', *, *, #72222, .T. ) ;
#116242 = CIRCLE ( 'NONE', #49381, 0.1000000000000000472 ) ;
#116244 = CARTESIAN_POINT ( 'NONE',  ( -6.450000000000014388, 2.500000000000000000, 6.248780366869521430 ) ) ;
#116245 = EDGE_CURVE ( 'NONE', #55738, #61538, #80744, .T. ) ;
#116246 = EDGE_LOOP ( 'NONE', ( #1100, #29003, #121747, #78127 ) ) ;
#116247 = CIRCLE ( 'NONE', #11987, 0.1000000000000002554 ) ;
#116248 = ORIENTED_EDGE ( 'NONE', *, *, #64794, .F. ) ;
#116249 = ORIENTED_EDGE ( 'NONE', *, *, #118280, .F. ) ;
#116250 = DIRECTION ( 'NONE',  ( 0.000000000000000000, -0.000000000000000000, 1.000000000000000000 ) ) ;
#116251 = CARTESIAN_POINT ( 'NONE',  ( -0.2000000000000347888, 2.500000000000000000, 0.3464101615137758494 ) ) ;
#116252 = CARTESIAN_POINT ( 'NONE',  ( 13.09999999999989839, 2.500000000000000000, -0.3464101615137783474 ) ) ;
#116253 = EDGE_LOOP ( 'NONE', ( #52968, #117408, #104013, #37614 ) ) ;
#116254 = CIRCLE ( 'NONE', #41075, 0.1000000000000002554 ) ;
#116255 = CIRCLE ( 'NONE', #22295, 0.1000000000000002554 ) ;
#116256 = DIRECTION ( 'NONE',  ( 0.000000000000000000, 1.000000000000000000, 0.000000000000000000 ) ) ;
#116257 = VECTOR ( 'NONE', #49769, 1000.000000000000000 ) ;
#116258 = CARTESIAN_POINT ( 'NONE',  ( -11.25000000000000000, 2.500000000000000000, -2.757883832488650100 ) ) ;
#116259 = CARTESIAN_POINT ( 'NONE',  ( 183.9479166673494603, -6.668395609140176816, -3.850000000000003642 ) ) ;
#116260 = DIRECTION ( 'NONE',  ( 0.000000000000000000, -0.9999939076577903929, 0.003490651415223739937 ) ) ;
#116261 = DIRECTION ( 'NONE',  ( 0.000000000000000000, 1.000000000000000000, 0.000000000000000000 ) ) ;
#116262 = ORIENTED_EDGE ( 'NONE', *, *, #15276, .F. ) ;
#116263 = CARTESIAN_POINT ( 'NONE',  ( 6.249999999999928946, 2.500000000000000000, 2.857883832488649301 ) ) ;
#116264 = VECTOR ( 'NONE', #16217, 1000.000000000000000 ) ;
#116265 = VERTEX_POINT ( 'NONE', #112134 ) ;
#116267 = AXIS2_PLACEMENT_3D ( 'NONE', #98869, #68116, #108045 ) ;
#116266 = AXIS2_PLACEMENT_3D ( 'NONE', #98720, #30664, #110487 ) ;
#116268 = VERTEX_POINT ( 'NONE', #101669 ) ;
#116269 = PLANE ( 'NONE',  #55138 ) ;
#116270 = CARTESIAN_POINT ( 'NONE',  ( 9.399999999999918643, 12.50000000000000000, 0.2813168883297362810 ) ) ;
#116271 = CARTESIAN_POINT ( 'NONE',  ( -11.04999999999999893, 12.50000000000000000, 1.818653347947321475 ) ) ;
#116272 = ORIENTED_EDGE ( 'NONE', *, *, #15700, .T. ) ;
#116273 = EDGE_LOOP ( 'NONE', ( #5104, #115356, #56707, #86982 ) ) ;
#116274 = DIRECTION ( 'NONE',  ( -0.000000000000000000, 1.000000000000000000, -0.000000000000000000 ) ) ;
#116275 = EDGE_CURVE ( 'NONE', #7829, #7349, #100375, .T. ) ;
#116276 = DIRECTION ( 'NONE',  ( 0.000000000000000000, -0.000000000000000000, 1.000000000000000000 ) ) ;
#116277 = DIRECTION ( 'NONE',  ( 0.000000000000000000, -0.9999939076577903929, 0.003490651415223739937 ) ) ;
#116278 = ORIENTED_EDGE ( 'NONE', *, *, #29123, .T. ) ;
#116279 = ORIENTED_EDGE ( 'NONE', *, *, #51625, .T. ) ;
#116280 = DIRECTION ( 'NONE',  ( 0.000000000000000000, 1.000000000000000000, 0.000000000000000000 ) ) ;
#116281 = ORIENTED_EDGE ( 'NONE', *, *, #82669, .F. ) ;
#116282 = FACE_OUTER_BOUND ( 'NONE', #73638, .T. ) ;
#116283 = CARTESIAN_POINT ( 'NONE',  ( -6.249999999999981348, 2.500000000000000000, 6.495190528383297135 ) ) ;
#116284 = ORIENTED_EDGE ( 'NONE', *, *, #5673, .F. ) ;
#116285 = LINE ( 'NONE', #26634, #2189 ) ;
#116286 = PLANE ( 'NONE',  #119386 ) ;
#116287 = DIRECTION ( 'NONE',  ( 0.000000000000000000, -0.000000000000000000, 1.000000000000000000 ) ) ;
#116288 = EDGE_CURVE ( 'NONE', #40954, #32314, #15772, .T. ) ;
#116289 = LINE ( 'NONE', #37751, #54261 ) ;
#116290 = VERTEX_POINT ( 'NONE', #40832 ) ;
#116291 = CARTESIAN_POINT ( 'NONE',  ( 4.149999999999941735, 12.50000000000000000, -2.922977105672691422 ) ) ;
#116292 = AXIS2_PLACEMENT_3D ( 'NONE', #128372, #38709, #97593 ) ;
#116293 = VECTOR ( 'NONE', #127611, 1000.000000000000000 ) ;
#116294 = DIRECTION ( 'NONE',  ( -0.000000000000000000, -1.000000000000000000, -0.000000000000000000 ) ) ;
#116295 = VERTEX_POINT ( 'NONE', #52556 ) ;
#116296 = ORIENTED_EDGE ( 'NONE', *, *, #22761, .T. ) ;
#116297 = CARTESIAN_POINT ( 'NONE',  ( 185.0468750003414016, -8.734944146203032389, -1.604583208406768146E-15 ) ) ;
#116298 = CARTESIAN_POINT ( 'NONE',  ( 11.44999999999990514, 12.50000000000000000, 2.511473670974873507 ) ) ;
#116299 = CARTESIAN_POINT ( 'NONE',  ( 11.64999999999990443, 2.500000000000000000, 2.757883832488649656 ) ) ;
#116300 = CARTESIAN_POINT ( 'NONE',  ( 14.54999999999989235, 2.500000000000000000, -2.165063509461101710 ) ) ;
#116301 = DIRECTION ( 'NONE',  ( 0.000000000000000000, 0.000000000000000000, 1.000000000000000000 ) ) ;
#116304 = AXIS2_PLACEMENT_3D ( 'NONE', #101258, #29307, #90794 ) ;
#116303 = DIRECTION ( 'NONE',  ( 0.000000000000000000, 0.000000000000000000, 1.000000000000000000 ) ) ;
#116302 = CONICAL_SURFACE ( 'NONE', #118456, 0.1000000000000002554, 0.003490658503988666988 ) ;
#116305 = CARTESIAN_POINT ( 'NONE',  ( 11.84999999999990372, 12.50000000000000000, -6.148780366869526226 ) ) ;
#116306 = CARTESIAN_POINT ( 'NONE',  ( 2.699999999999945555, 2.500000000000000000, 4.083716857408420609 ) ) ;
#116307 = CARTESIAN_POINT ( 'NONE',  ( 12.94999999999989981, 12.50000000000000000, -2.230156782645139391 ) ) ;
#116308 = CARTESIAN_POINT ( 'NONE',  ( -13.09999999999999254, 2.500000000000000000, -3.883716857408423984 ) ) ;
#116310 = AXIS2_PLACEMENT_3D ( 'NONE', #51833, #31545, #102221 ) ;
#116309 = AXIS2_PLACEMENT_3D ( 'NONE', #112639, #81866, #52417 ) ;
#116311 = EDGE_LOOP ( 'NONE', ( #36974, #63134, #98039, #111574 ) ) ;
#116313 = ADVANCED_FACE ( 'NONE', ( #1515 ), #84741, .T. ) ;
#116312 = AXIS2_PLACEMENT_3D ( 'NONE', #84414, #42582, #113885 ) ;
#116314 = EDGE_LOOP ( 'NONE', ( #78913, #128859, #91891, #66692 ) ) ;
#116315 = DIRECTION ( 'NONE',  ( 0.000000000000000000, 0.000000000000000000, -1.000000000000000000 ) ) ;
#116316 = ORIENTED_EDGE ( 'NONE', *, *, #43250, .T. ) ;
#116317 = DIRECTION ( 'NONE',  ( -4.274815082592931898E-19, -0.9999939076577903929, -0.003490651415223739937 ) ) ;
#116318 = DIRECTION ( 'NONE',  ( 0.000000000000000000, 0.000000000000000000, 1.000000000000000000 ) ) ;
#116319 = LINE ( 'NONE', #16813, #73090 ) ;
#116320 = EDGE_CURVE ( 'NONE', #15804, #97447, #101013, .T. ) ;
#116321 = ORIENTED_EDGE ( 'NONE', *, *, #78534, .T. ) ;
#116322 = DIRECTION ( 'NONE',  ( 0.000000000000000000, 0.000000000000000000, 1.000000000000000000 ) ) ;
#116323 = DIRECTION ( 'NONE',  ( 1.000000000000000000, 0.000000000000000000, 0.000000000000000000 ) ) ;
#116325 = ORIENTED_EDGE ( 'NONE', *, *, #21276, .F. ) ;
#116324 = DIRECTION ( 'NONE',  ( -4.274815082592931898E-19, -0.9999939076577903929, -0.003490651415223739937 ) ) ;
#116326 = EDGE_CURVE ( 'NONE', #88048, #4024, #5306, .T. ) ;
#116327 = EDGE_CURVE ( 'NONE', #112183, #18217, #61781, .T. ) ;
#116328 = ADVANCED_FACE ( 'NONE', ( #13263 ), #53218, .T. ) ;
#116329 = ADVANCED_FACE ( 'NONE', ( #113414 ), #3460, .T. ) ;
#116330 = CIRCLE ( 'NONE', #36936, 0.06509327318403745899 ) ;
#116331 = ADVANCED_FACE ( 'NONE', ( #94403 ), #44037, .T. ) ;
#116332 = CARTESIAN_POINT ( 'NONE',  ( 8.749999999999953815, 2.500000000000000000, 6.595190528383296780 ) ) ;
#116333 = VERTEX_POINT ( 'NONE', #74785 ) ;
#116334 = CIRCLE ( 'NONE', #20504, 0.1000000000000002554 ) ;
#116335 = AXIS2_PLACEMENT_3D ( 'NONE', #7528, #50070, #89960 ) ;
#116336 = VERTEX_POINT ( 'NONE', #95069 ) ;
#116337 = ORIENTED_EDGE ( 'NONE', *, *, #74711, .F. ) ;
#116338 = ORIENTED_EDGE ( 'NONE', *, *, #37363, .F. ) ;
#116339 = DIRECTION ( 'NONE',  ( 0.000000000000000000, 0.000000000000000000, 1.000000000000000000 ) ) ;
#116340 = EDGE_CURVE ( 'NONE', #83167, #47460, #23756, .T. ) ;
#116341 = AXIS2_PLACEMENT_3D ( 'NONE', #36074, #115914, #16398 ) ;
#116342 = DIRECTION ( 'NONE',  ( 0.000000000000000000, 1.000000000000000000, 0.000000000000000000 ) ) ;
#116343 = CARTESIAN_POINT ( 'NONE',  ( -9.400000000000009237, 2.500000000000000000, -3.983716857408421852 ) ) ;
#116344 = EDGE_CURVE ( 'NONE', #83303, #104829, #55500, .T. ) ;
#116345 = DIRECTION ( 'NONE',  ( 0.000000000000000000, 0.000000000000000000, 1.000000000000000000 ) ) ;
#116347 = ORIENTED_EDGE ( 'NONE', *, *, #81028, .F. ) ;
#116346 = ADVANCED_FACE ( 'NONE', ( #114689 ), #22067, .T. ) ;
#116348 = CIRCLE ( 'NONE', #15993, 0.1000000000000002554 ) ;
#116349 = DIRECTION ( 'NONE',  ( 0.000000000000000000, 1.000000000000000000, 0.000000000000000000 ) ) ;
#116350 = ORIENTED_EDGE ( 'NONE', *, *, #51280, .T. ) ;
#116351 = CARTESIAN_POINT ( 'NONE',  ( 81.97673105564510365, -3.779183769821120809, -6.223416305047164698 ) ) ;
#116352 = FACE_OUTER_BOUND ( 'NONE', #111541, .T. ) ;
#116353 = CARTESIAN_POINT ( 'NONE',  ( 4.799999999999937650, 2.500000000000000000, -3.983716857408426293 ) ) ;
#116354 = CARTESIAN_POINT ( 'NONE',  ( 20.80581321129229977, -0.6997403544481954896, 4.161084241360361702 ) ) ;
#116355 = AXIS2_PLACEMENT_3D ( 'NONE', #49171, #9221, #9869 ) ;
#116356 = AXIS2_PLACEMENT_3D ( 'NONE', #95774, #98338, #88520 ) ;
#116357 = EDGE_LOOP ( 'NONE', ( #105562, #18779, #115905, #96424 ) ) ;
#116359 = CONICAL_SURFACE ( 'NONE', #74608, 0.1000000000000000056, 0.003490658503988666988 ) ;
#116358 = VECTOR ( 'NONE', #49506, 1000.000000000000000 ) ;
#116360 = ORIENTED_EDGE ( 'NONE', *, *, #37474, .F. ) ;
#116361 = EDGE_LOOP ( 'NONE', ( #40287, #96134, #79265, #36596 ) ) ;
#116362 = CARTESIAN_POINT ( 'NONE',  ( 11.89999999999990798, 12.50000000000000000, -3.918623584224389056 ) ) ;
#116363 = DIRECTION ( 'NONE',  ( 0.000000000000000000, 1.000000000000000000, 0.000000000000000000 ) ) ;
#116364 = DIRECTION ( 'NONE',  ( 0.000000000000000000, 0.000000000000000000, 1.000000000000000000 ) ) ;
#116365 = FACE_BOUND ( 'NONE', #23367, .T. ) ;
#116366 = DIRECTION ( 'NONE',  ( 0.000000000000000000, 0.000000000000000000, 1.000000000000000000 ) ) ;
#116367 = CARTESIAN_POINT ( 'NONE',  ( -10.60000000000000142, 2.500000000000000000, 0.3464101615137736845 ) ) ;
#116368 = CARTESIAN_POINT ( 'NONE',  ( -11.64999999999999680, 12.50000000000000000, -7.188010851410850499 ) ) ;
#116369 = DIRECTION ( 'NONE',  ( 0.000000000000000000, 1.000000000000000000, 0.000000000000000000 ) ) ;
#116370 = B_SPLINE_CURVE_WITH_KNOTS ( 'NONE', 3,
 ( #48030, #118035, #67641, #19171, #87912, #27092, #89227, #88579, #9382, #36917, #116739, #108217, #28385, #57187, #17233, #107582, #49330, #17900 ),
 .UNSPECIFIED., .F., .F.,
 ( 4, 2, 2, 2, 2, 2, 2, 2, 4 ),
 ( -1.046607274944427702E-05, 0.0004931538261984684448, 0.0009967737251463811531, 0.002004013523042207003, 0.002507633421990117760, 0.002759443371464072054, 0.003011253320938025915, 0.003514873219885932334, 0.004018493118833838321 ),
 .UNSPECIFIED. ) ;
#116372 = EDGE_CURVE ( 'NONE', #127574, #31579, #113991, .T. ) ;
#116371 = CARTESIAN_POINT ( 'NONE',  ( 184.5468750003414300, -8.734944146203032389, -1.604583208406767949E-15 ) ) ;
#116373 = DIRECTION ( 'NONE',  ( -0.000000000000000000, -1.000000000000000000, -0.000000000000000000 ) ) ;
#116374 = DIRECTION ( 'NONE',  ( 0.000000000000000000, -0.000000000000000000, 1.000000000000000000 ) ) ;
#116375 = DIRECTION ( 'NONE',  ( 0.000000000000000000, -0.000000000000000000, 1.000000000000000000 ) ) ;
#116376 = ORIENTED_EDGE ( 'NONE', *, *, #87841, .F. ) ;
#116377 = ORIENTED_EDGE ( 'NONE', *, *, #125839, .T. ) ;
#116378 = ORIENTED_EDGE ( 'NONE', *, *, #79153, .T. ) ;
#116379 = ORIENTED_EDGE ( 'NONE', *, *, #101279, .F. ) ;
#116380 = DIRECTION ( 'NONE',  ( 0.000000000000000000, 0.000000000000000000, 1.000000000000000000 ) ) ;
#116381 = EDGE_CURVE ( 'NONE', #75694, #95476, #84460, .T. ) ;
#116382 = FACE_BOUND ( 'NONE', #38105, .T. ) ;
#116383 = CARTESIAN_POINT ( 'NONE',  ( 8.749999999999918288, 12.50000000000000000, -1.537336459617587581 ) ) ;
#116384 = CARTESIAN_POINT ( 'NONE',  ( 4.349999999999941025, 2.500000000000000000, -1.818653347947326138 ) ) ;
#116385 = ADVANCED_FACE ( 'NONE', ( #93140 ), #28025, .T. ) ;
#116386 = CIRCLE ( 'NONE', #62031, 0.1000000000000002554 ) ;
#116387 = AXIS2_PLACEMENT_3D ( 'NONE', #50666, #18624, #118109 ) ;
#116388 = EDGE_CURVE ( 'NONE', #34384, #5489, #123242, .T. ) ;
#116389 = ORIENTED_EDGE ( 'NONE', *, *, #128761, .F. ) ;
#116390 = DIRECTION ( 'NONE',  ( 0.000000000000000000, 0.000000000000000000, -1.000000000000000000 ) ) ;
#116391 = LINE ( 'NONE', #107224, #104323 ) ;
#116392 = ORIENTED_EDGE ( 'NONE', *, *, #33352, .T. ) ;
#116393 = CARTESIAN_POINT ( 'NONE',  ( 10.44999999999991047, 2.500000000000000000, -6.395190528383301931 ) ) ;
#116394 = DIRECTION ( 'NONE',  ( 0.000000000000000000, 0.000000000000000000, 1.000000000000000000 ) ) ;
#116395 = ADVANCED_FACE ( 'NONE', ( #104862 ), #68014, .T. ) ;
#116396 = VECTOR ( 'NONE', #120390, 1000.000000000000000 ) ;
#116397 = ORIENTED_EDGE ( 'NONE', *, *, #48543, .F. ) ;
#116398 = FACE_OUTER_BOUND ( 'NONE', #46864, .T. ) ;
#116399 = CARTESIAN_POINT ( 'NONE',  ( 6.649999999999931077, 2.500000000000000000, -6.595190528383302109 ) ) ;
#116401 = VECTOR ( 'NONE', #113317, 1000.000000000000000 ) ;
#116400 = CONICAL_SURFACE ( 'NONE', #26627, 0.09999999999999999167, 0.003490658503988666988 ) ;
#116402 = ORIENTED_EDGE ( 'NONE', *, *, #125271, .F. ) ;
#116403 = AXIS2_PLACEMENT_3D ( 'NONE', #38848, #118653, #86617 ) ;
#116404 = CARTESIAN_POINT ( 'NONE',  ( 5.649999999999936406, 2.500000000000000000, -6.248780366869526759 ) ) ;
#116405 = PLANE ( 'NONE',  #37291 ) ;
#116406 = ORIENTED_EDGE ( 'NONE', *, *, #1697, .F. ) ;
#116407 = DIRECTION ( 'NONE',  ( 0.000000000000000000, -0.9999939076577903929, 0.003490651415223739937 ) ) ;
#116408 = ORIENTED_EDGE ( 'NONE', *, *, #5774, .T. ) ;
#116409 = ORIENTED_EDGE ( 'NONE', *, *, #70945, .F. ) ;
#116410 = DIRECTION ( 'NONE',  ( -0.000000000000000000, -1.000000000000000000, -0.000000000000000000 ) ) ;
#116411 = ADVANCED_FACE ( 'NONE', ( #115311 ), #63822, .T. ) ;
#116412 = ORIENTED_EDGE ( 'NONE', *, *, #16753, .F. ) ;
#116413 = DIRECTION ( 'NONE',  ( 0.000000000000000000, 0.000000000000000000, 1.000000000000000000 ) ) ;
#116414 = DIRECTION ( 'NONE',  ( 0.000000000000000000, 0.000000000000000000, 1.000000000000000000 ) ) ;
#116415 = VERTEX_POINT ( 'NONE', #4092 ) ;
#116416 = CARTESIAN_POINT ( 'NONE',  ( -1.850000000000033840, 2.500000000000000000, 1.818653347947321475 ) ) ;
#116417 = CARTESIAN_POINT ( 'NONE',  ( -10.84999999999999964, 2.500000000000000000, 2.857883832488649301 ) ) ;
#116418 = CARTESIAN_POINT ( 'NONE',  ( 8.299999999999922551, 2.500000000000000000, -4.230127018922201998 ) ) ;
#116419 = DIRECTION ( 'NONE',  ( 0.000000000000000000, 1.000000000000000000, 0.000000000000000000 ) ) ;
#116420 = DIRECTION ( 'NONE',  ( 0.000000000000000000, 0.000000000000000000, -1.000000000000000000 ) ) ;
#116421 = AXIS2_PLACEMENT_3D ( 'NONE', #45611, #106445, #14182 ) ;
#116423 = AXIS2_PLACEMENT_3D ( 'NONE', #86309, #36608, #95502 ) ;
#116422 = CARTESIAN_POINT ( 'NONE',  ( -0.4500000000000397571, 2.500000000000000000, -2.165063509461101710 ) ) ;
#116424 = CIRCLE ( 'NONE', #11973, 0.09999999999999982514 ) ;
#116425 = VERTEX_POINT ( 'NONE', #55142 ) ;
#116426 = EDGE_LOOP ( 'NONE', ( #45299, #85670 ) ) ;
#116427 = CARTESIAN_POINT ( 'NONE',  ( 162.5000000000000000, -0.5000000000000000000, 7.499999999999994671 ) ) ;
#116428 = CIRCLE ( 'NONE', #39104, 0.06509327318403745899 ) ;
#116429 = EDGE_CURVE ( 'NONE', #102116, #120297, #101475, .T. ) ;
#116430 = CARTESIAN_POINT ( 'NONE',  ( -6.450000000000019718, 12.50000000000000000, -6.213873640053564351 ) ) ;
#116431 = LINE ( 'NONE', #94222, #66904 ) ;
#116433 = VERTEX_POINT ( 'NONE', #76070 ) ;
#116432 = VERTEX_POINT ( 'NONE', #104238 ) ;
#116434 = EDGE_LOOP ( 'NONE', ( #98648, #18851, #10617, #67385 ) ) ;
#116435 = DIRECTION ( 'NONE',  ( -0.000000000000000000, 1.000000000000000000, -0.000000000000000000 ) ) ;
#116436 = CONICAL_SURFACE ( 'NONE', #120560, 0.1000000000000000472, 0.003490658503988666988 ) ;
#116437 = AXIS2_PLACEMENT_3D ( 'NONE', #111744, #83585, #22093 ) ;
#116438 = FACE_OUTER_BOUND ( 'NONE', #99254, .T. ) ;
#116439 = DIRECTION ( 'NONE',  ( 0.000000000000000000, 0.000000000000000000, 1.000000000000000000 ) ) ;
#116440 = CIRCLE ( 'NONE', #62092, 0.09999999999999999167 ) ;
#116441 = APPLICATION_PROTOCOL_DEFINITION ( 'draft international standard', 'automotive_design', 1998, #44700 ) ;
#116442 = FACE_OUTER_BOUND ( 'NONE', #25422, .T. ) ;
#116443 = DIRECTION ( 'NONE',  ( 0.000000000000000000, 0.000000000000000000, 1.000000000000000000 ) ) ;
#116444 = CARTESIAN_POINT ( 'NONE',  ( 10.79999999999991367, 2.500000000000000000, -2.385244779468109755E-15 ) ) ;
#116445 = CARTESIAN_POINT ( 'NONE',  ( -8.750000000000010658, 2.500000000000000000, -1.372243186433550033 ) ) ;
#116446 = DIRECTION ( 'NONE',  ( 0.000000000000000000, 0.000000000000000000, 1.000000000000000000 ) ) ;
#116447 = AXIS2_PLACEMENT_3D ( 'NONE', #5823, #85038, #115793 ) ;
#116448 = ADVANCED_FACE ( 'NONE', ( #14552 ), #118191, .T. ) ;
#116449 = DIRECTION ( 'NONE',  ( 0.000000000000000000, -0.9999939076577903929, 0.003490651415223739937 ) ) ;
#116450 = AXIS2_PLACEMENT_3D ( 'NONE', #93688, #13823, #54400 ) ;
#116451 = VERTEX_POINT ( 'NONE', #106178 ) ;
#116453 = AXIS2_PLACEMENT_3D ( 'NONE', #121559, #41747, #113037 ) ;
#116452 = AXIS2_PLACEMENT_3D ( 'NONE', #129213, #128567, #9412 ) ;
#116454 = DIRECTION ( 'NONE',  ( -0.000000000000000000, 1.000000000000000000, -0.000000000000000000 ) ) ;
#116455 = ORIENTED_EDGE ( 'NONE', *, *, #65947, .T. ) ;
#116456 = ORIENTED_EDGE ( 'NONE', *, *, #73254, .F. ) ;
#116457 = FACE_OUTER_BOUND ( 'NONE', #90381, .T. ) ;
#116458 = CARTESIAN_POINT ( 'NONE',  ( 3.149999999999942624, 2.500000000000000000, 6.841600689897072485 ) ) ;
#116459 = CARTESIAN_POINT ( 'NONE',  ( 12.49999999999990585, 2.500000000000000000, -4.922947341949753586 ) ) ;
#116460 = CARTESIAN_POINT ( 'NONE',  ( -4.999999999999986677, 2.500000000000000000, 0.09999999999999772959 ) ) ;
#116461 = FACE_OUTER_BOUND ( 'NONE', #61368, .T. ) ;
#116462 = CARTESIAN_POINT ( 'NONE',  ( -7.700000000000016165, 12.50000000000000000, -3.983716857408426293 ) ) ;
#116463 = FACE_OUTER_BOUND ( 'NONE', #67777, .T. ) ;
#116464 = VERTEX_POINT ( 'NONE', #15845 ) ;
#116465 = FACE_OUTER_BOUND ( 'NONE', #72424, .T. ) ;
#116466 = CIRCLE ( 'NONE', #106104, 0.1000000000000002554 ) ;
#116467 = FACE_OUTER_BOUND ( 'NONE', #90760, .T. ) ;
#116468 = ORIENTED_EDGE ( 'NONE', *, *, #51166, .T. ) ;
#116469 = EDGE_LOOP ( 'NONE', ( #95713, #17188 ) ) ;
#116470 = EDGE_CURVE ( 'NONE', #28339, #82935, #47107, .T. ) ;
#116471 = ORIENTED_EDGE ( 'NONE', *, *, #79630, .T. ) ;
#116472 = ORIENTED_EDGE ( 'NONE', *, *, #115648, .F. ) ;
#116473 = ORIENTED_EDGE ( 'NONE', *, *, #96261, .F. ) ;
#116474 = CARTESIAN_POINT ( 'NONE',  ( 142.3152275665817115, 2.500000000000000000, 2.763522878056728693 ) ) ;
#116475 = DIRECTION ( 'NONE',  ( -0.000000000000000000, -1.000000000000000000, -0.000000000000000000 ) ) ;
#116476 = ADVANCED_FACE ( 'NONE', ( #16478 ), #43406, .T. ) ;
#116477 = EDGE_LOOP ( 'NONE', ( #113212, #28737 ) ) ;
#116478 = AXIS2_PLACEMENT_3D ( 'NONE', #53650, #3899, #43854 ) ;
#116479 = DIRECTION ( 'NONE',  ( -0.000000000000000000, 1.000000000000000000, -0.000000000000000000 ) ) ;
#116481 = CARTESIAN_POINT ( 'NONE',  ( -11.89999999999999503, 2.500000000000000000, 4.776537180435972196 ) ) ;
#116480 = AXIS2_PLACEMENT_3D ( 'NONE', #112169, #63715, #61793 ) ;
#116482 = DIRECTION ( 'NONE',  ( 0.000000000000000000, 0.000000000000000000, 1.000000000000000000 ) ) ;
#116483 = ORIENTED_EDGE ( 'NONE', *, *, #22622, .F. ) ;
#116484 = EDGE_CURVE ( 'NONE', #9001, #37856, #56416, .T. ) ;
#116485 = EDGE_CURVE ( 'NONE', #32461, #10213, #37445, .T. ) ;
#116486 = ADVANCED_FACE ( 'NONE', ( #117912 ), #48545, .T. ) ;
#116487 = CARTESIAN_POINT ( 'NONE',  ( -0.8500000000000390576, 2.500000000000000000, -2.065063509461102065 ) ) ;
#116488 = EDGE_CURVE ( 'NONE', #45295, #32793, #109791, .T. ) ;
#116490 = AXIS2_PLACEMENT_3D ( 'NONE', #60175, #100086, #88974 ) ;
#116489 = AXIS2_PLACEMENT_3D ( 'NONE', #59403, #110400, #128122 ) ;
#116491 = DIRECTION ( 'NONE',  ( -4.274815082592931898E-19, -0.9999939076577903929, -0.003490651415223739937 ) ) ;
#116492 = ORIENTED_EDGE ( 'NONE', *, *, #97851, .T. ) ;
#116493 = CONICAL_SURFACE ( 'NONE', #91457, 0.09999999999999982514, 0.003490658503988666988 ) ;
#116494 = VERTEX_POINT ( 'NONE', #127113 ) ;
#116496 = EDGE_LOOP ( 'NONE', ( #12874, #72405 ) ) ;
#116495 = EDGE_CURVE ( 'NONE', #123810, #65564, #11291, .T. ) ;
#116497 = DIRECTION ( 'NONE',  ( -0.000000000000000000, -1.000000000000000000, -0.000000000000000000 ) ) ;
#116498 = EDGE_CURVE ( 'NONE', #124819, #50249, #116040, .T. ) ;
#116499 = ADVANCED_FACE ( 'NONE', ( #47264 ), #26973, .T. ) ;
#116500 = AXIS2_PLACEMENT_3D ( 'NONE', #95462, #115735, #65339 ) ;
#116501 = DIRECTION ( 'NONE',  ( 0.000000000000000000, 0.000000000000000000, -1.000000000000000000 ) ) ;
#116502 = EDGE_CURVE ( 'NONE', #25999, #92156, #96333, .T. ) ;
#116503 = AXIS2_PLACEMENT_3D ( 'NONE', #32881, #34817, #14482 ) ;
#116504 = EDGE_CURVE ( 'NONE', #3741, #107010, #126514, .T. ) ;
#116505 = ORIENTED_EDGE ( 'NONE', *, *, #39922, .T. ) ;
#116506 = CARTESIAN_POINT ( 'NONE',  ( -1.850000000000033396, 2.500000000000000000, -2.511473670974877948 ) ) ;
#116507 = DIRECTION ( 'NONE',  ( -4.274815082592931898E-19, -0.9999939076577903929, -0.003490651415223739937 ) ) ;
#116508 = DIRECTION ( 'NONE',  ( 0.000000000000000000, 1.000000000000000000, 0.000000000000000000 ) ) ;
#116509 = DIRECTION ( 'NONE',  ( -4.274815082592931898E-19, -0.9999939076577903929, -0.003490651415223739937 ) ) ;
#116510 = EDGE_CURVE ( 'NONE', #119603, #4736, #90877, .T. ) ;
#116511 = ORIENTED_EDGE ( 'NONE', *, *, #96520, .T. ) ;
#116512 = CARTESIAN_POINT ( 'NONE',  ( 14.34999999999989306, 12.50000000000000000, -2.446380397790840266 ) ) ;
#116513 = CONICAL_SURFACE ( 'NONE', #114461, 0.09999999999999982514, 0.003490658503988666988 ) ;
#116514 = VERTEX_POINT ( 'NONE', #17777 ) ;
#116515 = EDGE_LOOP ( 'NONE', ( #115119, #49094, #110332, #9956 ) ) ;
#116516 = EDGE_LOOP ( 'NONE', ( #50243, #129516 ) ) ;
#116517 = CARTESIAN_POINT ( 'NONE',  ( 11.24999999999991118, 2.500000000000000000, 5.702370205355745014 ) ) ;
#116518 = FACE_BOUND ( 'NONE', #8970, .T. ) ;
#116519 = CIRCLE ( 'NONE', #14106, 0.1000000000000000472 ) ;
#116520 = CARTESIAN_POINT ( 'NONE',  ( 186.0312500006828031, 9.429780353434619030E-16, -7.700000000000000178 ) ) ;
#116521 = DIRECTION ( 'NONE',  ( 0.000000000000000000, 1.000000000000000000, 0.000000000000000000 ) ) ;
#116522 = CIRCLE ( 'NONE', #47590, 0.1000000000000000056 ) ;
#116523 = CARTESIAN_POINT ( 'NONE',  ( 0.6499999999999543920, 2.500000000000000000, 6.741600689897071952 ) ) ;
#116524 = CIRCLE ( 'NONE', #127008, 0.06509327318403745899 ) ;
#116525 = ORIENTED_EDGE ( 'NONE', *, *, #59202, .F. ) ;
#116526 = CARTESIAN_POINT ( 'NONE',  ( 13.09999999999990195, 12.50000000000000000, 4.048810130592458201 ) ) ;
#116527 = DIRECTION ( 'NONE',  ( -0.000000000000000000, 1.000000000000000000, -0.000000000000000000 ) ) ;
#116529 = CARTESIAN_POINT ( 'NONE',  ( 16.87640210516335415, 2.500000000000000000, 4.436424697255048955 ) ) ;
#116528 = AXIS2_PLACEMENT_3D ( 'NONE', #1622, #29177, #50732 ) ;
#116531 = DIRECTION ( 'NONE',  ( 0.000000000000000000, 0.000000000000000000, -1.000000000000000000 ) ) ;
#116530 = AXIS2_PLACEMENT_3D ( 'NONE', #58637, #109662, #8856 ) ;
#116532 = EDGE_LOOP ( 'NONE', ( #26980, #25867 ) ) ;
#116533 = DIRECTION ( 'NONE',  ( -0.000000000000000000, 1.000000000000000000, -0.000000000000000000 ) ) ;
#116534 = AXIS2_PLACEMENT_3D ( 'NONE', #41484, #33427, #29078 ) ;
#116535 = CIRCLE ( 'NONE', #70478, 0.06509327318403745899 ) ;
#116536 = CARTESIAN_POINT ( 'NONE',  ( 1.699999999999951994, 2.500000000000000000, -4.230127018922201998 ) ) ;
#116537 = ORIENTED_EDGE ( 'NONE', *, *, #48069, .T. ) ;
#116538 = DIRECTION ( 'NONE',  ( 0.000000000000000000, 1.000000000000000000, 0.000000000000000000 ) ) ;
#116539 = CIRCLE ( 'NONE', #101884, 0.1000000000000000472 ) ;
#116540 = DIRECTION ( 'NONE',  ( -0.000000000000000000, 1.000000000000000000, -0.000000000000000000 ) ) ;
#116541 = FACE_BOUND ( 'NONE', #119227, .T. ) ;
#116542 = CARTESIAN_POINT ( 'NONE',  ( 2.500000000000002220, -2.500000000000000000, -8.999999999999998224 ) ) ;
#116543 = EDGE_CURVE ( 'NONE', #117070, #71126, #103528, .T. ) ;
#116544 =( GEOMETRIC_REPRESENTATION_CONTEXT ( 3 ) GLOBAL_UNCERTAINTY_ASSIGNED_CONTEXT ( ( #6047 ) ) GLOBAL_UNIT_ASSIGNED_CONTEXT ( ( #11976, #70266, #1508 ) ) REPRESENTATION_CONTEXT ( 'NONE', 'WORKASPACE' ) );
#116545 = ORIENTED_EDGE ( 'NONE', *, *, #128060, .F. ) ;
#116546 = DIRECTION ( 'NONE',  ( -0.000000000000000000, -1.000000000000000000, -0.000000000000000000 ) ) ;
#116547 = EDGE_CURVE ( 'NONE', #41996, #23306, #57565, .T. ) ;
#116548 = EDGE_LOOP ( 'NONE', ( #90857, #97347 ) ) ;
#116549 = ORIENTED_EDGE ( 'NONE', *, *, #9115, .F. ) ;
#116550 = FACE_OUTER_BOUND ( 'NONE', #68549, .T. ) ;
#116551 = CARTESIAN_POINT ( 'NONE',  ( 187.1666666666666856, -6.668395609140176816, -3.850000000000003642 ) ) ;
#116552 = VERTEX_POINT ( 'NONE', #18434 ) ;
#116553 = DIRECTION ( 'NONE',  ( 0.000000000000000000, 0.000000000000000000, 1.000000000000000000 ) ) ;
#116554 = FACE_OUTER_BOUND ( 'NONE', #106534, .T. ) ;
#116555 = EDGE_CURVE ( 'NONE', #48757, #109936, #116625, .T. ) ;
#116556 = CARTESIAN_POINT ( 'NONE',  ( 7.499999999999961808, 2.500000000000000000, -4.330127018922201643 ) ) ;
#116557 = DIRECTION ( 'NONE',  ( 0.000000000000000000, 0.000000000000000000, 1.000000000000000000 ) ) ;
#116558 = AXIS2_PLACEMENT_3D ( 'NONE', #39677, #48838, #119485 ) ;
#116559 = ORIENTED_EDGE ( 'NONE', *, *, #27340, .F. ) ;
#116560 = CARTESIAN_POINT ( 'NONE',  ( 5.849999999999933920, 2.500000000000000000, 6.495190528383297135 ) ) ;
#116561 = DIRECTION ( 'NONE',  ( -0.000000000000000000, -1.000000000000000000, -0.000000000000000000 ) ) ;
#116562 = DIRECTION ( 'NONE',  ( 0.000000000000000000, 0.000000000000000000, -1.000000000000000000 ) ) ;
#116563 = CARTESIAN_POINT ( 'NONE',  ( 21.25104915411511897, 0.2454763298552203044, -4.189301388123448433 ) ) ;
#116564 = ORIENTED_EDGE ( 'NONE', *, *, #88571, .F. ) ;
#116565 = DIRECTION ( 'NONE',  ( -0.000000000000000000, 1.000000000000000000, -0.000000000000000000 ) ) ;
#116566 = ORIENTED_EDGE ( 'NONE', *, *, #117412, .F. ) ;
#116567 = CARTESIAN_POINT ( 'NONE',  ( -3.350000000000032507, 12.50000000000000000, -6.430097255199264339 ) ) ;
#116568 = DIRECTION ( 'NONE',  ( 0.000000000000000000, 1.000000000000000000, 0.000000000000000000 ) ) ;
#116569 = VERTEX_POINT ( 'NONE', #11011 ) ;
#116570 = DIRECTION ( 'NONE',  ( 0.000000000000000000, 0.000000000000000000, 1.000000000000000000 ) ) ;
#116571 = FACE_OUTER_BOUND ( 'NONE', #11621, .T. ) ;
#116572 = AXIS2_PLACEMENT_3D ( 'NONE', #39531, #99719, #107597 ) ;
#116573 = CARTESIAN_POINT ( 'NONE',  ( 9.349999999999916156, 2.500000000000000000, 6.741600689897071952 ) ) ;
#116574 = AXIS2_PLACEMENT_3D ( 'NONE', #22361, #91077, #43287 ) ;
#116575 = DIRECTION ( 'NONE',  ( -4.274815082592931898E-19, -0.9999939076577903929, -0.003490651415223739937 ) ) ;
#116576 = ORIENTED_EDGE ( 'NONE', *, *, #58245, .F. ) ;
#116577 = CARTESIAN_POINT ( 'NONE',  ( -15.59999999999998010, 12.50000000000000000, 0.2813168883297385570 ) ) ;
#116578 = DIRECTION ( 'NONE',  ( -4.274815082592931898E-19, -0.9999939076577903929, -0.003490651415223739937 ) ) ;
#116579 = FACE_OUTER_BOUND ( 'NONE', #27618, .T. ) ;
#116580 = CARTESIAN_POINT ( 'NONE',  ( 3.949999999999939782, 2.500000000000000000, 2.611473670974873151 ) ) ;
#116581 = DIRECTION ( 'NONE',  ( 0.000000000000000000, 0.000000000000000000, 1.000000000000000000 ) ) ;
#116582 = AXIS2_PLACEMENT_3D ( 'NONE', #116774, #6795, #46764 ) ;
#116583 = ADVANCED_FACE ( 'NONE', ( #38076 ), #109601, .T. ) ;
#116584 = VERTEX_POINT ( 'NONE', #67509 ) ;
#116586 = ORIENTED_EDGE ( 'NONE', *, *, #14187, .F. ) ;
#116585 = CIRCLE ( 'NONE', #83450, 0.06509327318403745899 ) ;
#116587 = CARTESIAN_POINT ( 'NONE',  ( 7.949999999999922018, 12.50000000000000000, 6.495190528383297135 ) ) ;
#116588 = ORIENTED_EDGE ( 'NONE', *, *, #50577, .T. ) ;
#116589 = DIRECTION ( 'NONE',  ( 0.000000000000000000, 0.000000000000000000, -1.000000000000000000 ) ) ;
#116591 = VERTEX_POINT ( 'NONE', #107457 ) ;
#116590 = VERTEX_POINT ( 'NONE', #81071 ) ;
#116592 = ORIENTED_EDGE ( 'NONE', *, *, #51226, .T. ) ;
#116593 = DIRECTION ( 'NONE',  ( 0.000000000000000000, 0.000000000000000000, -1.000000000000000000 ) ) ;
#116595 = FACE_OUTER_BOUND ( 'NONE', #81125, .T. ) ;
#116594 = AXIS2_PLACEMENT_3D ( 'NONE', #122535, #113344, #23683 ) ;
#116596 = CARTESIAN_POINT ( 'NONE',  ( -14.19999999999998685, 12.50000000000000000, -1.084202172485504434E-16 ) ) ;
#116597 =( NAMED_UNIT ( * ) PLANE_ANGLE_UNIT ( ) SI_UNIT ( $, .RADIAN. ) );
#116598 = FACE_OUTER_BOUND ( 'NONE', #16325, .T. ) ;
#116599 = DIRECTION ( 'NONE',  ( 0.000000000000000000, 1.000000000000000000, 0.000000000000000000 ) ) ;
#116600 = ADVANCED_FACE ( 'NONE', ( #66878 ), #21776, .T. ) ;
#116601 = LINE ( 'NONE', #78643, #120798 ) ;
#116602 = AXIS2_PLACEMENT_3D ( 'NONE', #129236, #57904, #99757 ) ;
#116603 = ORIENTED_EDGE ( 'NONE', *, *, #49537, .F. ) ;
#116604 = EDGE_CURVE ( 'NONE', #14341, #62130, #5021, .T. ) ;
#116605 = FACE_OUTER_BOUND ( 'NONE', #34947, .T. ) ;
#116606 = ORIENTED_EDGE ( 'NONE', *, *, #15969, .F. ) ;
#116607 = AXIS2_PLACEMENT_3D ( 'NONE', #30909, #30268, #89805 ) ;
#116608 = ORIENTED_EDGE ( 'NONE', *, *, #44334, .F. ) ;
#116609 = ORIENTED_EDGE ( 'NONE', *, *, #91858, .F. ) ;
#116610 = ORIENTED_EDGE ( 'NONE', *, *, #57203, .T. ) ;
#116611 = DIRECTION ( 'NONE',  ( 0.000000000000000000, -0.000000000000000000, 1.000000000000000000 ) ) ;
#116612 = ORIENTED_EDGE ( 'NONE', *, *, #76371, .F. ) ;
#116613 = EDGE_CURVE ( 'NONE', #119461, #86952, #70599, .T. ) ;
#116614 = ORIENTED_EDGE ( 'NONE', *, *, #10966, .F. ) ;
#116615 = AXIS2_PLACEMENT_3D ( 'NONE', #125925, #36296, #76205 ) ;
#116616 = CONICAL_SURFACE ( 'NONE', #64386, 0.1000000000000002554, 0.003490658503988666988 ) ;
#116617 = LINE ( 'NONE', #27581, #68609 ) ;
#116619 = VECTOR ( 'NONE', #73521, 1000.000000000000000 ) ;
#116618 = DIRECTION ( 'NONE',  ( -4.274815082592931898E-19, -0.9999939076577903929, -0.003490651415223739937 ) ) ;
#116620 = CARTESIAN_POINT ( 'NONE',  ( -10.40000000000000213, 12.50000000000000000, -0.6928203230275541413 ) ) ;
#116621 = DIRECTION ( 'NONE',  ( -0.000000000000000000, -1.000000000000000000, -0.000000000000000000 ) ) ;
#116622 = LINE ( 'NONE', #108090, #13273 ) ;
#116623 = ORIENTED_EDGE ( 'NONE', *, *, #103502, .F. ) ;
#116624 = AXIS2_PLACEMENT_3D ( 'NONE', #119308, #88562, #99694 ) ;
#116626 = CONICAL_SURFACE ( 'NONE', #126815, 0.09999999999999982514, 0.003490658503988666988 ) ;
#116625 = LINE ( 'NONE', #87801, #34593 ) ;
#116627 = ORIENTED_EDGE ( 'NONE', *, *, #95414, .F. ) ;
#116628 = AXIS2_PLACEMENT_3D ( 'NONE', #76445, #88831, #122010 ) ;
#116629 = DIRECTION ( 'NONE',  ( 0.000000000000000000, -0.000000000000000000, 1.000000000000000000 ) ) ;
#116630 = EDGE_LOOP ( 'NONE', ( #7445, #78377, #122916, #126449 ) ) ;
#116631 = DIRECTION ( 'NONE',  ( -0.000000000000000000, 1.000000000000000000, -0.000000000000000000 ) ) ;
#116632 = ORIENTED_EDGE ( 'NONE', *, *, #63034, .F. ) ;
#116633 = AXIS2_PLACEMENT_3D ( 'NONE', #75705, #6306, #43709 ) ;
#116634 = EDGE_LOOP ( 'NONE', ( #30436, #46160 ) ) ;
#116635 = CARTESIAN_POINT ( 'NONE',  ( -13.34999999999999076, 2.500000000000000000, 1.572243186433549544 ) ) ;
#116636 = CARTESIAN_POINT ( 'NONE',  ( -0.2000000000000339284, 2.500000000000000000, -0.3464101615137759604 ) ) ;
#116637 = ADVANCED_FACE ( 'NONE', ( #43739 ), #124264, .T. ) ;
#116639 = CIRCLE ( 'NONE', #125049, 0.1000000000000000472 ) ;
#116638 = AXIS2_PLACEMENT_3D ( 'NONE', #96983, #47256, #20847 ) ;
#116640 = CARTESIAN_POINT ( 'NONE',  ( -0.8500000000000382805, 12.50000000000000000, -2.792790559304616504 ) ) ;
#116641 = FACE_OUTER_BOUND ( 'NONE', #13550, .T. ) ;
#116642 = DIRECTION ( 'NONE',  ( 0.000000000000000000, 1.000000000000000000, 0.000000000000000000 ) ) ;
#116643 = ORIENTED_EDGE ( 'NONE', *, *, #97120, .T. ) ;
#116644 = LINE ( 'NONE', #7976, #1761 ) ;
#116645 = DIRECTION ( 'NONE',  ( -0.000000000000000000, 1.000000000000000000, -0.000000000000000000 ) ) ;
#116646 = EDGE_CURVE ( 'NONE', #73230, #24288, #2479, .T. ) ;
#116647 = DIRECTION ( 'NONE',  ( 0.000000000000000000, 0.000000000000000000, -1.000000000000000000 ) ) ;
#116648 = CARTESIAN_POINT ( 'NONE',  ( -7.500000000000013323, 2.500000000000000000, 5.022947341949748790 ) ) ;
#116649 = ADVANCED_FACE ( 'NONE', ( #22165 ), #11385, .T. ) ;
#116650 = DIRECTION ( 'NONE',  ( -0.000000000000000000, -1.000000000000000000, -0.000000000000000000 ) ) ;
#116651 = ORIENTED_EDGE ( 'NONE', *, *, #51846, .T. ) ;
#116652 = EDGE_LOOP ( 'NONE', ( #89507, #24751 ) ) ;
#116653 = EDGE_CURVE ( 'NONE', #55973, #108239, #111653, .T. ) ;
#116654 = EDGE_CURVE ( 'NONE', #20003, #6508, #88661, .T. ) ;
#116655 = CARTESIAN_POINT ( 'NONE',  ( 8.749999999999923617, 2.500000000000000000, -7.188010851410854052 ) ) ;
#116656 = ADVANCED_FACE ( 'NONE', ( #103287 ), #3154, .T. ) ;
#116657 = EDGE_LOOP ( 'NONE', ( #47906, #49831 ) ) ;
#116658 = DIRECTION ( 'NONE',  ( 0.000000000000000000, -0.9999939076577903929, 0.003490651415223739937 ) ) ;
#116659 = CARTESIAN_POINT ( 'NONE',  ( 4.349999999999936584, 12.50000000000000000, 6.148780366869520009 ) ) ;
#116660 = EDGE_CURVE ( 'NONE', #6759, #42690, #61584, .T. ) ;
#116661 = CIRCLE ( 'NONE', #18991, 0.06509327318403745899 ) ;
#116662 = VERTEX_POINT ( 'NONE', #113754 ) ;
#116663 = CARTESIAN_POINT ( 'NONE',  ( 184.5833333333333144, -6.668395609140180369, 3.849999999999994760 ) ) ;
#116664 = CARTESIAN_POINT ( 'NONE',  ( 3.099999999999945022, 12.50000000000000000, -0.3464101615137783474 ) ) ;
#116665 = DIRECTION ( 'NONE',  ( 0.000000000000000000, -0.000000000000000000, 1.000000000000000000 ) ) ;
#116666 = FACE_OUTER_BOUND ( 'NONE', #122713, .T. ) ;
#116667 = DIRECTION ( 'NONE',  ( -0.000000000000000000, -1.000000000000000000, -0.000000000000000000 ) ) ;
#116668 = EDGE_LOOP ( 'NONE', ( #68421, #107222 ) ) ;
#116669 = EDGE_CURVE ( 'NONE', #82548, #108166, #59440, .T. ) ;
#116670 = AXIS2_PLACEMENT_3D ( 'NONE', #73158, #93439, #111797 ) ;
#116671 = CARTESIAN_POINT ( 'NONE',  ( -14.59999999999998366, 12.50000000000000000, -1.084202172485504434E-16 ) ) ;
#116672 = DIRECTION ( 'NONE',  ( 0.000000000000000000, -0.9999939076577903929, 0.003490651415223739937 ) ) ;
#116673 = EDGE_LOOP ( 'NONE', ( #74293, #96219, #31946, #11798 ) ) ;
#116674 = DIRECTION ( 'NONE',  ( 0.000000000000000000, 0.000000000000000000, -1.000000000000000000 ) ) ;
#116675 = DIRECTION ( 'NONE',  ( -4.274815082592931898E-19, -0.9999939076577903929, -0.003490651415223739937 ) ) ;
#116676 = AXIS2_PLACEMENT_3D ( 'NONE', #8344, #97375, #118949 ) ;
#116677 = LINE ( 'NONE', #98317, #26122 ) ;
#116678 = AXIS2_PLACEMENT_3D ( 'NONE', #43154, #111200, #62777 ) ;
#116679 = EDGE_LOOP ( 'NONE', ( #107690, #17768 ) ) ;
#116680 = DIRECTION ( 'NONE',  ( -0.000000000000000000, -1.000000000000000000, -0.000000000000000000 ) ) ;
#116681 = VERTEX_POINT ( 'NONE', #81696 ) ;
#116682 = FACE_OUTER_BOUND ( 'NONE', #44996, .T. ) ;
#116683 = LINE ( 'NONE', #125227, #121974 ) ;
#116684 = CARTESIAN_POINT ( 'NONE',  ( 7.099999999999926814, 12.50000000000000000, -2.276824562219559311E-15 ) ) ;
#116685 = VERTEX_POINT ( 'NONE', #94101 ) ;
#116686 = AXIS2_PLACEMENT_3D ( 'NONE', #74562, #123640, #83107 ) ;
#116687 = FACE_OUTER_BOUND ( 'NONE', #93149, .T. ) ;
#116688 = CARTESIAN_POINT ( 'NONE',  ( 11.84999999999990372, 2.500000000000000000, -6.148780366869526226 ) ) ;
#116689 = VERTEX_POINT ( 'NONE', #92161 ) ;
#116690 = ORIENTED_EDGE ( 'NONE', *, *, #1946, .F. ) ;
#116691 = DIRECTION ( 'NONE',  ( 0.000000000000000000, 1.000000000000000000, 0.000000000000000000 ) ) ;
#116692 = AXIS2_PLACEMENT_3D ( 'NONE', #51618, #32644, #81701 ) ;
#116693 = ADVANCED_FACE ( 'NONE', ( #13591 ), #28120, .T. ) ;
#116694 = EDGE_LOOP ( 'NONE', ( #127665, #939, #66276, #21293 ) ) ;
#116695 = COLOUR_RGB ( '', 0.40784314, 0.44705882, 0.49803922) ;
#116696 = DIRECTION ( 'NONE',  ( 0.000000000000000000, 1.000000000000000000, 0.000000000000000000 ) ) ;
#116697 = DIRECTION ( 'NONE',  ( 0.000000000000000000, 1.000000000000000000, 0.000000000000000000 ) ) ;
#116698 = ORIENTED_EDGE ( 'NONE', *, *, #35573, .T. ) ;
#116699 = ORIENTED_EDGE ( 'NONE', *, *, #59793, .T. ) ;
#116700 = DIRECTION ( 'NONE',  ( -0.000000000000000000, -1.000000000000000000, -0.000000000000000000 ) ) ;
#116701 = LINE ( 'NONE', #25104, #19207 ) ;
#116702 = AXIS2_PLACEMENT_3D ( 'NONE', #360, #21302, #51439 ) ;
#116703 = VERTEX_POINT ( 'NONE', #43100 ) ;
#116704 = EDGE_CURVE ( 'NONE', #93541, #103724, #121616, .T. ) ;
#116705 = DIRECTION ( 'NONE',  ( -0.000000000000000000, 1.000000000000000000, -0.000000000000000000 ) ) ;
#116706 = DIRECTION ( 'NONE',  ( -0.000000000000000000, -1.000000000000000000, -0.000000000000000000 ) ) ;
#116707 = VECTOR ( 'NONE', #89147, 1000.000000000000000 ) ;
#116708 = CARTESIAN_POINT ( 'NONE',  ( 8.299999999999922551, 2.500000000000000000, 4.230127018922196669 ) ) ;
#116709 = LINE ( 'NONE', #68254, #38371 ) ;
#116710 = DIRECTION ( 'NONE',  ( 0.000000000000000000, 0.000000000000000000, 1.000000000000000000 ) ) ;
#116711 = CARTESIAN_POINT ( 'NONE',  ( 10.39999999999991509, 12.50000000000000000, -0.6928203230275542523 ) ) ;
#116712 = CONICAL_SURFACE ( 'NONE', #60317, 0.1000000000000002554, 0.003490658503988666988 ) ;
#116713 = EDGE_LOOP ( 'NONE', ( #112439, #120643 ) ) ;
#116714 = ORIENTED_EDGE ( 'NONE', *, *, #112419, .F. ) ;
#116715 = ORIENTED_EDGE ( 'NONE', *, *, #116660, .F. ) ;
#116716 = ORIENTED_EDGE ( 'NONE', *, *, #17651, .F. ) ;
#116717 = DIRECTION ( 'NONE',  ( 0.000000000000000000, 1.000000000000000000, 0.000000000000000000 ) ) ;
#116718 = FACE_OUTER_BOUND ( 'NONE', #12164, .T. ) ;
#116719 = DIRECTION ( 'NONE',  ( 0.000000000000000000, 0.000000000000000000, 1.000000000000000000 ) ) ;
#116720 = AXIS2_PLACEMENT_3D ( 'NONE', #13833, #24312, #81305 ) ;
#116721 = EDGE_LOOP ( 'NONE', ( #45449, #48483, #22123, #79325 ) ) ;
#116722 = FACE_BOUND ( 'NONE', #99059, .T. ) ;
#116723 = LINE ( 'NONE', #79402, #56286 ) ;
#116724 = CARTESIAN_POINT ( 'NONE',  ( 8.099999999999923261, 2.500000000000000000, 4.776537180435972196 ) ) ;
#116725 = CARTESIAN_POINT ( 'NONE',  ( 7.699999999999925571, 2.500000000000000000, 3.983716857408420076 ) ) ;
#116726 = VECTOR ( 'NONE', #89594, 1000.000000000000000 ) ;
#116727 = DIRECTION ( 'NONE',  ( -0.000000000000000000, -1.000000000000000000, -0.000000000000000000 ) ) ;
#116728 = DIRECTION ( 'NONE',  ( 0.000000000000000000, 0.000000000000000000, 1.000000000000000000 ) ) ;
#116729 = CARTESIAN_POINT ( 'NONE',  ( -8.350000000000012079, 12.50000000000000000, 1.472243186433545459 ) ) ;
#116730 = CARTESIAN_POINT ( 'NONE',  ( -7.500000000000016875, 2.500000000000000000, 0.6928203230275494784 ) ) ;
#116731 = CARTESIAN_POINT ( 'NONE',  ( 9.799999999999918998, 2.500000000000000000, -0.3464101615137782364 ) ) ;
#116732 = DIRECTION ( 'NONE',  ( 0.000000000000000000, 0.000000000000000000, 1.000000000000000000 ) ) ;
#116733 = CARTESIAN_POINT ( 'NONE',  ( -8.750000000000005329, 2.500000000000000000, 5.902370205355745192 ) ) ;
#116734 = EDGE_CURVE ( 'NONE', #120381, #24974, #128400, .T. ) ;
#116735 = ORIENTED_EDGE ( 'NONE', *, *, #127155, .T. ) ;
#116736 = ORIENTED_EDGE ( 'NONE', *, *, #48690, .T. ) ;
#116737 = ORIENTED_EDGE ( 'NONE', *, *, #62871, .F. ) ;
#116738 = ORIENTED_EDGE ( 'NONE', *, *, #123069, .F. ) ;
#116739 = CARTESIAN_POINT ( 'NONE',  ( 17.49100792770858703, -2.144659849949841490, -4.220823783475863955 ) ) ;
#116740 = AXIS2_PLACEMENT_3D ( 'NONE', #39945, #70682, #79851 ) ;
#116741 = CARTESIAN_POINT ( 'NONE',  ( 1.249999999999988454, 12.50000000000000000, 2.099970236277060032 ) ) ;
#116743 = VERTEX_POINT ( 'NONE', #31975 ) ;
#116742 = EDGE_LOOP ( 'NONE', ( #109778, #76957, #107025, #40531 ) ) ;
#116744 = ORIENTED_EDGE ( 'NONE', *, *, #118786, .F. ) ;
#116745 = DIRECTION ( 'NONE',  ( -0.000000000000000000, -1.000000000000000000, -0.000000000000000000 ) ) ;
#116746 = EDGE_CURVE ( 'NONE', #95423, #62529, #63632, .T. ) ;
#116747 = AXIS2_PLACEMENT_3D ( 'NONE', #2027, #121803, #42630 ) ;
#116748 = CIRCLE ( 'NONE', #45755, 0.1000000000000000472 ) ;
#116749 = CARTESIAN_POINT ( 'NONE',  ( 7.314170287673361415, -2.499999999999618083, 9.688393442490539798 ) ) ;
#116751 = DIRECTION ( 'NONE',  ( -0.000000000000000000, 1.000000000000000000, -0.000000000000000000 ) ) ;
#116750 = CIRCLE ( 'NONE', #22689, 0.1000000000000000472 ) ;
#116752 = DIRECTION ( 'NONE',  ( 0.000000000000000000, 0.000000000000000000, 1.000000000000000000 ) ) ;
#116753 = CARTESIAN_POINT ( 'NONE',  ( 187.1145833340161175, 6.668395609140177704, -3.849999999999998312 ) ) ;
#116754 = EDGE_CURVE ( 'NONE', #79916, #71153, #23921, .T. ) ;
#116755 = ADVANCED_FACE ( 'NONE', ( #74464 ), #92879, .T. ) ;
#116756 = VERTEX_POINT ( 'NONE', #123545 ) ;
#116757 = AXIS2_PLACEMENT_3D ( 'NONE', #10513, #41294, #100824 ) ;
#116758 = ORIENTED_EDGE ( 'NONE', *, *, #31680, .F. ) ;
#116759 = AXIS2_PLACEMENT_3D ( 'NONE', #57380, #29855, #97304 ) ;
#116760 = ORIENTED_EDGE ( 'NONE', *, *, #96978, .F. ) ;
#116761 = ORIENTED_EDGE ( 'NONE', *, *, #117499, .T. ) ;
#116762 = ADVANCED_FACE ( 'NONE', ( #124208 ), #9246, .T. ) ;
#116763 = AXIS2_PLACEMENT_3D ( 'NONE', #11293, #42725, #10627 ) ;
#116764 = DIRECTION ( 'NONE',  ( -0.000000000000000000, 1.000000000000000000, -0.000000000000000000 ) ) ;
#116765 = ORIENTED_EDGE ( 'NONE', *, *, #122846, .T. ) ;
#116766 = EDGE_CURVE ( 'NONE', #24092, #33748, #32254, .T. ) ;
#116767 = EDGE_LOOP ( 'NONE', ( #110948, #115495 ) ) ;
#116768 = AXIS2_PLACEMENT_3D ( 'NONE', #108324, #67082, #19290 ) ;
#116769 = CARTESIAN_POINT ( 'NONE',  ( 2.499999999999948930, 12.50000000000000000, -0.6277270498435166823 ) ) ;
#116770 = AXIS2_PLACEMENT_3D ( 'NONE', #37298, #30057, #119072 ) ;
#116771 = DIRECTION ( 'NONE',  ( 0.000000000000000000, 0.000000000000000000, -1.000000000000000000 ) ) ;
#116772 = DIRECTION ( 'NONE',  ( 0.000000000000000000, 0.000000000000000000, -1.000000000000000000 ) ) ;
#116773 = CARTESIAN_POINT ( 'NONE',  ( 11.69999999999990514, 2.500000000000000000, -0.1000000000000022815 ) ) ;
#116774 = CARTESIAN_POINT ( 'NONE',  ( 9.799999999999915445, 12.50000000000000000, -4.676537180435977881 ) ) ;
#116775 = ORIENTED_EDGE ( 'NONE', *, *, #18192, .F. ) ;
#116776 = DIRECTION ( 'NONE',  ( 0.000000000000000000, 0.000000000000000000, -1.000000000000000000 ) ) ;
#116777 = ORIENTED_EDGE ( 'NONE', *, *, #30090, .T. ) ;
#116778 = FACE_OUTER_BOUND ( 'NONE', #110954, .T. ) ;
#116779 = ORIENTED_EDGE ( 'NONE', *, *, #18743, .T. ) ;
#116780 = DIRECTION ( 'NONE',  ( 0.000000000000000000, 0.000000000000000000, -1.000000000000000000 ) ) ;
#116781 = PLANE ( 'NONE',  #38607 ) ;
#116782 = VECTOR ( 'NONE', #49225, 1000.000000000000000 ) ;
#116783 = EDGE_LOOP ( 'NONE', ( #68436, #21166 ) ) ;
#116784 = DIRECTION ( 'NONE',  ( 0.000000000000000000, 0.000000000000000000, 1.000000000000000000 ) ) ;
#116785 = LINE ( 'NONE', #36328, #118810 ) ;
#116786 = ORIENTED_EDGE ( 'NONE', *, *, #54256, .T. ) ;
#116787 = EDGE_CURVE ( 'NONE', #24257, #24371, #57362, .T. ) ;
#116788 = CIRCLE ( 'NONE', #18600, 0.06509327318403745899 ) ;
#116789 = CARTESIAN_POINT ( 'NONE',  ( -1.050000000000038236, 2.500000000000000000, -6.148780366869526226 ) ) ;
#116790 = VERTEX_POINT ( 'NONE', #17453 ) ;
#116791 = ORIENTED_EDGE ( 'NONE', *, *, #58420, .F. ) ;
#116792 = CARTESIAN_POINT ( 'NONE',  ( 3.149999999999946176, 2.500000000000000000, -6.148780366869526226 ) ) ;
#116793 = CARTESIAN_POINT ( 'NONE',  ( 127.5000000000000000, 5.000000000000000000, -4.999999999999998224 ) ) ;
#116794 = CARTESIAN_POINT ( 'NONE',  ( 185.4218750003414016, 0.000000000000000000, 7.564683531250000925 ) ) ;
#116797 = AXIS2_PLACEMENT_3D ( 'NONE', #23197, #33052, #990 ) ;
#116796 = VECTOR ( 'NONE', #19205, 1000.000000000000000 ) ;
#116795 = CARTESIAN_POINT ( 'NONE',  ( -5.600000000000020073, 12.50000000000000000, 0.2813168883297362810 ) ) ;
#116798 = EDGE_CURVE ( 'NONE', #80857, #40877, #47589, .T. ) ;
#116799 = CIRCLE ( 'NONE', #118867, 0.1000000000000000472 ) ;
#116800 = LINE ( 'NONE', #25858, #29051 ) ;
#116801 = FACE_OUTER_BOUND ( 'NONE', #49234, .T. ) ;
#116802 = EDGE_CURVE ( 'NONE', #55527, #97550, #65268, .T. ) ;
#116803 = AXIS2_PLACEMENT_3D ( 'NONE', #55273, #95194, #63805 ) ;
#116804 = EDGE_CURVE ( 'NONE', #10727, #249, #5067, .T. ) ;
#116805 = EDGE_CURVE ( 'NONE', #112541, #88966, #114375, .T. ) ;
#116806 = ORIENTED_EDGE ( 'NONE', *, *, #33435, .T. ) ;
#116807 = DIRECTION ( 'NONE',  ( -4.274815082592931898E-19, -0.9999939076577903929, -0.003490651415223739937 ) ) ;
#116808 = ORIENTED_EDGE ( 'NONE', *, *, #73358, .F. ) ;
#116811 = EDGE_CURVE ( 'NONE', #13161, #117090, #103339, .T. ) ;
#116810 = CIRCLE ( 'NONE', #62552, 0.1000000000000002554 ) ;
#116809 = CONICAL_SURFACE ( 'NONE', #123088, 0.1000000000000002554, 0.003490658503988666988 ) ;
#116812 = DIRECTION ( 'NONE',  ( -4.274815082592931898E-19, -0.9999939076577903929, -0.003490651415223739937 ) ) ;
#116813 = CARTESIAN_POINT ( 'NONE',  ( 14.39999999999989555, 2.500000000000000000, -0.4464101615137782142 ) ) ;
#116814 = DIRECTION ( 'NONE',  ( -0.000000000000000000, -1.000000000000000000, -0.000000000000000000 ) ) ;
#116815 = LINE ( 'NONE', #127937, #104474 ) ;
#116816 = FACE_OUTER_BOUND ( 'NONE', #22465, .T. ) ;
#116817 = ORIENTED_EDGE ( 'NONE', *, *, #84555, .F. ) ;
#116818 = EDGE_CURVE ( 'NONE', #23967, #86001, #54806, .T. ) ;
#116820 = EDGE_CURVE ( 'NONE', #84308, #56285, #46906, .T. ) ;
#116819 = CONICAL_SURFACE ( 'NONE', #106363, 0.1000000000000000472, 0.003490658503988666988 ) ;
#116821 = FACE_OUTER_BOUND ( 'NONE', #4199, .T. ) ;
#116822 = FACE_OUTER_BOUND ( 'NONE', #113941, .T. ) ;
#116823 = VERTEX_POINT ( 'NONE', #126790 ) ;
#116824 = DIRECTION ( 'NONE',  ( 0.000000000000000000, 0.000000000000000000, 1.000000000000000000 ) ) ;
#116825 = VERTEX_POINT ( 'NONE', #7639 ) ;
#116826 = VERTEX_POINT ( 'NONE', #45659 ) ;
#116827 = DIRECTION ( 'NONE',  ( 0.000000000000000000, 1.000000000000000000, 0.000000000000000000 ) ) ;
#116828 = AXIS2_PLACEMENT_3D ( 'NONE', #61851, #82785, #43504 ) ;
#116829 = ORIENTED_EDGE ( 'NONE', *, *, #76359, .T. ) ;
#116830 = CARTESIAN_POINT ( 'NONE',  ( -6.250000000000019540, 2.500000000000000000, -7.188010851410854052 ) ) ;
#116831 = LINE ( 'NONE', #17992, #98714 ) ;
#116832 = CARTESIAN_POINT ( 'NONE',  ( 7.499999999999925393, 2.500000000000000000, -0.6928203230275541413 ) ) ;
#116833 = VERTEX_POINT ( 'NONE', #15525 ) ;
#116834 = FACE_BOUND ( 'NONE', #45396, .T. ) ;
#116835 = CIRCLE ( 'NONE', #31191, 0.1000000000000000472 ) ;
#116837 = ORIENTED_EDGE ( 'NONE', *, *, #89471, .F. ) ;
#116836 = LINE ( 'NONE', #54683, #43215 ) ;
#116838 = FACE_OUTER_BOUND ( 'NONE', #45422, .T. ) ;
#116839 = CARTESIAN_POINT ( 'NONE',  ( 1.899999999999949507, 12.50000000000000000, 4.676537180435972552 ) ) ;
#116840 = VECTOR ( 'NONE', #108279, 1000.000000000000000 ) ;
#116841 = ORIENTED_EDGE ( 'NONE', *, *, #52772, .F. ) ;
#116842 = AXIS2_PLACEMENT_3D ( 'NONE', #41146, #90866, #81687 ) ;
#116843 = AXIS2_PLACEMENT_3D ( 'NONE', #26939, #125142, #76685 ) ;
#116845 = ORIENTED_EDGE ( 'NONE', *, *, #6534, .F. ) ;
#116844 = EDGE_CURVE ( 'NONE', #52645, #108881, #74088, .T. ) ;
#116846 = ORIENTED_EDGE ( 'NONE', *, *, #96226, .T. ) ;
#116847 = CARTESIAN_POINT ( 'NONE',  ( 4.799999999999937650, 2.500000000000000000, -0.4464101615137782142 ) ) ;
#116848 = DIRECTION ( 'NONE',  ( 0.000000000000000000, 0.000000000000000000, 1.000000000000000000 ) ) ;
#116849 = CARTESIAN_POINT ( 'NONE',  ( -3.749999999999991562, 2.500000000000000000, 6.395190528383296602 ) ) ;
#116850 = FACE_BOUND ( 'NONE', #68403, .T. ) ;
#116851 = EDGE_LOOP ( 'NONE', ( #121185, #75690 ) ) ;
#116852 = AXIS2_PLACEMENT_3D ( 'NONE', #117986, #27661, #87231 ) ;
#116853 = FACE_BOUND ( 'NONE', #99787, .T. ) ;
#116854 = DIRECTION ( 'NONE',  ( -0.000000000000000000, -1.000000000000000000, -0.000000000000000000 ) ) ;
#116855 = ADVANCED_FACE ( 'NONE', ( #116944 ), #34399, .T. ) ;
#116856 = CIRCLE ( 'NONE', #18582, 0.06509327318403745899 ) ;
#116857 = CARTESIAN_POINT ( 'NONE',  ( 184.7500000000000000, 9.429780353434619030E-16, -7.700000000000000178 ) ) ;
#116858 = FACE_OUTER_BOUND ( 'NONE', #65561, .T. ) ;
#116859 = DIRECTION ( 'NONE',  ( 0.000000000000000000, -0.9999939076577903929, 0.003490651415223739937 ) ) ;
#116860 = CARTESIAN_POINT ( 'NONE',  ( 2.699999999999945555, 2.500000000000000000, 3.883716857408420431 ) ) ;
#116861 = CARTESIAN_POINT ( 'NONE',  ( -5.800000000000022027, 2.500000000000000000, -4.230127018922201998 ) ) ;
#116862 = ORIENTED_EDGE ( 'NONE', *, *, #42754, .T. ) ;
#116863 = ORIENTED_EDGE ( 'NONE', *, *, #8599, .T. ) ;
#116864 = ORIENTED_EDGE ( 'NONE', *, *, #17479, .T. ) ;
#116865 = ORIENTED_EDGE ( 'NONE', *, *, #107150, .F. ) ;
#116866 = ORIENTED_EDGE ( 'NONE', *, *, #62877, .T. ) ;
#116867 = CONICAL_SURFACE ( 'NONE', #91853, 0.09999999999999982514, 0.003490658503988666988 ) ;
#116868 = DIRECTION ( 'NONE',  ( 0.000000000000000000, 0.000000000000000000, 1.000000000000000000 ) ) ;
#116869 = CARTESIAN_POINT ( 'NONE',  ( 8.549999999999920774, 12.50000000000000000, 6.148780366869520897 ) ) ;
#116870 = EDGE_LOOP ( 'NONE', ( #109971, #43019 ) ) ;
#116871 = FACE_BOUND ( 'NONE', #85808, .T. ) ;
#116872 = CARTESIAN_POINT ( 'NONE',  ( 7.099999999999928590, 2.500000000000000000, 4.430127018922196847 ) ) ;
#116873 = CARTESIAN_POINT ( 'NONE',  ( 12.04999999999990479, 12.50000000000000000, -6.495190528383302464 ) ) ;
#116874 = FACE_OUTER_BOUND ( 'NONE', #125627, .T. ) ;
#116875 = PLANE ( 'NONE',  #103380 ) ;
#116876 = FACE_OUTER_BOUND ( 'NONE', #49991, .T. ) ;
#116877 = EDGE_LOOP ( 'NONE', ( #13603, #94982, #65322, #71862 ) ) ;
#116878 = CONICAL_SURFACE ( 'NONE', #20757, 0.09999999999999982514, 0.003490658503988666988 ) ;
#116879 = DIRECTION ( 'NONE',  ( 0.000000000000000000, 1.000000000000000000, 0.000000000000000000 ) ) ;
#116881 = ORIENTED_EDGE ( 'NONE', *, *, #80383, .F. ) ;
#116880 = CONICAL_SURFACE ( 'NONE', #60493, 0.09999999999999982514, 0.003490658503988666988 ) ;
#116882 = EDGE_LOOP ( 'NONE', ( #3396, #23972 ) ) ;
#116883 = ORIENTED_EDGE ( 'NONE', *, *, #60199, .T. ) ;
#116884 = CARTESIAN_POINT ( 'NONE',  ( 9.349999999999919709, 12.50000000000000000, -6.906693963081115939 ) ) ;
#116885 = CARTESIAN_POINT ( 'NONE',  ( 14.18215599311778696, 2.499999999999998224, 6.639800458426438290 ) ) ;
#116886 = DIRECTION ( 'NONE',  ( -0.000000000000000000, -1.000000000000000000, -0.000000000000000000 ) ) ;
#116887 = AXIS2_PLACEMENT_3D ( 'NONE', #127868, #97766, #125923 ) ;
#116888 = EDGE_LOOP ( 'NONE', ( #30553, #68345 ) ) ;
#116889 = CARTESIAN_POINT ( 'NONE',  ( 7.173569985890439149, 2.499999999999999556, -8.713264184206867213 ) ) ;
#116890 = EDGE_CURVE ( 'NONE', #64922, #65156, #75738, .T. ) ;
#116891 = DIRECTION ( 'NONE',  ( 0.000000000000000000, 0.000000000000000000, -1.000000000000000000 ) ) ;
#116894 = AXIS2_PLACEMENT_3D ( 'NONE', #43639, #92725, #62632 ) ;
#116893 = DIRECTION ( 'NONE',  ( 0.000000000000000000, 0.000000000000000000, 1.000000000000000000 ) ) ;
#116892 = AXIS2_PLACEMENT_3D ( 'NONE', #1705, #101213, #100555 ) ;
#116895 = CARTESIAN_POINT ( 'NONE',  ( 184.1979166673494603, 6.668395609140176816, 3.850000000000000977 ) ) ;
#116896 = DIRECTION ( 'NONE',  ( -0.000000000000000000, 1.000000000000000000, -0.000000000000000000 ) ) ;
#116897 = DIRECTION ( 'NONE',  ( 0.000000000000000000, 0.000000000000000000, 1.000000000000000000 ) ) ;
#116898 = AXIS2_PLACEMENT_3D ( 'NONE', #94506, #42206, #122691 ) ;
#116899 = EDGE_CURVE ( 'NONE', #89926, #119243, #107127, .T. ) ;
#116900 = LINE ( 'NONE', #16757, #3520 ) ;
#116901 = EDGE_CURVE ( 'NONE', #1265, #79987, #115660, .T. ) ;
#116902 = EDGE_LOOP ( 'NONE', ( #21219, #30195 ) ) ;
#116903 = DIRECTION ( 'NONE',  ( 0.000000000000000000, 0.000000000000000000, -1.000000000000000000 ) ) ;
#116905 = AXIS2_PLACEMENT_3D ( 'NONE', #122804, #23296, #44228 ) ;
#116904 = CIRCLE ( 'NONE', #75066, 0.09999999999999982514 ) ;
#116906 = ORIENTED_EDGE ( 'NONE', *, *, #108916, .F. ) ;
#116907 = ORIENTED_EDGE ( 'NONE', *, *, #52680, .T. ) ;
#116908 = DIRECTION ( 'NONE',  ( 0.000000000000000000, 0.000000000000000000, -1.000000000000000000 ) ) ;
#116909 = EDGE_CURVE ( 'NONE', #112155, #43428, #26016, .T. ) ;
#116910 = EDGE_CURVE ( 'NONE', #42980, #11927, #90806, .T. ) ;
#116911 = CARTESIAN_POINT ( 'NONE',  ( 179.5000000000000000, 0.6250000000000000000, 7.634788798650556707 ) ) ;
#116912 = CARTESIAN_POINT ( 'NONE',  ( -7.500000000000015099, 2.500000000000000000, -5.022947341949754119 ) ) ;
#116913 = ADVANCED_FACE ( 'NONE', ( #105857 ), #35198, .T. ) ;
#116914 = EDGE_LOOP ( 'NONE', ( #96945, #116337 ) ) ;
#116915 = ORIENTED_EDGE ( 'NONE', *, *, #55205, .F. ) ;
#116916 = DIRECTION ( 'NONE',  ( -0.000000000000000000, 1.000000000000000000, -0.000000000000000000 ) ) ;
#116917 = CARTESIAN_POINT ( 'NONE',  ( 10.79999999999991012, 2.500000000000000000, -4.430127018922202176 ) ) ;
#116918 = DIRECTION ( 'NONE',  ( 0.000000000000000000, 0.000000000000000000, 1.000000000000000000 ) ) ;
#116919 = VERTEX_POINT ( 'NONE', #25343 ) ;
#116920 = ORIENTED_EDGE ( 'NONE', *, *, #13337, .T. ) ;
#116921 = DIRECTION ( 'NONE',  ( 0.000000000000000000, 0.000000000000000000, 1.000000000000000000 ) ) ;
#116922 = EDGE_LOOP ( 'NONE', ( #64355, #48613 ) ) ;
#116923 = CARTESIAN_POINT ( 'NONE',  ( 13.54999999999989946, 2.500000000000000000, 2.611473670974873151 ) ) ;
#116925 = DIRECTION ( 'NONE',  ( -0.000000000000000000, -1.000000000000000000, -0.000000000000000000 ) ) ;
#116924 = CIRCLE ( 'NONE', #129585, 0.06509327318403745899 ) ;
#116926 = VERTEX_POINT ( 'NONE', #46953 ) ;
#116927 = DIRECTION ( 'NONE',  ( -0.000000000000000000, -1.000000000000000000, -0.000000000000000000 ) ) ;
#116928 = CARTESIAN_POINT ( 'NONE',  ( -13.54999999999998828, 12.50000000000000000, 1.818653347947325472 ) ) ;
#116929 = FACE_OUTER_BOUND ( 'NONE', #127120, .T. ) ;
#116930 = CARTESIAN_POINT ( 'NONE',  ( -11.64999999999999680, 12.50000000000000000, -6.495190528383298911 ) ) ;
#116931 = CONICAL_SURFACE ( 'NONE', #85553, 0.1000000000000002554, 0.003490658503988666988 ) ;
#116932 = ORIENTED_EDGE ( 'NONE', *, *, #80606, .T. ) ;
#116933 = AXIS2_PLACEMENT_3D ( 'NONE', #121449, #91352, #29232 ) ;
#116935 = CARTESIAN_POINT ( 'NONE',  ( -11.89999999999999680, 12.50000000000000000, -4.611443907251937979 ) ) ;
#116934 = AXIS2_PLACEMENT_3D ( 'NONE', #62840, #13721, #31456 ) ;
#116936 = FACE_OUTER_BOUND ( 'NONE', #67089, .T. ) ;
#116937 = ORIENTED_EDGE ( 'NONE', *, *, #109597, .F. ) ;
#116938 = EDGE_LOOP ( 'NONE', ( #110811, #107619, #4477, #12956 ) ) ;
#116939 = CARTESIAN_POINT ( 'NONE',  ( 184.6302083336747444, -4.367472073101514418, -7.564683531250002702 ) ) ;
#116940 = CARTESIAN_POINT ( 'NONE',  ( -3.350000000000028511, 2.500000000000000000, 2.857883832488649301 ) ) ;
#116941 = CARTESIAN_POINT ( 'NONE',  ( -14.54999999999998472, 2.500000000000000000, -2.265063509461099578 ) ) ;
#116942 = DIRECTION ( 'NONE',  ( 0.000000000000000000, 1.000000000000000000, 0.000000000000000000 ) ) ;
#116943 = CONICAL_SURFACE ( 'NONE', #6214, 0.1000000000000002554, 0.003490658503988666988 ) ;
#116944 = FACE_OUTER_BOUND ( 'NONE', #98, .T. ) ;
#116945 = DIRECTION ( 'NONE',  ( 0.000000000000000000, 0.000000000000000000, 1.000000000000000000 ) ) ;
#116946 = CONICAL_SURFACE ( 'NONE', #37557, 0.09999999999999982514, 0.003490658503988666988 ) ;
#116947 = CIRCLE ( 'NONE', #20828, 0.06509327318403745899 ) ;
#116948 = LINE ( 'NONE', #16160, #25880 ) ;
#116949 = DIRECTION ( 'NONE',  ( -0.000000000000000000, 1.000000000000000000, -0.000000000000000000 ) ) ;
#116950 = CARTESIAN_POINT ( 'NONE',  ( 8.349999999999923261, 2.500000000000000000, 1.372243186433545370 ) ) ;
#116951 = EDGE_CURVE ( 'NONE', #81732, #97929, #59544, .T. ) ;
#116952 = ADVANCED_FACE ( 'NONE', ( #26657 ), #6980, .T. ) ;
#116953 = EDGE_CURVE ( 'NONE', #16115, #74932, #124358, .T. ) ;
#116954 = DIRECTION ( 'NONE',  ( -0.000000000000000000, -1.000000000000000000, -0.000000000000000000 ) ) ;
#116955 = EDGE_LOOP ( 'NONE', ( #122565, #36914 ) ) ;
#116956 = ADVANCED_FACE ( 'NONE', ( #117575 ), #36541, .T. ) ;
#116957 = AXIS2_PLACEMENT_3D ( 'NONE', #119987, #30334, #108858 ) ;
#116958 = FACE_OUTER_BOUND ( 'NONE', #12120, .T. ) ;
#116959 = EDGE_CURVE ( 'NONE', #81870, #21966, #61670, .T. ) ;
#116960 = DIRECTION ( 'NONE',  ( 0.000000000000000000, 0.000000000000000000, -1.000000000000000000 ) ) ;
#116961 = DIRECTION ( 'NONE',  ( 0.000000000000000000, 0.000000000000000000, -1.000000000000000000 ) ) ;
#116962 = DIRECTION ( 'NONE',  ( 0.000000000000000000, 0.000000000000000000, 1.000000000000000000 ) ) ;
#116963 = VERTEX_POINT ( 'NONE', #109050 ) ;
#116964 = ADVANCED_FACE ( 'NONE', ( #99909 ), #99230, .T. ) ;
#116965 = DIRECTION ( 'NONE',  ( 0.000000000000000000, -0.9999939076577903929, 0.003490651415223739937 ) ) ;
#116966 = EDGE_CURVE ( 'NONE', #67328, #48532, #82510, .T. ) ;
#116967 = DIRECTION ( 'NONE',  ( 0.000000000000000000, 0.000000000000000000, -1.000000000000000000 ) ) ;
#116969 = EDGE_LOOP ( 'NONE', ( #74810, #102159, #83889, #104499 ) ) ;
#116968 = FACE_OUTER_BOUND ( 'NONE', #10230, .T. ) ;
#116970 = EDGE_CURVE ( 'NONE', #92073, #3679, #50808, .T. ) ;
#116971 = ORIENTED_EDGE ( 'NONE', *, *, #110713, .T. ) ;
#116972 = EDGE_LOOP ( 'NONE', ( #82232, #103194 ) ) ;
#116973 = ORIENTED_EDGE ( 'NONE', *, *, #29898, .T. ) ;
#116974 = ORIENTED_EDGE ( 'NONE', *, *, #3858, .F. ) ;
#116975 = PLANE ( 'NONE',  #98846 ) ;
#116976 = AXIS2_PLACEMENT_3D ( 'NONE', #25469, #65401, #105340 ) ;
#116977 = PLANE ( 'NONE',  #128043 ) ;
#116978 = LINE ( 'NONE', #60036, #77605 ) ;
#116979 = CARTESIAN_POINT ( 'NONE',  ( 4.399999999999940847, 12.50000000000000000, -3.983716857408426293 ) ) ;
#116980 = ORIENTED_EDGE ( 'NONE', *, *, #61409, .T. ) ;
#116982 = AXIS2_PLACEMENT_3D ( 'NONE', #37675, #107697, #85473 ) ;
#116981 = VECTOR ( 'NONE', #72404, 1000.000000000000000 ) ;
#116983 = PLANE ( 'NONE',  #87958 ) ;
#116984 = EDGE_LOOP ( 'NONE', ( #57583, #26502, #23764, #79062 ) ) ;
#116985 = CARTESIAN_POINT ( 'NONE',  ( 65.40763333645755040, -3.109051995142349867, -5.794606894451852064 ) ) ;
#116986 = CARTESIAN_POINT ( 'NONE',  ( 13.80955901302179534, -2.500000000000000000, -7.955427456727499624 ) ) ;
#116987 = CARTESIAN_POINT ( 'NONE',  ( 6.249999999999934275, 2.500000000000000000, -7.288010851410854585 ) ) ;
#116988 = FACE_OUTER_BOUND ( 'NONE', #114088, .T. ) ;
#116989 = ORIENTED_EDGE ( 'NONE', *, *, #115744, .F. ) ;
#116991 = AXIS2_PLACEMENT_3D ( 'NONE', #114900, #107004, #127323 ) ;
#116990 = CONICAL_SURFACE ( 'NONE', #100293, 0.09999999999999982514, 0.003490658503988666988 ) ;
#116992 = ORIENTED_EDGE ( 'NONE', *, *, #112839, .T. ) ;
#116993 = ORIENTED_EDGE ( 'NONE', *, *, #4191, .F. ) ;
#116994 = ORIENTED_EDGE ( 'NONE', *, *, #73186, .T. ) ;
#116995 = CARTESIAN_POINT ( 'NONE',  ( -11.44999999999999929, 12.50000000000000000, -6.148780366869522673 ) ) ;
#116996 = CARTESIAN_POINT ( 'NONE',  ( -7.300000000000018474, 2.500000000000000000, -4.083716857408426826 ) ) ;
#116997 = PLANE ( 'NONE',  #25285 ) ;
#116998 = FACE_BOUND ( 'NONE', #52326, .T. ) ;
#116999 = DIRECTION ( 'NONE',  ( 0.000000000000000000, 0.000000000000000000, -1.000000000000000000 ) ) ;
#117000 = DIRECTION ( 'NONE',  ( 0.000000000000000000, 1.000000000000000000, 0.000000000000000000 ) ) ;
#117001 = CARTESIAN_POINT ( 'NONE',  ( -7.300000000000013145, 12.50000000000000000, 3.918623584224382839 ) ) ;
#117002 = DIRECTION ( 'NONE',  ( -0.000000000000000000, 1.000000000000000000, -0.000000000000000000 ) ) ;
#117003 = EDGE_CURVE ( 'NONE', #13612, #51768, #21970, .T. ) ;
#117004 = CARTESIAN_POINT ( 'NONE',  ( 186.2552083336747444, 6.551208109652275624, -3.782341765624998686 ) ) ;
#117005 = DIRECTION ( 'NONE',  ( 0.000000000000000000, 1.000000000000000000, 0.000000000000000000 ) ) ;
#117006 = CARTESIAN_POINT ( 'NONE',  ( -4.550000000000022915, 12.50000000000000000, 2.165063509461097713 ) ) ;
#117007 = AXIS2_PLACEMENT_3D ( 'NONE', #62438, #13307, #114101 ) ;
#117008 = CIRCLE ( 'NONE', #94053, 0.1000000000000002554 ) ;
#117009 = CARTESIAN_POINT ( 'NONE',  ( 0.8499999999999545697, 2.500000000000000000, -1.472243186433550122 ) ) ;
#117010 = VERTEX_POINT ( 'NONE', #107789 ) ;
#117011 = ORIENTED_EDGE ( 'NONE', *, *, #83984, .F. ) ;
#117012 = ORIENTED_EDGE ( 'NONE', *, *, #24178, .T. ) ;
#117013 = ORIENTED_EDGE ( 'NONE', *, *, #17448, .F. ) ;
#117014 = DIRECTION ( 'NONE',  ( -0.000000000000000000, 1.000000000000000000, -0.000000000000000000 ) ) ;
#117015 = FACE_BOUND ( 'NONE', #105162, .T. ) ;
#117016 = DIRECTION ( 'NONE',  ( 0.000000000000000000, 0.000000000000000000, 1.000000000000000000 ) ) ;
#117017 = AXIS2_PLACEMENT_3D ( 'NONE', #46569, #5993, #47240 ) ;
#117018 = CARTESIAN_POINT ( 'NONE',  ( -5.850000000000018296, 12.50000000000000000, 7.188010851410848723 ) ) ;
#117019 = EDGE_LOOP ( 'NONE', ( #96155, #80963 ) ) ;
#117020 = CARTESIAN_POINT ( 'NONE',  ( -7.499999999999980460, 2.500000000000000000, -0.1000000000000022815 ) ) ;
#117021 = CARTESIAN_POINT ( 'NONE',  ( -7.900000000000014566, 2.500000000000000000, -3.737306695894649700 ) ) ;
#117022 = DIRECTION ( 'NONE',  ( -0.000000000000000000, 1.000000000000000000, -0.000000000000000000 ) ) ;
#117023 = VECTOR ( 'NONE', #79065, 1000.000000000000000 ) ;
#117024 = VERTEX_POINT ( 'NONE', #68500 ) ;
#117025 = CARTESIAN_POINT ( 'NONE',  ( 10.64999999999990976, 12.50000000000000000, -6.213873640053564351 ) ) ;
#117026 = DIRECTION ( 'NONE',  ( 0.000000000000000000, 1.000000000000000000, 0.000000000000000000 ) ) ;
#117027 = CIRCLE ( 'NONE', #121262, 0.1000000000000002554 ) ;
#117028 = CONICAL_SURFACE ( 'NONE', #39728, 0.1000000000000000472, 0.003490658503988666988 ) ;
#117029 = ORIENTED_EDGE ( 'NONE', *, *, #2770, .T. ) ;
#117030 = CARTESIAN_POINT ( 'NONE',  ( 8.549999999999918998, 2.500000000000000000, -1.818653347947326138 ) ) ;
#117032 = CIRCLE ( 'NONE', #20917, 0.06509327318403745899 ) ;
#117031 = CARTESIAN_POINT ( 'NONE',  ( -6.450000000000017941, 2.500000000000000000, -6.941600689897077459 ) ) ;
#117033 = AXIS2_PLACEMENT_3D ( 'NONE', #113296, #32828, #102820 ) ;
#117034 = ORIENTED_EDGE ( 'NONE', *, *, #31751, .T. ) ;
#117035 = ADVANCED_FACE ( 'NONE', ( #59356 ), #40752, .T. ) ;
#117036 = DIRECTION ( 'NONE',  ( 0.000000000000000000, 0.000000000000000000, 1.000000000000000000 ) ) ;
#117037 = CARTESIAN_POINT ( 'NONE',  ( 11.84999999999990727, 2.500000000000000000, 6.841600689897072485 ) ) ;
#117038 = EDGE_LOOP ( 'NONE', ( #18912, #22417, #540, #93854 ) ) ;
#117039 = CARTESIAN_POINT ( 'NONE',  ( 9.999999999999911182, 2.500000000000000000, -3.637306695894650055 ) ) ;
#117040 = AXIS2_PLACEMENT_3D ( 'NONE', #104151, #14457, #54397 ) ;
#117041 = ORIENTED_EDGE ( 'NONE', *, *, #91159, .T. ) ;
#117042 = ORIENTED_EDGE ( 'NONE', *, *, #2929, .T. ) ;
#117043 = EDGE_CURVE ( 'NONE', #123305, #87698, #80270, .T. ) ;
#117044 = DIRECTION ( 'NONE',  ( 0.000000000000000000, 0.000000000000000000, 1.000000000000000000 ) ) ;
#117045 = EDGE_CURVE ( 'NONE', #6029, #63031, #109693, .T. ) ;
#117046 = ORIENTED_EDGE ( 'NONE', *, *, #24281, .T. ) ;
#117047 = DIRECTION ( 'NONE',  ( -0.000000000000000000, -1.000000000000000000, -0.000000000000000000 ) ) ;
#117048 = FACE_BOUND ( 'NONE', #96898, .T. ) ;
#117049 = ORIENTED_EDGE ( 'NONE', *, *, #100405, .T. ) ;
#117050 = CARTESIAN_POINT ( 'NONE',  ( 12.09999999999990195, 2.500000000000000000, -0.6928203230275541413 ) ) ;
#117051 = VERTEX_POINT ( 'NONE', #10237 ) ;
#117052 = DIRECTION ( 'NONE',  ( 0.000000000000000000, 0.000000000000000000, -1.000000000000000000 ) ) ;
#117053 = CARTESIAN_POINT ( 'NONE',  ( -4.150000000000027889, 12.50000000000000000, -6.560283801567339701 ) ) ;
#117054 = EDGE_CURVE ( 'NONE', #92955, #120893, #70445, .T. ) ;
#117055 = EDGE_CURVE ( 'NONE', #64042, #75618, #122211, .T. ) ;
#117056 =( BOUNDED_CURVE ( )  B_SPLINE_CURVE ( 2, ( #27480, #37967, #17673 ),
 .UNSPECIFIED., .F., .F. ) 
 B_SPLINE_CURVE_WITH_KNOTS ( ( 3, 3 ),
 ( 0.0008083180696985040568, 0.0008883710667521964310 ),
 .UNSPECIFIED. ) 
 CURVE ( )  GEOMETRIC_REPRESENTATION_ITEM ( )  RATIONAL_B_SPLINE_CURVE ( ( 0.9944676636817101345, 0.9972072019273799937, 1.000000000000000000 ) ) 
 REPRESENTATION_ITEM ( '' )  );
#117057 = DIRECTION ( 'NONE',  ( 0.000000000000000000, -0.9999939076577903929, 0.003490651415223739937 ) ) ;
#117058 = EDGE_CURVE ( 'NONE', #91328, #58594, #42818, .T. ) ;
#117059 = DIRECTION ( 'NONE',  ( 0.000000000000000000, 1.000000000000000000, 0.000000000000000000 ) ) ;
#117060 = ADVANCED_FACE ( 'NONE', ( #90726 ), #84644, .T. ) ;
#117061 = ADVANCED_FACE ( 'NONE', ( #60004 ), #51205, .T. ) ;
#117062 = DIRECTION ( 'NONE',  ( -0.000000000000000000, -1.000000000000000000, -0.000000000000000000 ) ) ;
#117063 = EDGE_LOOP ( 'NONE', ( #26196, #82800 ) ) ;
#117064 = ORIENTED_EDGE ( 'NONE', *, *, #127728, .F. ) ;
#117065 = DIRECTION ( 'NONE',  ( -0.000000000000000000, 1.000000000000000000, -0.000000000000000000 ) ) ;
#117066 = CARTESIAN_POINT ( 'NONE',  ( 17.37282530749025966, -0.4689596142739139717, 5.357821376857582862 ) ) ;
#117068 = LINE ( 'NONE', #96152, #112895 ) ;
#117067 = AXIS2_PLACEMENT_3D ( 'NONE', #121439, #82830, #51442 ) ;
#117070 = VERTEX_POINT ( 'NONE', #48886 ) ;
#117069 = ORIENTED_EDGE ( 'NONE', *, *, #74399, .T. ) ;
#117071 = EDGE_LOOP ( 'NONE', ( #43346, #7751, #32648, #78399, #127358, #123350, #58593, #75597, #112912, #100386, #40983, #44841 ) ) ;
#117072 = EDGE_CURVE ( 'NONE', #56826, #85037, #98589, .T. ) ;
#117073 = CARTESIAN_POINT ( 'NONE',  ( 8.949999999999917577, 2.500000000000000000, -2.511473670974877948 ) ) ;
#117074 = CARTESIAN_POINT ( 'NONE',  ( -8.300000000000011369, 12.50000000000000000, -4.395220292106239768 ) ) ;
#117075 = EDGE_CURVE ( 'NONE', #104178, #67710, #95024, .T. ) ;
#117076 = CARTESIAN_POINT ( 'NONE',  ( 7.899999999999924860, 12.50000000000000000, -4.957854068765716882 ) ) ;
#117077 = SHAPE_DEFINITION_REPRESENTATION ( #92096, #120523 ) ;
#117079 = AXIS2_PLACEMENT_3D ( 'NONE', #53298, #44100, #4804 ) ;
#117078 = CONICAL_SURFACE ( 'NONE', #106, 0.1000000000000000472, 0.003490658503988666988 ) ;
#117080 = LINE ( 'NONE', #86990, #108006 ) ;
#117081 = FACE_OUTER_BOUND ( 'NONE', #13018, .T. ) ;
#117082 = CARTESIAN_POINT ( 'NONE',  ( -6.650000000000018119, 2.500000000000000000, -2.957883832488653830 ) ) ;
#117083 = FACE_OUTER_BOUND ( 'NONE', #48134, .T. ) ;
#117084 = CARTESIAN_POINT ( 'NONE',  ( -11.25000000000000000, 2.500000000000000000, 7.188010851410848723 ) ) ;
#117085 = LINE ( 'NONE', #56243, #6033 ) ;
#117086 = VERTEX_POINT ( 'NONE', #58691 ) ;
#117087 = AXIS2_PLACEMENT_3D ( 'NONE', #72868, #112798, #23117 ) ;
#117088 = ORIENTED_EDGE ( 'NONE', *, *, #27418, .T. ) ;
#117089 = CARTESIAN_POINT ( 'NONE',  ( 11.69999999999990870, 12.50000000000000000, 4.330127018922196314 ) ) ;
#117090 = VERTEX_POINT ( 'NONE', #8924 ) ;
#117091 = VERTEX_POINT ( 'NONE', #128747 ) ;
#117092 = FACE_OUTER_BOUND ( 'NONE', #2315, .T. ) ;
#117093 = CARTESIAN_POINT ( 'NONE',  ( 4.549999999999937650, 2.500000000000000000, 2.065063509461097624 ) ) ;
#117094 = CARTESIAN_POINT ( 'NONE',  ( -4.251297162942325111E-14, 2.500000000000000000, -3.737306695894649700 ) ) ;
#117095 = FACE_OUTER_BOUND ( 'NONE', #69548, .T. ) ;
#117096 = DIRECTION ( 'NONE',  ( 0.000000000000000000, 1.000000000000000000, 0.000000000000000000 ) ) ;
#117097 = CARTESIAN_POINT ( 'NONE',  ( -7.300000000000018474, 2.500000000000000000, -4.083716857408426826 ) ) ;
#117098 = DIRECTION ( 'NONE',  ( 0.000000000000000000, 0.000000000000000000, 1.000000000000000000 ) ) ;
#117099 = EDGE_LOOP ( 'NONE', ( #114981, #66223, #105178, #46183 ) ) ;
#117100 = DIRECTION ( 'NONE',  ( 0.000000000000000000, -0.000000000000000000, 1.000000000000000000 ) ) ;
#117101 = EDGE_CURVE ( 'NONE', #15129, #63981, #103776, .T. ) ;
#117102 = ADVANCED_FACE ( 'NONE', ( #91368 ), #53260, .T. ) ;
#117103 = CARTESIAN_POINT ( 'NONE',  ( 9.149999999999916866, 2.500000000000000000, -1.472243186433550122 ) ) ;
#117104 = ORIENTED_EDGE ( 'NONE', *, *, #43823, .F. ) ;
#117105 = EDGE_CURVE ( 'NONE', #94293, #83874, #14078, .T. ) ;
#117106 = VERTEX_POINT ( 'NONE', #63850 ) ;
#117107 = EDGE_LOOP ( 'NONE', ( #105169, #10499, #9695, #108062 ) ) ;
#117108 = EDGE_CURVE ( 'NONE', #37252, #59946, #88757, .T. ) ;
#117109 = ORIENTED_EDGE ( 'NONE', *, *, #17314, .F. ) ;
#117110 = CARTESIAN_POINT ( 'NONE',  ( 1.849999999999950573, 2.500000000000000000, -1.818653347947326138 ) ) ;
#117111 = FACE_OUTER_BOUND ( 'NONE', #18855, .T. ) ;
#117112 = AXIS2_PLACEMENT_3D ( 'NONE', #101395, #121026, #78042 ) ;
#117113 = ADVANCED_FACE ( 'NONE', ( #33118 ), #76242, .T. ) ;
#117114 = EDGE_LOOP ( 'NONE', ( #101929, #67615 ) ) ;
#117115 = CARTESIAN_POINT ( 'NONE',  ( 12.89999999999990266, 2.500000000000000000, 5.022947341949748790 ) ) ;
#117116 = DIRECTION ( 'NONE',  ( -0.000000000000000000, 1.000000000000000000, -0.000000000000000000 ) ) ;
#117117 = ADVANCED_FACE ( 'NONE', ( #31183 ), #61276, .T. ) ;
#117118 = DIRECTION ( 'NONE',  ( -0.000000000000000000, -1.000000000000000000, -0.000000000000000000 ) ) ;
#117119 = ORIENTED_EDGE ( 'NONE', *, *, #25318, .F. ) ;
#117120 = DIRECTION ( 'NONE',  ( 0.000000000000000000, 0.000000000000000000, 1.000000000000000000 ) ) ;
#117121 = EDGE_CURVE ( 'NONE', #128031, #29713, #32354, .T. ) ;
#117122 = DIRECTION ( 'NONE',  ( 0.000000000000000000, -0.9999939076577903929, 0.003490651415223739937 ) ) ;
#117123 = CIRCLE ( 'NONE', #125458, 0.06509327318403745899 ) ;
#117124 = EDGE_LOOP ( 'NONE', ( #29312, #2665 ) ) ;
#117125 = CIRCLE ( 'NONE', #115070, 0.06509327318403745899 ) ;
#117126 = ORIENTED_EDGE ( 'NONE', *, *, #10963, .T. ) ;
#117127 = ORIENTED_EDGE ( 'NONE', *, *, #118125, .T. ) ;
#117128 = DIRECTION ( 'NONE',  ( -0.000000000000000000, -1.000000000000000000, -0.000000000000000000 ) ) ;
#117129 = AXIS2_PLACEMENT_3D ( 'NONE', #12370, #122982, #123603 ) ;
#117130 = CARTESIAN_POINT ( 'NONE',  ( -8.350000000000012079, 12.50000000000000000, -1.472243186433550122 ) ) ;
#117131 = AXIS2_PLACEMENT_3D ( 'NONE', #122363, #92231, #90286 ) ;
#117132 = ORIENTED_EDGE ( 'NONE', *, *, #118387, .T. ) ;
#117133 = CARTESIAN_POINT ( 'NONE',  ( 4.799999999999935874, 12.50000000000000000, 0.3464101615137735735 ) ) ;
#117134 = DIRECTION ( 'NONE',  ( 0.000000000000000000, 1.000000000000000000, 0.000000000000000000 ) ) ;
#117135 = CARTESIAN_POINT ( 'NONE',  ( 2.499999999999983569, 2.500000000000000000, -4.330127018922201643 ) ) ;
#117136 = CARTESIAN_POINT ( 'NONE',  ( 6.249999999999968914, 12.50000000000000000, -6.430097255199264339 ) ) ;
#117137 = EDGE_CURVE ( 'NONE', #28419, #47021, #73020, .T. ) ;
#117138 = ORIENTED_EDGE ( 'NONE', *, *, #66515, .F. ) ;
#117139 = DIRECTION ( 'NONE',  ( 0.000000000000000000, 0.000000000000000000, 1.000000000000000000 ) ) ;
#117140 = ORIENTED_EDGE ( 'NONE', *, *, #86344, .F. ) ;
#117141 = ORIENTED_EDGE ( 'NONE', *, *, #37332, .T. ) ;
#117142 = FACE_OUTER_BOUND ( 'NONE', #19849, .T. ) ;
#117143 = VERTEX_POINT ( 'NONE', #11519 ) ;
#117144 = CARTESIAN_POINT ( 'NONE',  ( -10.85000000000000142, 12.50000000000000000, -2.857883832488649745 ) ) ;
#117145 = FACE_BOUND ( 'NONE', #111597, .T. ) ;
#117146 = CARTESIAN_POINT ( 'NONE',  ( 8.349999999999919709, 2.500000000000000000, 5.902370205355745192 ) ) ;
#117147 = DIRECTION ( 'NONE',  ( 0.000000000000000000, 1.000000000000000000, 0.000000000000000000 ) ) ;
#117148 = CARTESIAN_POINT ( 'NONE',  ( 9.549999999999918998, 2.500000000000000000, -6.495190528383302464 ) ) ;
#117149 = EDGE_CURVE ( 'NONE', #95427, #23570, #51463, .T. ) ;
#117150 = AXIS2_PLACEMENT_3D ( 'NONE', #128050, #48862, #79596 ) ;
#117151 = EDGE_LOOP ( 'NONE', ( #120895, #23659 ) ) ;
#117153 = CONICAL_SURFACE ( 'NONE', #52428, 0.1000000000000000472, 0.003490658503988666988 ) ;
#117152 = CARTESIAN_POINT ( 'NONE',  ( 1.049999999999954525, 12.50000000000000000, -2.511473670974877948 ) ) ;
#117154 = CARTESIAN_POINT ( 'NONE',  ( -0.6000000000000383915, 12.50000000000000000, -3.983716857408426293 ) ) ;
#117155 = DIRECTION ( 'NONE',  ( 0.000000000000000000, -0.9999939076577903929, 0.003490651415223739937 ) ) ;
#117156 = CARTESIAN_POINT ( 'NONE',  ( 3.349999999999944578, 2.500000000000000000, -5.802370205355749988 ) ) ;
#117157 = VERTEX_POINT ( 'NONE', #1687 ) ;
#117158 = DIRECTION ( 'NONE',  ( -0.000000000000000000, 1.000000000000000000, -0.000000000000000000 ) ) ;
#117159 = CIRCLE ( 'NONE', #60761, 2.750000000000002665 ) ;
#117160 = CARTESIAN_POINT ( 'NONE',  ( 2.299999999999947864, 2.500000000000000000, 3.983716857408420964 ) ) ;
#117161 = VERTEX_POINT ( 'NONE', #41012 ) ;
#117162 = DIRECTION ( 'NONE',  ( 0.000000000000000000, 0.000000000000000000, 1.000000000000000000 ) ) ;
#117163 = EDGE_CURVE ( 'NONE', #108547, #71302, #74182, .T. ) ;
#117164 = DIRECTION ( 'NONE',  ( 0.000000000000000000, 0.000000000000000000, 1.000000000000000000 ) ) ;
#117165 = FACE_BOUND ( 'NONE', #1440, .T. ) ;
#117166 = DIRECTION ( 'NONE',  ( 0.000000000000000000, 0.000000000000000000, -1.000000000000000000 ) ) ;
#117167 = VERTEX_POINT ( 'NONE', #112307 ) ;
#117168 = CARTESIAN_POINT ( 'NONE',  ( 13.34999999999990017, 2.500000000000000000, 2.857883832488649301 ) ) ;
#117169 = EDGE_LOOP ( 'NONE', ( #31786, #54693 ) ) ;
#117170 = EDGE_LOOP ( 'NONE', ( #8129, #14248, #10633, #115856 ) ) ;
#117171 = CARTESIAN_POINT ( 'NONE',  ( 16.70850060796086822, 0.4765610498145367302, -5.930927070179643934 ) ) ;
#117172 = CARTESIAN_POINT ( 'NONE',  ( 186.9166666666666856, 6.668395609140176816, 3.850000000000000977 ) ) ;
#117173 = VERTEX_POINT ( 'NONE', #22648 ) ;
#117174 = CARTESIAN_POINT ( 'NONE',  ( 162.5000000000000000, -0.5000000000000000000, -7.500000000000005329 ) ) ;
#117175 = FACE_OUTER_BOUND ( 'NONE', #58228, .T. ) ;
#117176 = FACE_OUTER_BOUND ( 'NONE', #36510, .T. ) ;
#117177 = AXIS2_PLACEMENT_3D ( 'NONE', #71390, #41960, #72071 ) ;
#117178 = VERTEX_POINT ( 'NONE', #31814 ) ;
#117179 = EDGE_CURVE ( 'NONE', #114690, #10201, #103427, .T. ) ;
#117180 = CARTESIAN_POINT ( 'NONE',  ( 12.04999999999990479, 12.50000000000000000, 2.165063509461097713 ) ) ;
#117181 = CARTESIAN_POINT ( 'NONE',  ( 7.699999999999923794, 2.500000000000000000, -0.2464101615137783419 ) ) ;
#117182 = CARTESIAN_POINT ( 'NONE',  ( 7.299999999999926104, 2.500000000000000000, -0.4464101615137782142 ) ) ;
#117183 = CARTESIAN_POINT ( 'NONE',  ( 18.46077493896295607, -0.2575262203714185349, -4.048716073870159526 ) ) ;
#117184 = ORIENTED_EDGE ( 'NONE', *, *, #6504, .F. ) ;
#117185 = CARTESIAN_POINT ( 'NONE',  ( 3.099999999999945466, 2.500000000000000000, 0.4464101615137735513 ) ) ;
#117186 = ORIENTED_EDGE ( 'NONE', *, *, #103651, .F. ) ;
#117187 = DIRECTION ( 'NONE',  ( -0.000000000000000000, -1.000000000000000000, -0.000000000000000000 ) ) ;
#117188 = DIRECTION ( 'NONE',  ( 0.000000000000000000, 0.000000000000000000, 1.000000000000000000 ) ) ;
#117189 = AXIS2_PLACEMENT_3D ( 'NONE', #35087, #114267, #44900 ) ;
#117190 = ORIENTED_EDGE ( 'NONE', *, *, #64167, .F. ) ;
#117192 = ADVANCED_FACE ( 'NONE', ( #112946 ), #80449, .T. ) ;
#117191 = DIRECTION ( 'NONE',  ( 0.000000000000000000, -0.9999939076577903929, 0.003490651415223739937 ) ) ;
#117193 = DIRECTION ( 'NONE',  ( 0.000000000000000000, 0.000000000000000000, -1.000000000000000000 ) ) ;
#117194 = DIRECTION ( 'NONE',  ( 0.000000000000000000, 1.000000000000000000, 0.000000000000000000 ) ) ;
#117195 = FACE_OUTER_BOUND ( 'NONE', #20921, .T. ) ;
#117196 = VERTEX_POINT ( 'NONE', #62573 ) ;
#117197 = FACE_OUTER_BOUND ( 'NONE', #56092, .T. ) ;
#117198 = DIRECTION ( 'NONE',  ( 0.000000000000000000, 0.000000000000000000, -1.000000000000000000 ) ) ;
#117199 = EDGE_CURVE ( 'NONE', #98888, #20569, #111662, .T. ) ;
#117200 = EDGE_CURVE ( 'NONE', #39357, #105467, #12788, .T. ) ;
#117201 = CARTESIAN_POINT ( 'NONE',  ( 6.249999999999932498, 2.500000000000000000, -2.857883832488653741 ) ) ;
#117202 = LINE ( 'NONE', #58966, #79955 ) ;
#117203 = EDGE_CURVE ( 'NONE', #41353, #51914, #72128, .T. ) ;
#117204 = EDGE_CURVE ( 'NONE', #83387, #78182, #52731, .T. ) ;
#117205 = FACE_OUTER_BOUND ( 'NONE', #10519, .T. ) ;
#117206 = AXIS2_PLACEMENT_3D ( 'NONE', #71269, #93500, #22844 ) ;
#117207 = ORIENTED_EDGE ( 'NONE', *, *, #31477, .T. ) ;
#117208 = CIRCLE ( 'NONE', #48291, 0.06509327318403745899 ) ;
#117209 = ORIENTED_EDGE ( 'NONE', *, *, #68476, .F. ) ;
#117210 = CARTESIAN_POINT ( 'NONE',  ( -11.44999999999999751, 12.50000000000000000, 2.446380397790835826 ) ) ;
#117212 = ORIENTED_EDGE ( 'NONE', *, *, #42465, .T. ) ;
#117211 = EDGE_CURVE ( 'NONE', #115271, #30923, #45040, .T. ) ;
#117213 = DIRECTION ( 'NONE',  ( 0.000000000000000000, 0.000000000000000000, -1.000000000000000000 ) ) ;
#117215 = VERTEX_POINT ( 'NONE', #116795 ) ;
#117214 = VERTEX_POINT ( 'NONE', #104413 ) ;
#117216 = ORIENTED_EDGE ( 'NONE', *, *, #78991, .F. ) ;
#117217 = EDGE_CURVE ( 'NONE', #99388, #29668, #76251, .T. ) ;
#117218 = DIRECTION ( 'NONE',  ( -0.000000000000000000, -1.000000000000000000, -0.000000000000000000 ) ) ;
#117219 = EDGE_CURVE ( 'NONE', #121539, #108936, #66412, .T. ) ;
#117220 = CARTESIAN_POINT ( 'NONE',  ( 4.349999999999937472, 2.500000000000000000, 6.841600689897072485 ) ) ;
#117221 = EDGE_CURVE ( 'NONE', #75789, #11464, #80540, .T. ) ;
#117222 = CARTESIAN_POINT ( 'NONE',  ( 6.849999999999927702, 2.500000000000000000, 1.718653347947321386 ) ) ;
#117223 = DIRECTION ( 'NONE',  ( 0.000000000000000000, 1.000000000000000000, 0.000000000000000000 ) ) ;
#117224 = AXIS2_PLACEMENT_3D ( 'NONE', #91931, #11432, #82110 ) ;
#117225 = CARTESIAN_POINT ( 'NONE',  ( 9.999999999999916511, 2.500000000000000000, -0.5928203230275541635 ) ) ;
#117226 = DIRECTION ( 'NONE',  ( -0.000000000000000000, -1.000000000000000000, -0.000000000000000000 ) ) ;
#117227 = DIRECTION ( 'NONE',  ( -0.000000000000000000, -1.000000000000000000, -0.000000000000000000 ) ) ;
#117228 = ORIENTED_EDGE ( 'NONE', *, *, #89731, .T. ) ;
#117229 = ADVANCED_FACE ( 'NONE', ( #25195 ), #103518, .T. ) ;
#117230 = DIRECTION ( 'NONE',  ( -0.000000000000000000, -1.000000000000000000, -0.000000000000000000 ) ) ;
#117231 = ORIENTED_EDGE ( 'NONE', *, *, #14407, .T. ) ;
#117232 = ORIENTED_EDGE ( 'NONE', *, *, #38089, .T. ) ;
#117233 = ORIENTED_EDGE ( 'NONE', *, *, #30480, .F. ) ;
#117234 = ORIENTED_EDGE ( 'NONE', *, *, #91346, .T. ) ;
#117235 = LINE ( 'NONE', #57041, #96567 ) ;
#117236 = EDGE_LOOP ( 'NONE', ( #96627, #122863, #90708, #2302 ) ) ;
#117237 = ORIENTED_EDGE ( 'NONE', *, *, #46908, .T. ) ;
#117238 = CARTESIAN_POINT ( 'NONE',  ( -7.900000000000014566, 2.500000000000000000, 0.6928203230275494784 ) ) ;
#117239 = DIRECTION ( 'NONE',  ( 0.000000000000000000, 0.000000000000000000, -1.000000000000000000 ) ) ;
#117240 = CARTESIAN_POINT ( 'NONE',  ( -0.2000000000000399791, 12.50000000000000000, -4.676537180435977881 ) ) ;
#117241 = DIRECTION ( 'NONE',  ( 0.000000000000000000, 0.000000000000000000, 1.000000000000000000 ) ) ;
#117242 = AXIS2_PLACEMENT_3D ( 'NONE', #708, #19045, #39385 ) ;
#117243 = CARTESIAN_POINT ( 'NONE',  ( -6.650000000000014566, 2.500000000000000000, 5.902370205355745192 ) ) ;
#117244 = ORIENTED_EDGE ( 'NONE', *, *, #36538, .F. ) ;
#117245 = AXIS2_PLACEMENT_3D ( 'NONE', #21834, #11353, #82688 ) ;
#117246 = CONICAL_SURFACE ( 'NONE', #96332, 0.1000000000000000472, 0.003490658503988666988 ) ;
#117247 = CARTESIAN_POINT ( 'NONE',  ( 186.5000000000000000, 0.000000000000000000, 0.000000000000000000 ) ) ;
#117248 = ORIENTED_EDGE ( 'NONE', *, *, #24188, .T. ) ;
#117249 = CARTESIAN_POINT ( 'NONE',  ( 7.049999999999930544, 12.50000000000000000, -6.495190528383302464 ) ) ;
#117250 = AXIS2_PLACEMENT_3D ( 'NONE', #122483, #44558, #73364 ) ;
#117251 = ORIENTED_EDGE ( 'NONE', *, *, #127160, .F. ) ;
#117252 = DIRECTION ( 'NONE',  ( 0.000000000000000000, 0.000000000000000000, 1.000000000000000000 ) ) ;
#117253 = VERTEX_POINT ( 'NONE', #5555 ) ;
#117254 = ORIENTED_EDGE ( 'NONE', *, *, #28598, .T. ) ;
#117255 = LINE ( 'NONE', #109395, #123461 ) ;
#117256 = DIRECTION ( 'NONE',  ( 0.000000000000000000, 1.000000000000000000, 0.000000000000000000 ) ) ;
#117257 = EDGE_CURVE ( 'NONE', #119203, #70042, #111839, .T. ) ;
#117258 = DIRECTION ( 'NONE',  ( -0.000000000000000000, -1.000000000000000000, -0.000000000000000000 ) ) ;
#117259 = DIRECTION ( 'NONE',  ( 0.000000000000000000, 1.000000000000000000, 0.000000000000000000 ) ) ;
#117260 = EDGE_CURVE ( 'NONE', #45163, #111163, #124048, .T. ) ;
#117261 = CARTESIAN_POINT ( 'NONE',  ( -14.34999999999998543, 2.500000000000000000, -2.411473670974875638 ) ) ;
#117262 = EDGE_LOOP ( 'NONE', ( #62598, #12663, #118767, #93866 ) ) ;
#117263 = DIRECTION ( 'NONE',  ( -0.000000000000000000, -1.000000000000000000, -0.000000000000000000 ) ) ;
#117264 = CARTESIAN_POINT ( 'NONE',  ( 2.899999999999946620, 12.50000000000000000, 0.6928203230275494784 ) ) ;
#117265 = LINE ( 'NONE', #116004, #68985 ) ;
#117266 = FACE_OUTER_BOUND ( 'NONE', #49559, .T. ) ;
#117267 = ADVANCED_FACE ( 'NONE', ( #6193 ), #120247, .T. ) ;
#117268 = FACE_OUTER_BOUND ( 'NONE', #38716, .T. ) ;
#117269 = ORIENTED_EDGE ( 'NONE', *, *, #9797, .T. ) ;
#117270 = AXIS2_PLACEMENT_3D ( 'NONE', #123509, #14825, #33233 ) ;
#117271 = ORIENTED_EDGE ( 'NONE', *, *, #40031, .F. ) ;
#117272 = CARTESIAN_POINT ( 'NONE',  ( 6.049999999999934097, 12.50000000000000000, -6.148780366869526226 ) ) ;
#117273 = ORIENTED_EDGE ( 'NONE', *, *, #5145, .T. ) ;
#117274 = LINE ( 'NONE', #67540, #21548 ) ;
#117275 = CIRCLE ( 'NONE', #60869, 0.1000000000000002554 ) ;
#117276 = CARTESIAN_POINT ( 'NONE',  ( 15.39999999999989200, 2.500000000000000000, -0.6928203230275542523 ) ) ;
#117277 = ORIENTED_EDGE ( 'NONE', *, *, #60365, .F. ) ;
#117278 = CARTESIAN_POINT ( 'NONE',  ( 186.7916666666666572, 4.445597072760120838, -7.699999999999998401 ) ) ;
#117279 = DIRECTION ( 'NONE',  ( 0.000000000000000000, 0.000000000000000000, -1.000000000000000000 ) ) ;
#117280 = CARTESIAN_POINT ( 'NONE',  ( -7.499999999999980460, 12.50000000000000000, -4.395220292106239768 ) ) ;
#117281 = DIRECTION ( 'NONE',  ( 0.000000000000000000, 0.000000000000000000, 1.000000000000000000 ) ) ;
#117282 = ORIENTED_EDGE ( 'NONE', *, *, #2352, .T. ) ;
#117283 = CONICAL_SURFACE ( 'NONE', #39965, 0.1000000000000002554, 0.003490658503988666988 ) ;
#117284 = DIRECTION ( 'NONE',  ( 0.000000000000000000, 1.000000000000000000, 0.000000000000000000 ) ) ;
#117285 = DIRECTION ( 'NONE',  ( 0.000000000000000000, 0.000000000000000000, 1.000000000000000000 ) ) ;
#117286 = VERTEX_POINT ( 'NONE', #86037 ) ;
#117287 = FACE_OUTER_BOUND ( 'NONE', #81903, .T. ) ;
#117288 = DIRECTION ( 'NONE',  ( -0.000000000000000000, 1.000000000000000000, -0.000000000000000000 ) ) ;
#117289 = FACE_OUTER_BOUND ( 'NONE', #101322, .T. ) ;
#117290 = AXIS2_PLACEMENT_3D ( 'NONE', #90096, #58728, #18787 ) ;
#117291 = AXIS2_PLACEMENT_3D ( 'NONE', #14760, #54695, #44910 ) ;
#117292 = ORIENTED_EDGE ( 'NONE', *, *, #110957, .T. ) ;
#117293 = DIRECTION ( 'NONE',  ( -0.000000000000000000, -1.000000000000000000, -0.000000000000000000 ) ) ;
#117294 = ORIENTED_EDGE ( 'NONE', *, *, #13674, .F. ) ;
#117295 = DIRECTION ( 'NONE',  ( 0.000000000000000000, 1.000000000000000000, 0.000000000000000000 ) ) ;
#117296 = DIRECTION ( 'NONE',  ( 0.000000000000000000, 1.000000000000000000, 0.000000000000000000 ) ) ;
#117297 = CONICAL_SURFACE ( 'NONE', #14894, 0.1000000000000000472, 0.003490658503988666988 ) ;
#117298 = CARTESIAN_POINT ( 'NONE',  ( -1.250000000000001110, 12.50000000000000000, -6.495190528383302464 ) ) ;
#117299 = EDGE_LOOP ( 'NONE', ( #11024, #90247 ) ) ;
#117300 = DIRECTION ( 'NONE',  ( 0.000000000000000000, -0.9999939076577903929, 0.003490651415223739937 ) ) ;
#117301 = CARTESIAN_POINT ( 'NONE',  ( -10.80000000000000071, 2.500000000000000000, 0.09999999999999772959 ) ) ;
#117302 = CIRCLE ( 'NONE', #33806, 0.1000000000000000472 ) ;
#117303 = CIRCLE ( 'NONE', #19035, 0.06509327318403745899 ) ;
#117304 = EDGE_CURVE ( 'NONE', #9105, #106026, #63815, .T. ) ;
#117305 = ORIENTED_EDGE ( 'NONE', *, *, #19733, .F. ) ;
#117306 = LINE ( 'NONE', #47324, #2969 ) ;
#117307 = ADVANCED_FACE ( 'NONE', ( #15364 ), #70068, .T. ) ;
#117308 = VERTEX_POINT ( 'NONE', #46135 ) ;
#117309 = DIRECTION ( 'NONE',  ( 0.000000000000000000, 1.000000000000000000, 0.000000000000000000 ) ) ;
#117310 = ORIENTED_EDGE ( 'NONE', *, *, #115651, .F. ) ;
#117311 = CARTESIAN_POINT ( 'NONE',  ( -6.050000000000022027, 12.50000000000000000, -6.148780366869526226 ) ) ;
#117312 = DIRECTION ( 'NONE',  ( 0.000000000000000000, 1.000000000000000000, 0.000000000000000000 ) ) ;
#117313 = VERTEX_POINT ( 'NONE', #106970 ) ;
#117314 = EDGE_CURVE ( 'NONE', #46749, #92080, #32444, .T. ) ;
#117315 = ORIENTED_EDGE ( 'NONE', *, *, #127267, .F. ) ;
#117316 = DIRECTION ( 'NONE',  ( 0.000000000000000000, 0.000000000000000000, 1.000000000000000000 ) ) ;
#117317 = LINE ( 'NONE', #27669, #109085 ) ;
#117318 = ORIENTED_EDGE ( 'NONE', *, *, #80617, .T. ) ;
#117319 = DIRECTION ( 'NONE',  ( -0.000000000000000000, 1.000000000000000000, -0.000000000000000000 ) ) ;
#117320 = CARTESIAN_POINT ( 'NONE',  ( 1.849999999999950573, 2.500000000000000000, 2.511473670974873507 ) ) ;
#117321 = AXIS2_PLACEMENT_3D ( 'NONE', #5851, #96817, #76548 ) ;
#117322 = CARTESIAN_POINT ( 'NONE',  ( 15.79999999999989058, 12.50000000000000000, -2.385244779468109755E-15 ) ) ;
#117323 = DIRECTION ( 'NONE',  ( 0.000000000000000000, 0.000000000000000000, -1.000000000000000000 ) ) ;
#117324 = AXIS2_PLACEMENT_3D ( 'NONE', #57062, #70760, #4404 ) ;
#117325 = VECTOR ( 'NONE', #29695, 1000.000000000000000 ) ;
#117326 = CARTESIAN_POINT ( 'NONE',  ( -4.150000000000027889, 2.500000000000000000, -7.088010851410853519 ) ) ;
#117327 = FACE_OUTER_BOUND ( 'NONE', #16363, .T. ) ;
#117328 = AXIS2_PLACEMENT_3D ( 'NONE', #13642, #2524, #43782 ) ;
#117329 = ORIENTED_EDGE ( 'NONE', *, *, #44430, .T. ) ;
#117331 = ORIENTED_EDGE ( 'NONE', *, *, #70404, .F. ) ;
#117330 = EDGE_CURVE ( 'NONE', #35601, #34064, #1099, .T. ) ;
#117332 = VERTEX_POINT ( 'NONE', #106345 ) ;
#117333 = ORIENTED_EDGE ( 'NONE', *, *, #47482, .F. ) ;
#117334 = FACE_OUTER_BOUND ( 'NONE', #1951, .T. ) ;
#117335 = DIRECTION ( 'NONE',  ( -0.000000000000000000, -1.000000000000000000, -0.000000000000000000 ) ) ;
#117336 = CONICAL_SURFACE ( 'NONE', #94383, 0.1000000000000000472, 0.003490658503988666988 ) ;
#117337 = DIRECTION ( 'NONE',  ( -0.000000000000000000, 1.000000000000000000, -0.000000000000000000 ) ) ;
#117338 = ORIENTED_EDGE ( 'NONE', *, *, #64193, .T. ) ;
#117339 = FACE_BOUND ( 'NONE', #43183, .T. ) ;
#117340 = ORIENTED_EDGE ( 'NONE', *, *, #122780, .F. ) ;
#117341 = CARTESIAN_POINT ( 'NONE',  ( -6.250000000000017764, 12.50000000000000000, 7.188010851410848723 ) ) ;
#117342 = CARTESIAN_POINT ( 'NONE',  ( -5.850000000000018296, 2.500000000000000000, 2.957883832488649389 ) ) ;
#117344 = ADVANCED_FACE ( 'NONE', ( #34409 ), #90992, .T. ) ;
#117343 = CARTESIAN_POINT ( 'NONE',  ( -6.900000000000019007, 12.50000000000000000, -0.3464101615137783474 ) ) ;
#117345 = DIRECTION ( 'NONE',  ( 0.000000000000000000, -0.9999939076577903929, 0.003490651415223739937 ) ) ;
#117346 = CARTESIAN_POINT ( 'NONE',  ( 17.49862860983209600, -2.500000000000000000, 4.081131818001135336 ) ) ;
#117347 = CARTESIAN_POINT ( 'NONE',  ( 14.59999999999989484, 2.500000000000000000, 0.7928203230275495672 ) ) ;
#117348 = DIRECTION ( 'NONE',  ( 0.000000000000000000, 0.000000000000000000, 1.000000000000000000 ) ) ;
#117349 = DIRECTION ( 'NONE',  ( -0.000000000000000000, -1.000000000000000000, -0.000000000000000000 ) ) ;
#117350 = EDGE_CURVE ( 'NONE', #44383, #41372, #84118, .T. ) ;
#117351 = ADVANCED_FACE ( 'NONE', ( #74317 ), #28303, .T. ) ;
#117352 = CARTESIAN_POINT ( 'NONE',  ( -0.6000000000000388356, 2.500000000000000000, 3.983716857408420964 ) ) ;
#117353 = ADVANCED_FACE ( 'NONE', ( #56580 ), #105576, .T. ) ;
#117354 = EDGE_CURVE ( 'NONE', #14513, #54407, #11560, .T. ) ;
#117355 = CARTESIAN_POINT ( 'NONE',  ( 6.899999999999926636, 2.500000000000000000, -0.4464101615137782142 ) ) ;
#117356 = ORIENTED_EDGE ( 'NONE', *, *, #14086, .T. ) ;
#117357 = EDGE_LOOP ( 'NONE', ( #18134, #88108, #95188, #85020 ) ) ;
#117358 = EDGE_LOOP ( 'NONE', ( #73799, #7291 ) ) ;
#117359 = ORIENTED_EDGE ( 'NONE', *, *, #14550, .F. ) ;
#117360 = DIRECTION ( 'NONE',  ( 0.000000000000000000, 1.000000000000000000, 0.000000000000000000 ) ) ;
#117361 = EDGE_CURVE ( 'NONE', #23570, #32403, #4906, .T. ) ;
#117362 = DIRECTION ( 'NONE',  ( 0.000000000000000000, 0.000000000000000000, -1.000000000000000000 ) ) ;
#117365 = VERTEX_POINT ( 'NONE', #129241 ) ;
#117364 = ORIENTED_EDGE ( 'NONE', *, *, #63441, .F. ) ;
#117363 = EDGE_CURVE ( 'NONE', #113534, #76503, #127919, .T. ) ;
#117366 = ORIENTED_EDGE ( 'NONE', *, *, #15042, .F. ) ;
#117367 = DIRECTION ( 'NONE',  ( -4.274815082592931898E-19, -0.9999939076577903929, -0.003490651415223739937 ) ) ;
#117368 = AXIS2_PLACEMENT_3D ( 'NONE', #3803, #24736, #43754 ) ;
#117370 = EDGE_CURVE ( 'NONE', #8727, #43078, #84731, .T. ) ;
#117369 = CONICAL_SURFACE ( 'NONE', #12820, 0.1000000000000002554, 0.003490658503988666988 ) ;
#117371 = EDGE_CURVE ( 'NONE', #114782, #45293, #101463, .T. ) ;
#117372 = CARTESIAN_POINT ( 'NONE',  ( -3.749999999999991118, 2.500000000000000000, -2.165063509461101710 ) ) ;
#117373 = CARTESIAN_POINT ( 'NONE',  ( 3.549999999999943867, 12.50000000000000000, -1.883746621131363597 ) ) ;
#117374 = CARTESIAN_POINT ( 'NONE',  ( 0.6499999999999561684, 2.500000000000000000, -1.818653347947325916 ) ) ;
#117375 = CARTESIAN_POINT ( 'NONE',  ( 8.099999999999921485, 12.50000000000000000, 0.3464101615137735735 ) ) ;
#117376 = DIRECTION ( 'NONE',  ( 0.000000000000000000, 1.000000000000000000, 0.000000000000000000 ) ) ;
#117377 = ADVANCED_FACE ( 'NONE', ( #58551 ), #49159, .T. ) ;
#117378 = VERTEX_POINT ( 'NONE', #117420 ) ;
#117380 = EDGE_CURVE ( 'NONE', #104514, #16978, #68350, .T. ) ;
#117379 = AXIS2_PLACEMENT_3D ( 'NONE', #11717, #121668, #22209 ) ;
#117381 = VECTOR ( 'NONE', #125633, 1000.000000000000000 ) ;
#117382 = DIRECTION ( 'NONE',  ( -0.000000000000000000, 1.000000000000000000, -0.000000000000000000 ) ) ;
#117383 = ORIENTED_EDGE ( 'NONE', *, *, #57166, .T. ) ;
#117384 = EDGE_LOOP ( 'NONE', ( #93762, #36410 ) ) ;
#117385 = AXIS2_PLACEMENT_3D ( 'NONE', #29256, #1062, #69148 ) ;
#117386 = EDGE_LOOP ( 'NONE', ( #19575, #88059, #51197, #88148 ) ) ;
#117387 = CARTESIAN_POINT ( 'NONE',  ( 9.799999999999915445, 2.500000000000000000, -4.676537180435977881 ) ) ;
#117388 = ORIENTED_EDGE ( 'NONE', *, *, #59188, .T. ) ;
#117389 = ORIENTED_EDGE ( 'NONE', *, *, #108190, .F. ) ;
#117390 = CIRCLE ( 'NONE', #54708, 0.06509327318403745899 ) ;
#117391 = DIRECTION ( 'NONE',  ( -0.000000000000000000, 1.000000000000000000, -0.000000000000000000 ) ) ;
#117392 = VECTOR ( 'NONE', #126534, 1000.000000000000000 ) ;
#117393 = DIRECTION ( 'NONE',  ( -4.274815082592931898E-19, -0.9999939076577903929, -0.003490651415223739937 ) ) ;
#117394 = DIRECTION ( 'NONE',  ( 0.000000000000000000, -0.9999939076577903929, 0.003490651415223739937 ) ) ;
#117395 = CARTESIAN_POINT ( 'NONE',  ( -8.150000000000012790, 2.500000000000000000, -1.918653347947326004 ) ) ;
#117396 = CONICAL_SURFACE ( 'NONE', #60984, 0.1000000000000002554, 0.003490658503988666988 ) ;
#117397 = DIRECTION ( 'NONE',  ( 0.000000000000000000, -0.9999939076577903929, 0.003490651415223739937 ) ) ;
#117398 = CIRCLE ( 'NONE', #25476, 0.06509327318403745899 ) ;
#117399 = EDGE_LOOP ( 'NONE', ( #95203, #43940 ) ) ;
#117400 = DIRECTION ( 'NONE',  ( 0.000000000000000000, -0.9999939076577903929, 0.003490651415223739937 ) ) ;
#117401 = ORIENTED_EDGE ( 'NONE', *, *, #94030, .T. ) ;
#117402 = CARTESIAN_POINT ( 'NONE',  ( 186.1250000000000000, -8.891194145520236347, -1.633285867636356299E-15 ) ) ;
#117403 = VERTEX_POINT ( 'NONE', #98441 ) ;
#117404 = CARTESIAN_POINT ( 'NONE',  ( 108.3389004593042415, 7.119691004531022216, -5.000000000000006217 ) ) ;
#117405 = CIRCLE ( 'NONE', #17138, 0.06509327318403745899 ) ;
#117406 = CONICAL_SURFACE ( 'NONE', #33807, 0.1000000000000000056, 0.003490658503988666988 ) ;
#117407 = DIRECTION ( 'NONE',  ( -0.000000000000000000, 1.000000000000000000, -0.000000000000000000 ) ) ;
#117408 = ORIENTED_EDGE ( 'NONE', *, *, #4933, .T. ) ;
#117409 = FACE_OUTER_BOUND ( 'NONE', #93902, .T. ) ;
#117410 = DIRECTION ( 'NONE',  ( -0.000000000000000000, -1.000000000000000000, -0.000000000000000000 ) ) ;
#117411 = ORIENTED_EDGE ( 'NONE', *, *, #43148, .F. ) ;
#117412 = EDGE_CURVE ( 'NONE', #66216, #96385, #38793, .T. ) ;
#117413 = CARTESIAN_POINT ( 'NONE',  ( 8.949999999999919353, 2.500000000000000000, -6.148780366869526226 ) ) ;
#117414 = EDGE_CURVE ( 'NONE', #109336, #125197, #17825, .T. ) ;
#117415 = ORIENTED_EDGE ( 'NONE', *, *, #52507, .F. ) ;
#117416 = ORIENTED_EDGE ( 'NONE', *, *, #72169, .F. ) ;
#117417 = DIRECTION ( 'NONE',  ( 0.000000000000000000, 0.000000000000000000, -1.000000000000000000 ) ) ;
#117418 = DIRECTION ( 'NONE',  ( 0.000000000000000000, 0.000000000000000000, 1.000000000000000000 ) ) ;
#117419 = CARTESIAN_POINT ( 'NONE',  ( 186.2968750003414584, 8.734944146203032389, 5.348610694689227483E-16 ) ) ;
#117420 = CARTESIAN_POINT ( 'NONE',  ( -15.59999999999998010, 2.500000000000000000, 0.4464101615137759382 ) ) ;
#117421 = LINE ( 'NONE', #16016, #22796 ) ;
#117422 = DIRECTION ( 'NONE',  ( -4.274815082592931898E-19, -0.9999939076577903929, -0.003490651415223739937 ) ) ;
#117423 = AXIS2_PLACEMENT_3D ( 'NONE', #115667, #26021, #67186 ) ;
#117424 = AXIS2_PLACEMENT_3D ( 'NONE', #85236, #15841, #34222 ) ;
#117425 = ORIENTED_EDGE ( 'NONE', *, *, #44258, .T. ) ;
#117426 = CARTESIAN_POINT ( 'NONE',  ( -5.800000000000018474, 12.50000000000000000, 4.330127018922196314 ) ) ;
#117427 = CARTESIAN_POINT ( 'NONE',  ( -11.44999999999999929, 2.500000000000000000, -1.718653347947322052 ) ) ;
#117428 = AXIS2_PLACEMENT_3D ( 'NONE', #115962, #127084, #46563 ) ;
#117429 = ORIENTED_EDGE ( 'NONE', *, *, #43347, .F. ) ;
#117430 = AXIS2_PLACEMENT_3D ( 'NONE', #7583, #58644, #37071 ) ;
#117431 = CONICAL_SURFACE ( 'NONE', #52717, 0.1000000000000000472, 0.003490658503988666988 ) ;
#117432 = CARTESIAN_POINT ( 'NONE',  ( -5.000000000000022204, 12.50000000000000000, -0.6928203230275541413 ) ) ;
#117433 = CARTESIAN_POINT ( 'NONE',  ( -0.8500000000000382805, 12.50000000000000000, -1.472243186433550122 ) ) ;
#117434 = CARTESIAN_POINT ( 'NONE',  ( -1.250000000000035749, 2.500000000000000000, -2.857883832488653741 ) ) ;
#117435 = CARTESIAN_POINT ( 'NONE',  ( 179.5000000000000000, 0.6250000000000028866, -7.634788798650556707 ) ) ;
#117436 = CARTESIAN_POINT ( 'NONE',  ( 8.949999999999917577, 2.500000000000000000, -2.511473670974877948 ) ) ;
#117437 = ORIENTED_EDGE ( 'NONE', *, *, #7895, .T. ) ;
#117438 = AXIS2_PLACEMENT_3D ( 'NONE', #41720, #81618, #111730 ) ;
#117439 = CARTESIAN_POINT ( 'NONE',  ( -12.89999999999999325, 2.500000000000000000, -3.637306695894647390 ) ) ;
#117440 = SURFACE_STYLE_FILL_AREA ( #19258 ) ;
#117441 = EDGE_LOOP ( 'NONE', ( #71250, #101791 ) ) ;
#117442 = DIRECTION ( 'NONE',  ( -0.000000000000000000, 1.000000000000000000, -0.000000000000000000 ) ) ;
#117443 = ADVANCED_FACE ( 'NONE', ( #87968 ), #108276, .T. ) ;
#117444 = ORIENTED_EDGE ( 'NONE', *, *, #38950, .T. ) ;
#117445 = VERTEX_POINT ( 'NONE', #48728 ) ;
#117446 = DIRECTION ( 'NONE',  ( 0.000000000000000000, 1.000000000000000000, 0.000000000000000000 ) ) ;
#117447 = VERTEX_POINT ( 'NONE', #27773 ) ;
#117448 = CARTESIAN_POINT ( 'NONE',  ( -1.650000000000034328, 2.500000000000000000, -7.288010851410854585 ) ) ;
#117449 = DIRECTION ( 'NONE',  ( 0.000000000000000000, 0.000000000000000000, 1.000000000000000000 ) ) ;
#117450 = CARTESIAN_POINT ( 'NONE',  ( 4.999999999999936939, 12.50000000000000000, -0.7579135962115916003 ) ) ;
#117451 = CONICAL_SURFACE ( 'NONE', #100748, 0.09999999999999982514, 0.003490658503988666988 ) ;
#117452 = ORIENTED_EDGE ( 'NONE', *, *, #129559, .T. ) ;
#117453 = AXIS2_PLACEMENT_3D ( 'NONE', #47266, #114692, #87164 ) ;
#117454 = DIRECTION ( 'NONE',  ( -0.000000000000000000, 1.000000000000000000, -0.000000000000000000 ) ) ;
#117456 = ORIENTED_EDGE ( 'NONE', *, *, #32552, .T. ) ;
#117455 = CARTESIAN_POINT ( 'NONE',  ( 9.799999999999917222, 2.500000000000000000, 0.3464101615137735735 ) ) ;
#117457 = EDGE_CURVE ( 'NONE', #67849, #35226, #47096, .T. ) ;
#117458 = DIRECTION ( 'NONE',  ( 0.000000000000000000, 1.000000000000000000, 0.000000000000000000 ) ) ;
#117459 = LINE ( 'NONE', #21721, #59305 ) ;
#117460 = EDGE_CURVE ( 'NONE', #119760, #127429, #57907, .T. ) ;
#117461 = AXIS2_PLACEMENT_3D ( 'NONE', #13643, #93508, #3833 ) ;
#117462 = ORIENTED_EDGE ( 'NONE', *, *, #119476, .T. ) ;
#117463 = CIRCLE ( 'NONE', #56836, 0.06509327318403745899 ) ;
#117464 = AXIS2_PLACEMENT_3D ( 'NONE', #112316, #4915, #122775 ) ;
#117465 = ORIENTED_EDGE ( 'NONE', *, *, #110717, .F. ) ;
#117466 = ORIENTED_EDGE ( 'NONE', *, *, #33016, .F. ) ;
#117467 = DIRECTION ( 'NONE',  ( 0.000000000000000000, 0.000000000000000000, -1.000000000000000000 ) ) ;
#117468 = LINE ( 'NONE', #127968, #81276 ) ;
#117469 = CARTESIAN_POINT ( 'NONE',  ( 14.14999999999989377, 2.500000000000000000, -2.857883832488653741 ) ) ;
#117470 =( REPRESENTATION_RELATIONSHIP ('NONE','NONE', #102928, #120523 ) REPRESENTATION_RELATIONSHIP_WITH_TRANSFORMATION ( #69937 )SHAPE_REPRESENTATION_RELATIONSHIP( ) );
#117471 = ADVANCED_FACE ( 'NONE', ( #37620 ), #59196, .T. ) ;
#117472 = FACE_BOUND ( 'NONE', #45107, .T. ) ;
#117473 = ORIENTED_EDGE ( 'NONE', *, *, #36262, .F. ) ;
#117474 = DIRECTION ( 'NONE',  ( 0.000000000000000000, -0.000000000000000000, 1.000000000000000000 ) ) ;
#117475 = DIRECTION ( 'NONE',  ( 0.000000000000000000, 0.000000000000000000, 1.000000000000000000 ) ) ;
#117476 = AXIS2_PLACEMENT_3D ( 'NONE', #3985, #24284, #64198 ) ;
#117477 = VERTEX_POINT ( 'NONE', #67699 ) ;
#117478 = AXIS2_PLACEMENT_3D ( 'NONE', #7381, #47332, #42014 ) ;
#117479 = CARTESIAN_POINT ( 'NONE',  ( 184.8333333333333144, 6.668395609140177704, -3.849999999999998312 ) ) ;
#117480 = CIRCLE ( 'NONE', #127980, 0.06509327318403745899 ) ;
#117481 = AXIS2_PLACEMENT_3D ( 'NONE', #77340, #26957, #89100 ) ;
#117482 = CIRCLE ( 'NONE', #19302, 0.1000000000000002554 ) ;
#117483 = FACE_OUTER_BOUND ( 'NONE', #38713, .T. ) ;
#117484 = DIRECTION ( 'NONE',  ( 0.000000000000000000, 0.000000000000000000, -1.000000000000000000 ) ) ;
#117485 = DIRECTION ( 'NONE',  ( 0.000000000000000000, 0.000000000000000000, 1.000000000000000000 ) ) ;
#117486 = AXIS2_PLACEMENT_3D ( 'NONE', #9819, #80509, #81148 ) ;
#117487 = DIRECTION ( 'NONE',  ( -0.000000000000000000, -1.000000000000000000, -0.000000000000000000 ) ) ;
#117488 = ORIENTED_EDGE ( 'NONE', *, *, #79845, .T. ) ;
#117489 = AXIS2_PLACEMENT_3D ( 'NONE', #87734, #38005, #89685 ) ;
#117490 = ORIENTED_EDGE ( 'NONE', *, *, #93575, .F. ) ;
#117491 = EDGE_LOOP ( 'NONE', ( #84032, #128171, #125258, #25273 ) ) ;
#117492 = EDGE_LOOP ( 'NONE', ( #76053, #70321, #33732, #38083 ) ) ;
#117493 = EDGE_LOOP ( 'NONE', ( #6526, #116272, #188, #118350 ) ) ;
#117494 = DIRECTION ( 'NONE',  ( -0.000000000000000000, -1.000000000000000000, -0.000000000000000000 ) ) ;
#117495 = DIRECTION ( 'NONE',  ( 0.000000000000000000, 0.000000000000000000, -1.000000000000000000 ) ) ;
#117496 = ORIENTED_EDGE ( 'NONE', *, *, #86774, .F. ) ;
#117497 = FACE_BOUND ( 'NONE', #69874, .T. ) ;
#117498 = CARTESIAN_POINT ( 'NONE',  ( -11.04999999999999893, 12.50000000000000000, 1.883746621131358934 ) ) ;
#117499 = EDGE_CURVE ( 'NONE', #41725, #128844, #55398, .T. ) ;
#117500 = CARTESIAN_POINT ( 'NONE',  ( -3.750000000000026201, 2.500000000000000000, 5.802370205355744659 ) ) ;
#117501 = DIRECTION ( 'NONE',  ( 0.000000000000000000, -0.9999939076577903929, 0.003490651415223739937 ) ) ;
#117502 = CARTESIAN_POINT ( 'NONE',  ( -1.250000000000036193, 2.500000000000000000, 5.802370205355744659 ) ) ;
#117503 = ADVANCED_FACE ( 'NONE', ( #107640 ), #19903, .T. ) ;
#117504 = DIRECTION ( 'NONE',  ( 0.000000000000000000, 0.000000000000000000, -1.000000000000000000 ) ) ;
#117505 = ORIENTED_EDGE ( 'NONE', *, *, #126901, .F. ) ;
#117506 = LINE ( 'NONE', #1465, #17980 ) ;
#117507 = EDGE_CURVE ( 'NONE', #71451, #86508, #36637, .T. ) ;
#117508 = ORIENTED_EDGE ( 'NONE', *, *, #121368, .T. ) ;
#117509 = ORIENTED_EDGE ( 'NONE', *, *, #324, .T. ) ;
#117510 = CONICAL_SURFACE ( 'NONE', #77828, 0.1000000000000002554, 0.003490658503988666988 ) ;
#117511 = ORIENTED_EDGE ( 'NONE', *, *, #36901, .T. ) ;
#117512 = EDGE_CURVE ( 'NONE', #22290, #90888, #42997, .T. ) ;
#117513 = DIRECTION ( 'NONE',  ( 0.000000000000000000, 0.000000000000000000, -1.000000000000000000 ) ) ;
#117514 = VECTOR ( 'NONE', #67, 1000.000000000000000 ) ;
#117516 = EDGE_CURVE ( 'NONE', #72858, #30037, #19992, .T. ) ;
#117515 = DIRECTION ( 'NONE',  ( 0.000000000000000000, 0.000000000000000000, 1.000000000000000000 ) ) ;
#117517 = CARTESIAN_POINT ( 'NONE',  ( 129.5000000000000000, -0.6250000000000000000, 7.634788798650553154 ) ) ;
#117519 = ORIENTED_EDGE ( 'NONE', *, *, #101946, .F. ) ;
#117518 = EDGE_CURVE ( 'NONE', #63031, #2959, #10081, .T. ) ;
#117520 = CARTESIAN_POINT ( 'NONE',  ( 10.87377556668899814, 2.500000000000640821, -8.986829607521531926 ) ) ;
#117521 = EDGE_CURVE ( 'NONE', #34246, #28046, #5398, .T. ) ;
#117522 = DIRECTION ( 'NONE',  ( 0.000000000000000000, 0.000000000000000000, -1.000000000000000000 ) ) ;
#117523 = AXIS2_PLACEMENT_3D ( 'NONE', #32785, #11819, #62864 ) ;
#117524 = AXIS2_PLACEMENT_3D ( 'NONE', #52273, #103945, #3171 ) ;
#117525 = AXIS2_PLACEMENT_3D ( 'NONE', #102752, #34025, #54309 ) ;
#117527 = EDGE_CURVE ( 'NONE', #61622, #76508, #60491, .T. ) ;
#117526 = PLANE ( 'NONE',  #28618 ) ;
#117528 = CARTESIAN_POINT ( 'NONE',  ( 184.0729166673494603, 4.445597072760120838, -7.699999999999998401 ) ) ;
#117529 = CARTESIAN_POINT ( 'NONE',  ( 2.699999999999946443, 2.500000000000000000, -3.983716857408426293 ) ) ;
#117530 = DIRECTION ( 'NONE',  ( 0.000000000000000000, 1.000000000000000000, 0.000000000000000000 ) ) ;
#117531 = AXIS2_PLACEMENT_3D ( 'NONE', #118036, #108853, #68287 ) ;
#117532 = AXIS2_PLACEMENT_3D ( 'NONE', #16920, #85050, #45791 ) ;
#117533 = CARTESIAN_POINT ( 'NONE',  ( 8.549999999999920774, 2.500000000000000000, 6.248780366869521430 ) ) ;
#117534 = EDGE_LOOP ( 'NONE', ( #124393, #125456 ) ) ;
#117535 = DIRECTION ( 'NONE',  ( -4.274815082592931898E-19, -0.9999939076577903929, -0.003490651415223739937 ) ) ;
#117536 = ADVANCED_FACE ( 'NONE', ( #102333 ), #31037, .T. ) ;
#117537 = CIRCLE ( 'NONE', #88297, 0.09999999999999982514 ) ;
#117538 = VERTEX_POINT ( 'NONE', #51316 ) ;
#117539 = ORIENTED_EDGE ( 'NONE', *, *, #105157, .F. ) ;
#117540 = CARTESIAN_POINT ( 'NONE',  ( -1.450000000000035483, 12.50000000000000000, 1.818653347947321475 ) ) ;
#117541 = DIRECTION ( 'NONE',  ( -0.000000000000000000, -1.000000000000000000, -0.000000000000000000 ) ) ;
#117542 = DIRECTION ( 'NONE',  ( -0.000000000000000000, -1.000000000000000000, -0.000000000000000000 ) ) ;
#117543 = EDGE_LOOP ( 'NONE', ( #42094, #124747, #21839, #21734 ) ) ;
#117544 = VERTEX_POINT ( 'NONE', #123258 ) ;
#117545 = VECTOR ( 'NONE', #127319, 1000.000000000000000 ) ;
#117546 = CARTESIAN_POINT ( 'NONE',  ( -1.850000000000033396, 12.50000000000000000, -2.511473670974877948 ) ) ;
#117547 = CARTESIAN_POINT ( 'NONE',  ( 4.599999999999937472, 2.500000000000000000, 0.6928203230275494784 ) ) ;
#117548 = CARTESIAN_POINT ( 'NONE',  ( -10.84999999999999964, 2.500000000000000000, 5.802370205355744659 ) ) ;
#117549 = ORIENTED_EDGE ( 'NONE', *, *, #64170, .T. ) ;
#117550 = ORIENTED_EDGE ( 'NONE', *, *, #127785, .T. ) ;
#117551 = DIRECTION ( 'NONE',  ( -0.000000000000000000, -1.000000000000000000, -0.000000000000000000 ) ) ;
#117552 = ORIENTED_EDGE ( 'NONE', *, *, #71448, .F. ) ;
#117553 = DIRECTION ( 'NONE',  ( 0.000000000000000000, 0.000000000000000000, 1.000000000000000000 ) ) ;
#117554 = AXIS2_PLACEMENT_3D ( 'NONE', #22415, #72788, #121879 ) ;
#117555 = CARTESIAN_POINT ( 'NONE',  ( 108.0000000000000142, 9.000000000000001776, 0.000000000000000000 ) ) ;
#117556 = ORIENTED_EDGE ( 'NONE', *, *, #50221, .T. ) ;
#117557 = DIRECTION ( 'NONE',  ( 0.000000000000000000, 0.000000000000000000, 1.000000000000000000 ) ) ;
#117558 = DIRECTION ( 'NONE',  ( 0.000000000000000000, -0.000000000000000000, 1.000000000000000000 ) ) ;
#117559 = FACE_OUTER_BOUND ( 'NONE', #81379, .T. ) ;
#117561 = VECTOR ( 'NONE', #104452, 1000.000000000000000 ) ;
#117560 = CARTESIAN_POINT ( 'NONE',  ( -4.200000000000025935, 2.500000000000000000, 4.230127018922196669 ) ) ;
#117562 = ORIENTED_EDGE ( 'NONE', *, *, #129403, .F. ) ;
#117563 = AXIS2_PLACEMENT_3D ( 'NONE', #78810, #117391, #8736 ) ;
#117564 = AXIS2_PLACEMENT_3D ( 'NONE', #44629, #22433, #124481 ) ;
#117565 = DIRECTION ( 'NONE',  ( -0.000000000000000000, -1.000000000000000000, -0.000000000000000000 ) ) ;
#117566 = CIRCLE ( 'NONE', #75729, 0.1000000000000000472 ) ;
#117567 = EDGE_CURVE ( 'NONE', #59434, #90074, #32327, .T. ) ;
#117568 = EDGE_LOOP ( 'NONE', ( #17010, #35975 ) ) ;
#117569 = ORIENTED_EDGE ( 'NONE', *, *, #38060, .T. ) ;
#117570 = LINE ( 'NONE', #88788, #41610 ) ;
#117571 = LINE ( 'NONE', #28585, #118098 ) ;
#117572 = PLANE ( 'NONE',  #7113 ) ;
#117573 = DIRECTION ( 'NONE',  ( 0.000000000000000000, 0.000000000000000000, 1.000000000000000000 ) ) ;
#117574 = AXIS2_PLACEMENT_3D ( 'NONE', #79202, #119749, #81131 ) ;
#117575 = FACE_OUTER_BOUND ( 'NONE', #27723, .T. ) ;
#117576 = DIRECTION ( 'NONE',  ( -0.000000000000000000, 1.000000000000000000, -0.000000000000000000 ) ) ;
#117577 = VECTOR ( 'NONE', #59601, 1000.000000000000000 ) ;
#117578 = EDGE_CURVE ( 'NONE', #58093, #84838, #1200, .T. ) ;
#117579 = CARTESIAN_POINT ( 'NONE',  ( 13.74999999999989875, 2.500000000000000000, 1.572243186433545548 ) ) ;
#117580 = CONICAL_SURFACE ( 'NONE', #75742, 0.1000000000000000056, 0.003490658503988666988 ) ;
#117581 = CARTESIAN_POINT ( 'NONE',  ( -12.89999999999999147, 2.500000000000000000, -4.922947341949750921 ) ) ;
#117582 = AXIS2_PLACEMENT_3D ( 'NONE', #43880, #92970, #3293 ) ;
#117583 = AXIS2_PLACEMENT_3D ( 'NONE', #11785, #2596, #121099 ) ;
#117584 = DIRECTION ( 'NONE',  ( 0.000000000000000000, 0.000000000000000000, 1.000000000000000000 ) ) ;
#117585 = CIRCLE ( 'NONE', #113413, 0.1000000000000000472 ) ;
#117586 = DIRECTION ( 'NONE',  ( 0.000000000000000000, 0.000000000000000000, -1.000000000000000000 ) ) ;
#117587 = AXIS2_PLACEMENT_3D ( 'NONE', #81004, #12878, #60093 ) ;
#117588 = ORIENTED_EDGE ( 'NONE', *, *, #30238, .T. ) ;
#117589 = DIRECTION ( 'NONE',  ( -0.000000000000000000, 1.000000000000000000, -0.000000000000000000 ) ) ;
#117590 = LINE ( 'NONE', #58705, #81399 ) ;
#117591 = DIRECTION ( 'NONE',  ( 0.000000000000000000, 0.000000000000000000, 1.000000000000000000 ) ) ;
#117592 = CARTESIAN_POINT ( 'NONE',  ( -10.80000000000000071, 2.500000000000000000, -2.276824562219559311E-15 ) ) ;
#117593 = DIRECTION ( 'NONE',  ( 0.000000000000000000, 0.000000000000000000, 1.000000000000000000 ) ) ;
#117594 = EDGE_LOOP ( 'NONE', ( #13391, #109390 ) ) ;
#117595 = CARTESIAN_POINT ( 'NONE',  ( 13.74999999999989875, 2.500000000000000000, 1.472243186433545459 ) ) ;
#117596 = FACE_OUTER_BOUND ( 'NONE', #4359, .T. ) ;
#117598 = ORIENTED_EDGE ( 'NONE', *, *, #71889, .T. ) ;
#117597 = DIRECTION ( 'NONE',  ( 0.000000000000000000, 1.000000000000000000, 0.000000000000000000 ) ) ;
#117599 = AXIS2_PLACEMENT_3D ( 'NONE', #79941, #119867, #32801 ) ;
#117600 = ORIENTED_EDGE ( 'NONE', *, *, #127421, .T. ) ;
#117601 = EDGE_CURVE ( 'NONE', #65687, #81044, #50646, .T. ) ;
#117602 = ORIENTED_EDGE ( 'NONE', *, *, #121051, .T. ) ;
#117603 = ORIENTED_EDGE ( 'NONE', *, *, #13656, .T. ) ;
#117604 = ORIENTED_EDGE ( 'NONE', *, *, #71344, .F. ) ;
#117605 = CARTESIAN_POINT ( 'NONE',  ( -6.450000000000019718, 12.50000000000000000, -1.818653347947326138 ) ) ;
#117606 = CIRCLE ( 'NONE', #75772, 0.06509327318403745899 ) ;
#117607 = DIRECTION ( 'NONE',  ( 0.000000000000000000, 1.000000000000000000, 0.000000000000000000 ) ) ;
#117608 = DIRECTION ( 'NONE',  ( 0.000000000000000000, 1.000000000000000000, 0.000000000000000000 ) ) ;
#117609 = DIRECTION ( 'NONE',  ( -0.000000000000000000, -1.000000000000000000, -0.000000000000000000 ) ) ;
#117610 = EDGE_CURVE ( 'NONE', #125433, #125134, #24191, .T. ) ;
#117612 = ORIENTED_EDGE ( 'NONE', *, *, #38790, .T. ) ;
#117611 = CONICAL_SURFACE ( 'NONE', #121751, 0.1000000000000002554, 0.003490658503988666988 ) ;
#117613 = CIRCLE ( 'NONE', #59072, 0.1000000000000000472 ) ;
#117614 = CIRCLE ( 'NONE', #119695, 0.09999999999999982514 ) ;
#117615 = DIRECTION ( 'NONE',  ( -0.000000000000000000, 1.000000000000000000, -0.000000000000000000 ) ) ;
#117617 = VERTEX_POINT ( 'NONE', #21183 ) ;
#117616 = VECTOR ( 'NONE', #101638, 1000.000000000000000 ) ;
#117618 = CARTESIAN_POINT ( 'NONE',  ( 21.24754738303276369, -0.7337760880902376437, -4.182111650399355618 ) ) ;
#117619 = CARTESIAN_POINT ( 'NONE',  ( -4.150000000000024336, 12.50000000000000000, -2.857883832488653741 ) ) ;
#117620 = VECTOR ( 'NONE', #88701, 1000.000000000000000 ) ;
#117621 = ADVANCED_FACE ( 'NONE', ( #1537 ), #38896, .T. ) ;
#117623 = CONICAL_SURFACE ( 'NONE', #90442, 0.1000000000000000472, 0.003490658503988666988 ) ;
#117622 = CARTESIAN_POINT ( 'NONE',  ( 21.24754738303277435, 0.7337760880902391980, 4.182111650399362723 ) ) ;
#117624 = FACE_OUTER_BOUND ( 'NONE', #46129, .T. ) ;
#117625 = CARTESIAN_POINT ( 'NONE',  ( -1.250000000000036193, 2.500000000000000000, 1.372243186433545370 ) ) ;
#117626 = ADVANCED_FACE ( 'NONE', ( #41502 ), #101037, .T. ) ;
#117627 = CIRCLE ( 'NONE', #42361, 0.1000000000000000472 ) ;
#117628 = VERTEX_POINT ( 'NONE', #61775 ) ;
#117629 = EDGE_LOOP ( 'NONE', ( #94150, #26574, #55146, #67156 ) ) ;
#117631 = ORIENTED_EDGE ( 'NONE', *, *, #110256, .T. ) ;
#117630 = ADVANCED_FACE ( 'NONE', ( #12007 ), #97343, .T. ) ;
#117632 = ORIENTED_EDGE ( 'NONE', *, *, #73089, .T. ) ;
#117633 = PLANE ( 'NONE',  #25197 ) ;
#117634 = CARTESIAN_POINT ( 'NONE',  ( 32.27737261616376685, 1.406459146825700390, 4.686451385765966648 ) ) ;
#117635 = DIRECTION ( 'NONE',  ( 0.000000000000000000, 0.000000000000000000, 1.000000000000000000 ) ) ;
#117636 = EDGE_CURVE ( 'NONE', #96595, #42755, #72869, .T. ) ;
#117637 = FACE_BOUND ( 'NONE', #91265, .T. ) ;
#117638 = DIRECTION ( 'NONE',  ( 0.000000000000000000, 1.000000000000000000, 0.000000000000000000 ) ) ;
#117639 = CARTESIAN_POINT ( 'NONE',  ( 186.8229166673494319, -4.445597072760122614, 7.699999999999998401 ) ) ;
#117640 = CARTESIAN_POINT ( 'NONE',  ( -2.500000000000031086, 2.500000000000000000, 3.637306695894644726 ) ) ;
#117641 = CARTESIAN_POINT ( 'NONE',  ( 6.849999999999930367, 2.500000000000000000, -6.148780366869526226 ) ) ;
#117642 = CARTESIAN_POINT ( 'NONE',  ( 184.3385416670080872, 6.551208109652274736, 3.782341765625001351 ) ) ;
#117643 = CARTESIAN_POINT ( 'NONE',  ( -3.350000000000028955, 12.50000000000000000, 7.253104124594885960 ) ) ;
#117644 = FACE_OUTER_BOUND ( 'NONE', #101968, .T. ) ;
#117645 = CIRCLE ( 'NONE', #61250, 0.06509327318403745899 ) ;
#117646 = VECTOR ( 'NONE', #11429, 1000.000000000000000 ) ;
#117647 = AXIS2_PLACEMENT_3D ( 'NONE', #83876, #124465, #15119 ) ;
#117648 = CARTESIAN_POINT ( 'NONE',  ( -7.700000000000014388, 2.500000000000000000, -0.3464101615137782364 ) ) ;
#117649 = VERTEX_POINT ( 'NONE', #40857 ) ;
#117650 = ORIENTED_EDGE ( 'NONE', *, *, #70820, .F. ) ;
#117651 = VERTEX_POINT ( 'NONE', #71572 ) ;
#117652 = ORIENTED_EDGE ( 'NONE', *, *, #8570, .T. ) ;
#117653 = CARTESIAN_POINT ( 'NONE',  ( -5.600000000000020073, 12.50000000000000000, 3.918623584224383727 ) ) ;
#117654 = FACE_BOUND ( 'NONE', #46436, .T. ) ;
#117655 = VECTOR ( 'NONE', #120413, 1000.000000000000000 ) ;
#117656 = AXIS2_PLACEMENT_3D ( 'NONE', #89586, #129539, #39865 ) ;
#117657 = DIRECTION ( 'NONE',  ( 0.000000000000000000, 0.000000000000000000, 1.000000000000000000 ) ) ;
#117658 = CONICAL_SURFACE ( 'NONE', #57039, 0.1000000000000000056, 0.003490658503988666988 ) ;
#117659 = ORIENTED_EDGE ( 'NONE', *, *, #37984, .T. ) ;
#117660 = FACE_OUTER_BOUND ( 'NONE', #38825, .T. ) ;
#117661 = DIRECTION ( 'NONE',  ( 0.000000000000000000, -0.9999939076577903929, 0.003490651415223739937 ) ) ;
#117662 = DIRECTION ( 'NONE',  ( 0.000000000000000000, 0.000000000000000000, -1.000000000000000000 ) ) ;
#117663 = ORIENTED_EDGE ( 'NONE', *, *, #76212, .F. ) ;
#117665 = CARTESIAN_POINT ( 'NONE',  ( 6.849999999999929479, 12.50000000000000000, -2.446380397790840266 ) ) ;
#117664 = AXIS2_PLACEMENT_3D ( 'NONE', #16218, #74528, #115724 ) ;
#117666 = DIRECTION ( 'NONE',  ( 0.000000000000000000, 1.000000000000000000, 0.000000000000000000 ) ) ;
#117667 = EDGE_CURVE ( 'NONE', #49122, #62242, #80634, .T. ) ;
#117668 = CONICAL_SURFACE ( 'NONE', #121805, 0.09999999999999999167, 0.003490658503988666988 ) ;
#117669 = AXIS2_PLACEMENT_3D ( 'NONE', #29391, #9736, #32472 ) ;
#117670 = EDGE_LOOP ( 'NONE', ( #34669, #21128, #5251, #33761 ) ) ;
#117671 = EDGE_CURVE ( 'NONE', #128960, #113533, #53238, .T. ) ;
#117672 = ORIENTED_EDGE ( 'NONE', *, *, #61887, .F. ) ;
#117673 = EDGE_CURVE ( 'NONE', #65564, #123810, #36722, .T. ) ;
#117674 = CARTESIAN_POINT ( 'NONE',  ( -2.300000000000033573, 2.500000000000000000, -4.083716857408426826 ) ) ;
#117675 = DIRECTION ( 'NONE',  ( 0.000000000000000000, 1.000000000000000000, 0.000000000000000000 ) ) ;
#117676 = VECTOR ( 'NONE', #21414, 1000.000000000000000 ) ;
#117677 = ADVANCED_FACE ( 'NONE', ( #82031 ), #47180, .T. ) ;
#117678 = EDGE_CURVE ( 'NONE', #52047, #76324, #22502, .T. ) ;
#117679 = CARTESIAN_POINT ( 'NONE',  ( 4.149999999999938183, 2.500000000000000000, 7.088010851410848190 ) ) ;
#117680 = DIRECTION ( 'NONE',  ( 0.000000000000000000, 0.000000000000000000, 1.000000000000000000 ) ) ;
#117681 = ORIENTED_EDGE ( 'NONE', *, *, #82364, .T. ) ;
#117683 = EDGE_CURVE ( 'NONE', #1124, #47988, #91081, .T. ) ;
#117682 = DIRECTION ( 'NONE',  ( 0.000000000000000000, 1.000000000000000000, 0.000000000000000000 ) ) ;
#117684 = VERTEX_POINT ( 'NONE', #3479 ) ;
#117685 = ORIENTED_EDGE ( 'NONE', *, *, #117380, .T. ) ;
#117686 = CARTESIAN_POINT ( 'NONE',  ( 3.749999999999940492, 2.500000000000000000, 5.802370205355744659 ) ) ;
#117687 = ORIENTED_EDGE ( 'NONE', *, *, #98326, .T. ) ;
#117688 = CARTESIAN_POINT ( 'NONE',  ( -3.350000000000032507, 12.50000000000000000, -6.495190528383302464 ) ) ;
#117689 = FACE_BOUND ( 'NONE', #17852, .T. ) ;
#117690 = EDGE_CURVE ( 'NONE', #52824, #98546, #34674, .T. ) ;
#117691 = ADVANCED_FACE ( 'NONE', ( #126484 ), #53875, .T. ) ;
#117692 = VERTEX_POINT ( 'NONE', #44703 ) ;
#117693 = CARTESIAN_POINT ( 'NONE',  ( 2.899999999999946620, 12.50000000000000000, -3.572213422710612374 ) ) ;
#117694 = ORIENTED_EDGE ( 'NONE', *, *, #113001, .F. ) ;
#117695 = CARTESIAN_POINT ( 'NONE',  ( -10.85000000000000142, 2.500000000000000000, 6.495190528383297135 ) ) ;
#117696 = DIRECTION ( 'NONE',  ( -0.000000000000000000, -1.000000000000000000, -0.000000000000000000 ) ) ;
#117697 = DIRECTION ( 'NONE',  ( 0.000000000000000000, 1.000000000000000000, 0.000000000000000000 ) ) ;
#117698 = CIRCLE ( 'NONE', #109406, 0.06509327318403743123 ) ;
#117699 = CARTESIAN_POINT ( 'NONE',  ( 9.599999999999917932, 2.500000000000000000, -0.7928203230275542301 ) ) ;
#117700 = CARTESIAN_POINT ( 'NONE',  ( 0.6499999999999566125, 12.50000000000000000, -6.083687093685488989 ) ) ;
#117701 = ORIENTED_EDGE ( 'NONE', *, *, #52525, .F. ) ;
#117702 = EDGE_LOOP ( 'NONE', ( #65050, #80908, #2445 ) ) ;
#117703 = DIRECTION ( 'NONE',  ( 0.000000000000000000, 0.000000000000000000, 1.000000000000000000 ) ) ;
#117704 = AXIS2_PLACEMENT_3D ( 'NONE', #115531, #35706, #43608 ) ;
#117705 = AXIS2_PLACEMENT_3D ( 'NONE', #72620, #31411, #32064 ) ;
#117706 = CARTESIAN_POINT ( 'NONE',  ( 0.5999999999999555689, 2.500000000000000000, 4.576537180435972019 ) ) ;
#117707 = CONICAL_SURFACE ( 'NONE', #11104, 0.1000000000000002554, 0.003490658503988666988 ) ;
#117709 = CARTESIAN_POINT ( 'NONE',  ( 6.049999999999930544, 2.500000000000000000, 2.611473670974873151 ) ) ;
#117708 = CONICAL_SURFACE ( 'NONE', #98849, 0.1000000000000002554, 0.003490658503988666988 ) ;
#117711 = VERTEX_POINT ( 'NONE', #4744 ) ;
#117710 = ORIENTED_EDGE ( 'NONE', *, *, #90739, .T. ) ;
#117712 = ORIENTED_EDGE ( 'NONE', *, *, #36885, .T. ) ;
#117713 = CARTESIAN_POINT ( 'NONE',  ( 7.499999999999925393, 2.500000000000000000, 5.022947341949748790 ) ) ;
#117714 = CARTESIAN_POINT ( 'NONE',  ( 187.2812500006828031, 0.000000000000000000, 7.700000000000000178 ) ) ;
#117715 = AXIS2_PLACEMENT_3D ( 'NONE', #58217, #107937, #68010 ) ;
#117716 = CIRCLE ( 'NONE', #2710, 0.06509327318403745899 ) ;
#117717 = AXIS2_PLACEMENT_3D ( 'NONE', #2185, #40863, #21857 ) ;
#117718 = APPLICATION_PROTOCOL_DEFINITION ( 'draft international standard', 'automotive_design', 1998, #17924 ) ;
#117719 = DIRECTION ( 'NONE',  ( -0.000000000000000000, -1.000000000000000000, -0.000000000000000000 ) ) ;
#117720 = DIRECTION ( 'NONE',  ( 0.000000000000000000, -0.000000000000000000, 1.000000000000000000 ) ) ;
#117721 = CARTESIAN_POINT ( 'NONE',  ( 6.849999999999929479, 12.50000000000000000, 6.841600689897072485 ) ) ;
#117722 = CONICAL_SURFACE ( 'NONE', #17372, 0.1000000000000000472, 0.003490658503988666988 ) ;
#117723 = CARTESIAN_POINT ( 'NONE',  ( 15.19999999999989093, 12.50000000000000000, 0.3464101615137735735 ) ) ;
#117724 = CARTESIAN_POINT ( 'NONE',  ( 5.849999999999933920, 2.500000000000000000, 6.395190528383296602 ) ) ;
#117725 = AXIS2_PLACEMENT_3D ( 'NONE', #114687, #75406, #23755 ) ;
#117726 = CARTESIAN_POINT ( 'NONE',  ( 184.5312500006828031, 9.429780353434619030E-16, -7.700000000000000178 ) ) ;
#117727 = AXIS2_PLACEMENT_3D ( 'NONE', #89120, #49220, #119866 ) ;
#117728 = EDGE_LOOP ( 'NONE', ( #29365, #46724 ) ) ;
#117729 = ORIENTED_EDGE ( 'NONE', *, *, #94997, .F. ) ;
#117730 = DIRECTION ( 'NONE',  ( 0.000000000000000000, 1.000000000000000000, 0.000000000000000000 ) ) ;
#117731 = DIRECTION ( 'NONE',  ( 0.000000000000000000, -0.000000000000000000, 1.000000000000000000 ) ) ;
#117732 = VERTEX_POINT ( 'NONE', #44052 ) ;
#117733 = VERTEX_POINT ( 'NONE', #125813 ) ;
#117734 = CARTESIAN_POINT ( 'NONE',  ( 186.9427083336747160, -6.551208109652278289, 3.782341765624995134 ) ) ;
#117735 = DIRECTION ( 'NONE',  ( -0.000000000000000000, 1.000000000000000000, -0.000000000000000000 ) ) ;
#117736 = DIRECTION ( 'NONE',  ( 0.000000000000000000, 0.000000000000000000, 1.000000000000000000 ) ) ;
#117737 = DIRECTION ( 'NONE',  ( 0.000000000000000000, 0.000000000000000000, -1.000000000000000000 ) ) ;
#117738 = EDGE_CURVE ( 'NONE', #54447, #22835, #112019, .T. ) ;
#117739 = DIRECTION ( 'NONE',  ( -4.274815082592931898E-19, -0.9999939076577903929, -0.003490651415223739937 ) ) ;
#117740 = DIRECTION ( 'NONE',  ( 0.000000000000000000, 1.000000000000000000, 0.000000000000000000 ) ) ;
#117741 = DIRECTION ( 'NONE',  ( -0.000000000000000000, 1.000000000000000000, -0.000000000000000000 ) ) ;
#117742 = ORIENTED_EDGE ( 'NONE', *, *, #105601, .T. ) ;
#117743 = CARTESIAN_POINT ( 'NONE',  ( 8.549999999999920774, 12.50000000000000000, -2.511473670974877948 ) ) ;
#117744 = VECTOR ( 'NONE', #86228, 1000.000000000000000 ) ;
#117746 = CIRCLE ( 'NONE', #6924, 0.06509327318403745899 ) ;
#117745 = DIRECTION ( 'NONE',  ( 0.000000000000000000, 0.000000000000000000, 1.000000000000000000 ) ) ;
#117747 = AXIS2_PLACEMENT_3D ( 'NONE', #86077, #114906, #125391 ) ;
#117748 = EDGE_LOOP ( 'NONE', ( #14414, #20151, #50074, #40126 ) ) ;
#117749 = EDGE_LOOP ( 'NONE', ( #103885, #88191 ) ) ;
#117750 = ORIENTED_EDGE ( 'NONE', *, *, #86612, .F. ) ;
#117751 = VERTEX_POINT ( 'NONE', #84623 ) ;
#117752 = VECTOR ( 'NONE', #107200, 1000.000000000000000 ) ;
#117753 = DIRECTION ( 'NONE',  ( -0.000000000000000000, -1.000000000000000000, -0.000000000000000000 ) ) ;
#117754 = DIRECTION ( 'NONE',  ( -4.274815082592931898E-19, -0.9999939076577903929, -0.003490651415223739937 ) ) ;
#117755 = CIRCLE ( 'NONE', #9008, 0.1000000000000002554 ) ;
#117756 = CIRCLE ( 'NONE', #23695, 0.1000000000000000472 ) ;
#117757 = ORIENTED_EDGE ( 'NONE', *, *, #111623, .T. ) ;
#117758 = DIRECTION ( 'NONE',  ( 0.000000000000000000, 0.000000000000000000, -1.000000000000000000 ) ) ;
#117759 = CARTESIAN_POINT ( 'NONE',  ( 17.50000000000000000, 0.9166666666666674068, -9.999999999999998224 ) ) ;
#117760 = CARTESIAN_POINT ( 'NONE',  ( -2.050000000000033129, 2.500000000000000000, 6.495190528383297135 ) ) ;
#117762 = ORIENTED_EDGE ( 'NONE', *, *, #96058, .T. ) ;
#117761 = DIRECTION ( 'NONE',  ( -0.000000000000000000, -1.000000000000000000, -0.000000000000000000 ) ) ;
#117763 = DIRECTION ( 'NONE',  ( 0.000000000000000000, 1.000000000000000000, 0.000000000000000000 ) ) ;
#117764 = AXIS2_PLACEMENT_3D ( 'NONE', #90315, #123494, #33213 ) ;
#117765 = FACE_OUTER_BOUND ( 'NONE', #79446, .T. ) ;
#117766 = VERTEX_POINT ( 'NONE', #104261 ) ;
#117767 = AXIS2_PLACEMENT_3D ( 'NONE', #37607, #129226, #68337 ) ;
#117768 = AXIS2_PLACEMENT_3D ( 'NONE', #94701, #5023, #114975 ) ;
#117769 = EDGE_LOOP ( 'NONE', ( #13877, #14030, #51077, #2288 ) ) ;
#117770 = EDGE_LOOP ( 'NONE', ( #61556, #43038 ) ) ;
#117771 = DIRECTION ( 'NONE',  ( 0.000000000000000000, 0.000000000000000000, -1.000000000000000000 ) ) ;
#117772 = AXIS2_PLACEMENT_3D ( 'NONE', #120753, #112873, #61848 ) ;
#117773 = CARTESIAN_POINT ( 'NONE',  ( 179.5000000000000000, 0.000000000000000000, 6.000000000000000000 ) ) ;
#117774 = VECTOR ( 'NONE', #106247, 1000.000000000000000 ) ;
#117775 = EDGE_CURVE ( 'NONE', #79983, #83925, #13705, .T. ) ;
#117776 = EDGE_LOOP ( 'NONE', ( #55755, #120168, #112296, #46936 ) ) ;
#117777 = DIRECTION ( 'NONE',  ( 0.000000000000000000, 1.000000000000000000, 0.000000000000000000 ) ) ;
#117778 = CARTESIAN_POINT ( 'NONE',  ( 108.0000000000000142, 8.500000000000000000, -2.749999999999997335 ) ) ;
#117779 = EDGE_CURVE ( 'NONE', #57084, #25471, #103624, .T. ) ;
#117780 = DIRECTION ( 'NONE',  ( -0.000000000000000000, 1.000000000000000000, -0.000000000000000000 ) ) ;
#117781 = DIRECTION ( 'NONE',  ( 0.000000000000000000, 0.000000000000000000, 1.000000000000000000 ) ) ;
#117782 = EDGE_CURVE ( 'NONE', #102213, #104601, #3261, .T. ) ;
#117783 = EDGE_LOOP ( 'NONE', ( #11116, #52424, #103939, #120446 ) ) ;
#117784 = DIRECTION ( 'NONE',  ( 0.000000000000000000, 1.000000000000000000, 0.000000000000000000 ) ) ;
#117785 = EDGE_LOOP ( 'NONE', ( #80960, #32148 ) ) ;
#117786 = ADVANCED_FACE ( 'NONE', ( #85890 ), #76733, .T. ) ;
#117788 = EDGE_LOOP ( 'NONE', ( #67494, #101633, #88603, #35869 ) ) ;
#117787 = EDGE_CURVE ( 'NONE', #113497, #125598, #24411, .T. ) ;
#117790 = VECTOR ( 'NONE', #98102, 1000.000000000000000 ) ;
#117789 = CARTESIAN_POINT ( 'NONE',  ( -7.900000000000014566, 2.500000000000000000, -0.6928203230275541413 ) ) ;
#117791 = AXIS2_PLACEMENT_3D ( 'NONE', #105315, #75205, #104648 ) ;
#117792 = EDGE_CURVE ( 'NONE', #41830, #107284, #63700, .T. ) ;
#117794 = EDGE_CURVE ( 'NONE', #90718, #89885, #30471, .T. ) ;
#117793 = CARTESIAN_POINT ( 'NONE',  ( 2.049999999999950084, 12.50000000000000000, -6.495190528383302464 ) ) ;
#117795 = EDGE_CURVE ( 'NONE', #35451, #107061, #122398, .T. ) ;
#117796 = FACE_BOUND ( 'NONE', #31384, .T. ) ;
#117797 = DIRECTION ( 'NONE',  ( -0.000000000000000000, -1.000000000000000000, -0.000000000000000000 ) ) ;
#117798 = CARTESIAN_POINT ( 'NONE',  ( 0.4499999999999569344, 2.500000000000000000, 2.265063509461097357 ) ) ;
#117799 = CARTESIAN_POINT ( 'NONE',  ( 7.699999999999923794, 2.500000000000000000, -3.983716857408426293 ) ) ;
#117800 = AXIS2_PLACEMENT_3D ( 'NONE', #101724, #82067, #108934 ) ;
#117801 = AXIS2_PLACEMENT_3D ( 'NONE', #43103, #83015, #33276 ) ;
#117802 = CONICAL_SURFACE ( 'NONE', #126144, 0.1000000000000002554, 0.003490658503988666988 ) ;
#117803 = ORIENTED_EDGE ( 'NONE', *, *, #97582, .T. ) ;
#117804 = DIRECTION ( 'NONE',  ( -0.000000000000000000, 1.000000000000000000, 0.000000000000000000 ) ) ;
#117805 = LINE ( 'NONE', #129608, #51062 ) ;
#117806 = ADVANCED_FACE ( 'NONE', ( #114717 ), #35535, .T. ) ;
#117807 = DIRECTION ( 'NONE',  ( 0.000000000000000000, 0.000000000000000000, -1.000000000000000000 ) ) ;
#117808 = CARTESIAN_POINT ( 'NONE',  ( 13.54999999999989946, 2.500000000000000000, 2.511473670974873507 ) ) ;
#117809 = ORIENTED_EDGE ( 'NONE', *, *, #53279, .F. ) ;
#117810 = CARTESIAN_POINT ( 'NONE',  ( 14.99999999999992895, 2.500000000000000000, -0.1000000000000022815 ) ) ;
#117811 = AXIS2_PLACEMENT_3D ( 'NONE', #121920, #72190, #123217 ) ;
#117812 = AXIS2_PLACEMENT_3D ( 'NONE', #1595, #13988, #81467 ) ;
#117813 = CARTESIAN_POINT ( 'NONE',  ( -14.59999999999998366, 2.500000000000000000, 0.6928203230275518099 ) ) ;
#117814 = EDGE_LOOP ( 'NONE', ( #27882, #101387, #7314, #64192 ) ) ;
#117815 = ORIENTED_EDGE ( 'NONE', *, *, #39833, .T. ) ;
#117816 = AXIS2_PLACEMENT_3D ( 'NONE', #51767, #10529, #21002 ) ;
#117817 = DIRECTION ( 'NONE',  ( 0.000000000000000000, 1.000000000000000000, 0.000000000000000000 ) ) ;
#117818 = DIRECTION ( 'NONE',  ( 0.000000000000000000, 1.000000000000000000, 0.000000000000000000 ) ) ;
#117819 = FACE_BOUND ( 'NONE', #60997, .T. ) ;
#117820 = CARTESIAN_POINT ( 'NONE',  ( 4.999999999999969802, 2.500000000000000000, 4.330127018922196314 ) ) ;
#117821 = ORIENTED_EDGE ( 'NONE', *, *, #62769, .T. ) ;
#117822 = LINE ( 'NONE', #127036, #52860 ) ;
#117823 = EDGE_LOOP ( 'NONE', ( #102879, #62151 ) ) ;
#117824 =( BOUNDED_CURVE ( )  B_SPLINE_CURVE ( 2, ( #123835, #13235, #102289, #23080, #14524, #112111, #63001 ),
 .UNSPECIFIED., .F., .F. ) 
 B_SPLINE_CURVE_WITH_KNOTS ( ( 3, 2, 2, 3 ),
 ( 0.5000000000000004441, 0.5238095238095242800, 0.5476190476190482270, 0.5714285714285719520 ),
 .UNSPECIFIED. ) 
 CURVE ( )  GEOMETRIC_REPRESENTATION_ITEM ( )  RATIONAL_B_SPLINE_CURVE ( ( 0.9999999999999974465, 0.8660254037844412611, 1.000000000000000000, 0.8660254037844387076, 1.000000000000000000, 0.8660254037844355990, 1.000000000000003109 ) ) 
 REPRESENTATION_ITEM ( '' )  );
#117825 = ORIENTED_EDGE ( 'NONE', *, *, #89886, .F. ) ;
#117826 = DIRECTION ( 'NONE',  ( 0.000000000000000000, 0.000000000000000000, 1.000000000000000000 ) ) ;
#117827 = CARTESIAN_POINT ( 'NONE',  ( 186.0000000000000000, 0.000000000000000000, 7.700000000000000178 ) ) ;
#117828 = EDGE_LOOP ( 'NONE', ( #49415, #26466, #94623, #36723 ) ) ;
#117829 = FACE_OUTER_BOUND ( 'NONE', #9294, .T. ) ;
#117830 = DIRECTION ( 'NONE',  ( 0.000000000000000000, 0.000000000000000000, 1.000000000000000000 ) ) ;
#117831 = EDGE_CURVE ( 'NONE', #9793, #45052, #65942, .T. ) ;
#117832 = DIRECTION ( 'NONE',  ( 0.000000000000000000, 0.000000000000000000, -1.000000000000000000 ) ) ;
#117833 = DIRECTION ( 'NONE',  ( 0.000000000000000000, -0.000000000000000000, 1.000000000000000000 ) ) ;
#117834 = CIRCLE ( 'NONE', #61144, 0.06509327318403745899 ) ;
#117835 = EDGE_CURVE ( 'NONE', #54631, #51919, #70165, .T. ) ;
#117836 = VECTOR ( 'NONE', #22405, 1000.000000000000000 ) ;
#117837 = ORIENTED_EDGE ( 'NONE', *, *, #31062, .F. ) ;
#117838 = EDGE_CURVE ( 'NONE', #76450, #26951, #9522, .T. ) ;
#117839 = DIRECTION ( 'NONE',  ( 0.000000000000000000, 1.000000000000000000, 0.000000000000000000 ) ) ;
#117840 = LINE ( 'NONE', #127049, #112408 ) ;
#117841 = DIRECTION ( 'NONE',  ( 0.000000000000000000, 0.000000000000000000, 1.000000000000000000 ) ) ;
#117842 = FACE_OUTER_BOUND ( 'NONE', #49789, .T. ) ;
#117843 = ORIENTED_EDGE ( 'NONE', *, *, #17486, .T. ) ;
#117844 = DIRECTION ( 'NONE',  ( 0.000000000000000000, 1.000000000000000000, 0.000000000000000000 ) ) ;
#117845 = VERTEX_POINT ( 'NONE', #4108 ) ;
#117846 = ADVANCED_FACE ( 'NONE', ( #76091 ), #123884, .T. ) ;
#117847 = CONICAL_SURFACE ( 'NONE', #19672, 0.09999999999999982514, 0.003490658503988666988 ) ;
#117848 = CARTESIAN_POINT ( 'NONE',  ( 0.3999999999999563904, 2.500000000000000000, 3.637306695894644726 ) ) ;
#117849 = VECTOR ( 'NONE', #8278, 1000.000000000000000 ) ;
#117851 = VERTEX_POINT ( 'NONE', #49871 ) ;
#117850 = EDGE_CURVE ( 'NONE', #32199, #11699, #86872, .T. ) ;
#117853 = FACE_OUTER_BOUND ( 'NONE', #71031, .T. ) ;
#117852 = CONICAL_SURFACE ( 'NONE', #9202, 0.09999999999999982514, 0.003490658503988666988 ) ;
#117854 = DIRECTION ( 'NONE',  ( 0.000000000000000000, -0.000000000000000000, 1.000000000000000000 ) ) ;
#117855 = EDGE_CURVE ( 'NONE', #57879, #62826, #45124, .T. ) ;
#117856 = AXIS2_PLACEMENT_3D ( 'NONE', #36997, #17318, #17986 ) ;
#117857 = DIRECTION ( 'NONE',  ( -0.000000000000000000, 1.000000000000000000, -0.000000000000000000 ) ) ;
#117858 = ADVANCED_FACE ( 'NONE', ( #67530 ), #19075, .T. ) ;
#117859 = FACE_OUTER_BOUND ( 'NONE', #75326, .T. ) ;
#117860 = VERTEX_POINT ( 'NONE', #106818 ) ;
#117861 = CARTESIAN_POINT ( 'NONE',  ( 6.249999999999932498, 12.50000000000000000, -2.857883832488653741 ) ) ;
#117862 = DIRECTION ( 'NONE',  ( 0.000000000000000000, 1.000000000000000000, 0.000000000000000000 ) ) ;
#117863 = CARTESIAN_POINT ( 'NONE',  ( -5.000000000000023093, 2.500000000000000000, 4.922947341949748257 ) ) ;
#117864 = CARTESIAN_POINT ( 'NONE',  ( 185.3177083336747160, 4.367472073101515306, 7.564683531250000925 ) ) ;
#117865 = LINE ( 'NONE', #97591, #94610 ) ;
#117866 = AXIS2_PLACEMENT_3D ( 'NONE', #17394, #46887, #126070 ) ;
#117868 = EDGE_CURVE ( 'NONE', #3164, #2356, #63989, .T. ) ;
#117867 = DIRECTION ( 'NONE',  ( -1.000000000000000000, -0.000000000000000000, -0.000000000000000000 ) ) ;
#117869 = ORIENTED_EDGE ( 'NONE', *, *, #89790, .T. ) ;
#117870 = ORIENTED_EDGE ( 'NONE', *, *, #5613, .F. ) ;
#117871 = DIRECTION ( 'NONE',  ( 0.000000000000000000, -0.9999939076577903929, 0.003490651415223739937 ) ) ;
#117873 = VERTEX_POINT ( 'NONE', #119231 ) ;
#117872 = CIRCLE ( 'NONE', #82398, 0.06509327318403745899 ) ;
#117874 = CIRCLE ( 'NONE', #105370, 0.06509327318403745899 ) ;
#117875 = CIRCLE ( 'NONE', #11267, 0.06509327318403745899 ) ;
#117876 = CARTESIAN_POINT ( 'NONE',  ( -2.500000000000030642, 2.500000000000000000, -0.6928203230275541413 ) ) ;
#117878 = ORIENTED_EDGE ( 'NONE', *, *, #51059, .F. ) ;
#117877 = VERTEX_POINT ( 'NONE', #17798 ) ;
#117879 = VERTEX_POINT ( 'NONE', #98950 ) ;
#117880 = CIRCLE ( 'NONE', #13417, 0.1000000000000002554 ) ;
#117881 = DIRECTION ( 'NONE',  ( 0.000000000000000000, 1.000000000000000000, 0.000000000000000000 ) ) ;
#117882 = AXIS2_PLACEMENT_3D ( 'NONE', #3689, #61981, #82909 ) ;
#117883 = DIRECTION ( 'NONE',  ( -0.000000000000000000, -1.000000000000000000, -0.000000000000000000 ) ) ;
#117884 = CARTESIAN_POINT ( 'NONE',  ( -13.34999999999999076, 12.50000000000000000, -2.857883832488651521 ) ) ;
#117885 = DIRECTION ( 'NONE',  ( -0.000000000000000000, 1.000000000000000000, -0.000000000000000000 ) ) ;
#117886 = CARTESIAN_POINT ( 'NONE',  ( 6.249999999999968914, 2.500000000000000000, -6.595190528383302109 ) ) ;
#117887 = CARTESIAN_POINT ( 'NONE',  ( 6.449999999999931788, 12.50000000000000000, -6.148780366869526226 ) ) ;
#117888 = DIRECTION ( 'NONE',  ( -4.274815082592931898E-19, -0.9999939076577903929, -0.003490651415223739937 ) ) ;
#117889 = EDGE_CURVE ( 'NONE', #119822, #126385, #89034, .T. ) ;
#117890 = DIRECTION ( 'NONE',  ( -0.000000000000000000, -1.000000000000000000, -0.000000000000000000 ) ) ;
#117891 = ORIENTED_EDGE ( 'NONE', *, *, #119037, .F. ) ;
#117892 = ORIENTED_EDGE ( 'NONE', *, *, #126105, .F. ) ;
#117893 = ORIENTED_EDGE ( 'NONE', *, *, #52619, .T. ) ;
#117894 = ORIENTED_EDGE ( 'NONE', *, *, #103334, .F. ) ;
#117895 = AXIS2_PLACEMENT_3D ( 'NONE', #110824, #92480, #61094 ) ;
#117896 = DIRECTION ( 'NONE',  ( 0.000000000000000000, 1.000000000000000000, 0.000000000000000000 ) ) ;
#117897 = AXIS2_PLACEMENT_3D ( 'NONE', #54791, #35812, #84908 ) ;
#117898 = AXIS2_PLACEMENT_3D ( 'NONE', #90825, #31914, #90154 ) ;
#117899 = ORIENTED_EDGE ( 'NONE', *, *, #66827, .F. ) ;
#117900 = EDGE_LOOP ( 'NONE', ( #71854, #106480, #31217, #17228 ) ) ;
#117902 = CARTESIAN_POINT ( 'NONE',  ( -13.54999999999999005, 2.500000000000000000, 2.511473670974877503 ) ) ;
#117901 = AXIS2_PLACEMENT_3D ( 'NONE', #44740, #125223, #93830 ) ;
#117903 = AXIS2_PLACEMENT_3D ( 'NONE', #101841, #60009, #90067 ) ;
#117904 = CARTESIAN_POINT ( 'NONE',  ( -8.750000000000010658, 2.500000000000000000, 2.857883832488649301 ) ) ;
#117905 = ADVANCED_FACE ( 'NONE', ( #47283 ), #124631, .T. ) ;
#117907 = DIRECTION ( 'NONE',  ( 0.000000000000000000, 1.000000000000000000, 0.000000000000000000 ) ) ;
#117906 = AXIS2_PLACEMENT_3D ( 'NONE', #8789, #79491, #97821 ) ;
#117908 = CARTESIAN_POINT ( 'NONE',  ( 3.749999999999978684, 12.50000000000000000, -6.495190528383302464 ) ) ;
#117909 = CONICAL_SURFACE ( 'NONE', #82335, 0.1000000000000002554, 0.003490658503988666988 ) ;
#117910 = CARTESIAN_POINT ( 'NONE',  ( 6.449999999999930012, 12.50000000000000000, -1.818653347947326138 ) ) ;
#117911 = ORIENTED_EDGE ( 'NONE', *, *, #84455, .T. ) ;
#117912 = FACE_OUTER_BOUND ( 'NONE', #49016, .T. ) ;
#117913 = CONICAL_SURFACE ( 'NONE', #42644, 0.1000000000000002554, 0.003490658503988666988 ) ;
#117915 = ORIENTED_EDGE ( 'NONE', *, *, #37576, .F. ) ;
#117914 = CIRCLE ( 'NONE', #63555, 0.1000000000000000472 ) ;
#117916 = DIRECTION ( 'NONE',  ( 0.000000000000000000, 0.000000000000000000, -1.000000000000000000 ) ) ;
#117917 = AXIS2_PLACEMENT_3D ( 'NONE', #109314, #19657, #27515 ) ;
#117918 = ORIENTED_EDGE ( 'NONE', *, *, #122287, .T. ) ;
#117919 = DIRECTION ( 'NONE',  ( -0.000000000000000000, -1.000000000000000000, -0.000000000000000000 ) ) ;
#117920 = VERTEX_POINT ( 'NONE', #128436 ) ;
#117921 = CIRCLE ( 'NONE', #860, 0.06509327318403745899 ) ;
#117922 = EDGE_CURVE ( 'NONE', #63043, #107053, #7536, .T. ) ;
#117923 = ORIENTED_EDGE ( 'NONE', *, *, #26089, .F. ) ;
#117924 = DIRECTION ( 'NONE',  ( -0.000000000000000000, 1.000000000000000000, -0.000000000000000000 ) ) ;
#117925 = CARTESIAN_POINT ( 'NONE',  ( 87.50000000000001421, -3.975350567648449740, -6.360562287258772152 ) ) ;
#117926 = DIRECTION ( 'NONE',  ( 0.000000000000000000, 1.000000000000000000, 0.000000000000000000 ) ) ;
#117927 = FACE_OUTER_BOUND ( 'NONE', #64630, .T. ) ;
#117928 = AXIS2_PLACEMENT_3D ( 'NONE', #110805, #72194, #32284 ) ;
#117929 = CARTESIAN_POINT ( 'NONE',  ( -1.450000000000036371, 2.500000000000000000, 6.841600689897072485 ) ) ;
#117930 = ORIENTED_EDGE ( 'NONE', *, *, #102303, .T. ) ;
#117931 = DIRECTION ( 'NONE',  ( -0.000000000000000000, 1.000000000000000000, -0.000000000000000000 ) ) ;
#117932 = CARTESIAN_POINT ( 'NONE',  ( 179.5000000000000000, -0.6250000000000028866, -7.634788798650553154 ) ) ;
#117933 = CARTESIAN_POINT ( 'NONE',  ( -9.150000000000009237, 2.500000000000000000, -7.288010851410849256 ) ) ;
#117934 = DIRECTION ( 'NONE',  ( 0.000000000000000000, 1.000000000000000000, 0.000000000000000000 ) ) ;
#117935 = AXIS2_PLACEMENT_3D ( 'NONE', #126133, #86186, #48221 ) ;
#117936 = CARTESIAN_POINT ( 'NONE',  ( 10.39999999999991154, 2.500000000000000000, 3.637306695894644726 ) ) ;
#117937 = VERTEX_POINT ( 'NONE', #26997 ) ;
#117938 = VERTEX_POINT ( 'NONE', #7979 ) ;
#117939 = DIRECTION ( 'NONE',  ( 0.000000000000000000, 0.000000000000000000, -1.000000000000000000 ) ) ;
#117940 = ORIENTED_EDGE ( 'NONE', *, *, #762, .F. ) ;
#117941 = AXIS2_PLACEMENT_3D ( 'NONE', #62010, #31900, #84201 ) ;
#117942 = DIRECTION ( 'NONE',  ( -0.000000000000000000, -1.000000000000000000, -0.000000000000000000 ) ) ;
#117943 = CARTESIAN_POINT ( 'NONE',  ( -14.19999999999998685, 12.50000000000000000, -1.084202172485504434E-16 ) ) ;
#117944 = ADVANCED_FACE ( 'NONE', ( #66898 ), #116201, .T. ) ;
#117945 = VERTEX_POINT ( 'NONE', #7332 ) ;
#117946 = CARTESIAN_POINT ( 'NONE',  ( 186.7500000000000000, 9.429780353434619030E-16, -7.700000000000000178 ) ) ;
#117947 = CARTESIAN_POINT ( 'NONE',  ( -6.250000000000015987, 2.500000000000000000, 5.802370205355744659 ) ) ;
#117948 = CARTESIAN_POINT ( 'NONE',  ( -3.550000000000028244, 12.50000000000000000, -1.818653347947326138 ) ) ;
#117949 = DIRECTION ( 'NONE',  ( 0.000000000000000000, 0.000000000000000000, 1.000000000000000000 ) ) ;
#117950 = EDGE_LOOP ( 'NONE', ( #95007, #99718, #33617, #114496 ) ) ;
#117951 = EDGE_CURVE ( 'NONE', #66296, #6219, #86967, .T. ) ;
#117952 = AXIS2_PLACEMENT_3D ( 'NONE', #100422, #10721, #50672 ) ;
#117953 = DIRECTION ( 'NONE',  ( 0.000000000000000000, 1.000000000000000000, 0.000000000000000000 ) ) ;
#117954 = CARTESIAN_POINT ( 'NONE',  ( -13.09999999999999076, 2.500000000000000000, 3.983716857408420964 ) ) ;
#117955 = VERTEX_POINT ( 'NONE', #57082 ) ;
#117956 = EDGE_CURVE ( 'NONE', #79243, #109920, #18004, .T. ) ;
#117957 = ADVANCED_FACE ( 'NONE', ( #117266 ), #91182, .T. ) ;
#117958 = EDGE_CURVE ( 'NONE', #20142, #80050, #49350, .T. ) ;
#117960 = EDGE_CURVE ( 'NONE', #64674, #10550, #49228, .T. ) ;
#117959 = DIRECTION ( 'NONE',  ( 0.000000000000000000, 0.000000000000000000, 1.000000000000000000 ) ) ;
#117961 = FACE_OUTER_BOUND ( 'NONE', #60875, .T. ) ;
#117962 = DIRECTION ( 'NONE',  ( 0.000000000000000000, 0.000000000000000000, 1.000000000000000000 ) ) ;
#117963 = ORIENTED_EDGE ( 'NONE', *, *, #116802, .T. ) ;
#117964 = CIRCLE ( 'NONE', #17617, 0.09999999999999982514 ) ;
#117965 = VECTOR ( 'NONE', #91109, 1000.000000000000000 ) ;
#117966 = DIRECTION ( 'NONE',  ( 0.000000000000000000, -0.9999939076577903929, 0.003490651415223739937 ) ) ;
#117968 = ORIENTED_EDGE ( 'NONE', *, *, #104968, .F. ) ;
#117967 = CIRCLE ( 'NONE', #51104, 0.09999999999999982514 ) ;
#117969 = FACE_OUTER_BOUND ( 'NONE', #46734, .T. ) ;
#117970 = CARTESIAN_POINT ( 'NONE',  ( -4.293440603042597559E-14, 2.500000000000000000, 5.122947341949749323 ) ) ;
#117971 = EDGE_CURVE ( 'NONE', #55580, #88783, #8609, .T. ) ;
#117972 = DIRECTION ( 'NONE',  ( 0.000000000000000000, 0.000000000000000000, -1.000000000000000000 ) ) ;
#117973 = AXIS2_PLACEMENT_3D ( 'NONE', #29151, #58603, #117474 ) ;
#117974 = ORIENTED_EDGE ( 'NONE', *, *, #19389, .T. ) ;
#117975 = EDGE_CURVE ( 'NONE', #10181, #87020, #72320, .T. ) ;
#117977 = EDGE_CURVE ( 'NONE', #66966, #81045, #107894, .T. ) ;
#117976 = CARTESIAN_POINT ( 'NONE',  ( -2.100000000000034284, 2.500000000000000000, -4.230127018922201998 ) ) ;
#117978 = FACE_OUTER_BOUND ( 'NONE', #64758, .T. ) ;
#117979 = ORIENTED_EDGE ( 'NONE', *, *, #11329, .T. ) ;
#117980 = CARTESIAN_POINT ( 'NONE',  ( -0.4000000000000404898, 2.500000000000000000, 5.022947341949748790 ) ) ;
#117981 = VERTEX_POINT ( 'NONE', #69475 ) ;
#117982 = DIRECTION ( 'NONE',  ( 0.000000000000000000, 0.000000000000000000, 1.000000000000000000 ) ) ;
#117983 = VECTOR ( 'NONE', #30848, 1000.000000000000000 ) ;
#117984 = EDGE_LOOP ( 'NONE', ( #106435, #87450, #112136, #116279 ) ) ;
#117985 = CYLINDRICAL_SURFACE ( 'NONE', #6570, 1.000000000000000888 ) ;
#117986 = CARTESIAN_POINT ( 'NONE',  ( 11.64999999999990798, 2.500000000000000000, -2.857883832488653741 ) ) ;
#117987 = AXIS2_PLACEMENT_3D ( 'NONE', #27587, #77997, #58377 ) ;
#117988 = VECTOR ( 'NONE', #123386, 1000.000000000000000 ) ;
#117989 = ORIENTED_EDGE ( 'NONE', *, *, #33174, .T. ) ;
#117990 = ORIENTED_EDGE ( 'NONE', *, *, #21054, .T. ) ;
#117991 = FACE_OUTER_BOUND ( 'NONE', #97371, .T. ) ;
#117992 = DIRECTION ( 'NONE',  ( 0.000000000000000000, 1.000000000000000000, 0.000000000000000000 ) ) ;
#117993 = ORIENTED_EDGE ( 'NONE', *, *, #75095, .F. ) ;
#117994 = CARTESIAN_POINT ( 'NONE',  ( 11.64999999999990266, 12.50000000000000000, 2.230156782645134950 ) ) ;
#117995 = CARTESIAN_POINT ( 'NONE',  ( 187.1927083336747160, 6.551208109652275624, -3.782341765624998686 ) ) ;
#117996 = CIRCLE ( 'NONE', #122221, 0.1000000000000002554 ) ;
#117997 = AXIS2_PLACEMENT_3D ( 'NONE', #27536, #85187, #15135 ) ;
#117998 = CONICAL_SURFACE ( 'NONE', #61595, 0.1000000000000002554, 0.003490658503988666988 ) ;
#117999 = DIRECTION ( 'NONE',  ( -4.274815082592931898E-19, -0.9999939076577903929, -0.003490651415223739937 ) ) ;
#118000 = DIRECTION ( 'NONE',  ( 0.000000000000000000, 1.000000000000000000, 0.000000000000000000 ) ) ;
#118001 = VECTOR ( 'NONE', #26188, 1000.000000000000000 ) ;
#118002 = DIRECTION ( 'NONE',  ( 0.000000000000000000, -0.9999939076577903929, 0.003490651415223739937 ) ) ;
#118003 = CARTESIAN_POINT ( 'NONE',  ( 12.69999999999990159, 2.500000000000000000, 4.676537180435972552 ) ) ;
#118004 = AXIS2_PLACEMENT_3D ( 'NONE', #65427, #94247, #84431 ) ;
#118005 = CIRCLE ( 'NONE', #30302, 0.06509327318403745899 ) ;
#118006 = EDGE_LOOP ( 'NONE', ( #126453, #101517, #17090, #53338 ) ) ;
#118007 = ORIENTED_EDGE ( 'NONE', *, *, #65516, .T. ) ;
#118008 = ORIENTED_EDGE ( 'NONE', *, *, #126703, .F. ) ;
#118009 = ORIENTED_EDGE ( 'NONE', *, *, #18073, .F. ) ;
#118010 = DIRECTION ( 'NONE',  ( -0.000000000000000000, -1.000000000000000000, -0.000000000000000000 ) ) ;
#118011 = CARTESIAN_POINT ( 'NONE',  ( 133.2169897921533845, 0.5000000000000000000, -2.337293474289257933 ) ) ;
#118012 = AXIS2_PLACEMENT_3D ( 'NONE', #113758, #54812, #14240 ) ;
#118013 = CARTESIAN_POINT ( 'NONE',  ( 9.149999999999916866, 12.50000000000000000, -1.472243186433550122 ) ) ;
#118014 = ORIENTED_EDGE ( 'NONE', *, *, #33434, .T. ) ;
#118015 = FACE_BOUND ( 'NONE', #33022, .T. ) ;
#118016 = ORIENTED_EDGE ( 'NONE', *, *, #99457, .T. ) ;
#118017 = EDGE_CURVE ( 'NONE', #63986, #98143, #126685, .T. ) ;
#118018 = CARTESIAN_POINT ( 'NONE',  ( -14.99999999999998401, 12.50000000000000000, 0.7579135962115892688 ) ) ;
#118019 = LINE ( 'NONE', #46710, #75156 ) ;
#118020 = ADVANCED_FACE ( 'NONE', ( #81249 ), #51152, .T. ) ;
#118021 = DIRECTION ( 'NONE',  ( 0.000000000000000000, 1.000000000000000000, 0.000000000000000000 ) ) ;
#118022 = FACE_OUTER_BOUND ( 'NONE', #63369, .T. ) ;
#118023 = EDGE_CURVE ( 'NONE', #65136, #97390, #57742, .T. ) ;
#118024 = DIRECTION ( 'NONE',  ( -0.000000000000000000, 1.000000000000000000, -0.000000000000000000 ) ) ;
#118025 = DIRECTION ( 'NONE',  ( 0.000000000000000000, 0.000000000000000000, -1.000000000000000000 ) ) ;
#118026 = PLANE ( 'NONE',  #81271 ) ;
#118027 = DIRECTION ( 'NONE',  ( -0.000000000000000000, -1.000000000000000000, -0.000000000000000000 ) ) ;
#118028 = CARTESIAN_POINT ( 'NONE',  ( 10.84999999999991260, 2.500000000000000000, -2.857883832488653741 ) ) ;
#118030 = ADVANCED_FACE ( 'NONE', ( #91061 ), #62260, .T. ) ;
#118029 = LINE ( 'NONE', #68279, #127505 ) ;
#118031 = ORIENTED_EDGE ( 'NONE', *, *, #92835, .T. ) ;
#118032 = ORIENTED_EDGE ( 'NONE', *, *, #42804, .F. ) ;
#118033 = ORIENTED_EDGE ( 'NONE', *, *, #10766, .F. ) ;
#118034 = VERTEX_POINT ( 'NONE', #61617 ) ;
#118035 = CARTESIAN_POINT ( 'NONE',  ( 16.64732342996689596, -0.5906619305413305376, -5.996708608239496030 ) ) ;
#118036 = CARTESIAN_POINT ( 'NONE',  ( -7.950000000000012612, 2.500000000000000000, 2.165063509461097713 ) ) ;
#118038 = EDGE_LOOP ( 'NONE', ( #61820, #2490, #31328, #10021 ) ) ;
#118037 = ORIENTED_EDGE ( 'NONE', *, *, #16582, .F. ) ;
#118039 = VERTEX_POINT ( 'NONE', #22973 ) ;
#118040 = CARTESIAN_POINT ( 'NONE',  ( 2.099999999999950351, 12.50000000000000000, -4.265033745738164406 ) ) ;
#118041 = AXIS2_PLACEMENT_3D ( 'NONE', #105132, #104493, #95964 ) ;
#118042 = CIRCLE ( 'NONE', #118131, 0.1000000000000002554 ) ;
#118043 = CARTESIAN_POINT ( 'NONE',  ( 0.4499999999999569344, 12.50000000000000000, -2.099970236277064473 ) ) ;
#118044 = DIRECTION ( 'NONE',  ( -0.000000000000000000, 1.000000000000000000, -0.000000000000000000 ) ) ;
#118045 = CARTESIAN_POINT ( 'NONE',  ( 1.849999999999950573, 2.500000000000000000, 2.411473670974873862 ) ) ;
#118046 = DIRECTION ( 'NONE',  ( 0.000000000000000000, 0.000000000000000000, -1.000000000000000000 ) ) ;
#118047 = CARTESIAN_POINT ( 'NONE',  ( 6.249999999999965361, 12.50000000000000000, 2.165063509461097713 ) ) ;
#118048 = DIRECTION ( 'NONE',  ( 0.000000000000000000, 1.000000000000000000, 0.000000000000000000 ) ) ;
#118049 = EDGE_CURVE ( 'NONE', #87436, #11640, #82790, .T. ) ;
#118050 = VERTEX_POINT ( 'NONE', #13121 ) ;
#118051 = DIRECTION ( 'NONE',  ( 0.000000000000000000, 1.000000000000000000, 0.000000000000000000 ) ) ;
#118052 = VERTEX_POINT ( 'NONE', #11199 ) ;
#118053 = CIRCLE ( 'NONE', #61634, 0.1000000000000002554 ) ;
#118054 = ORIENTED_EDGE ( 'NONE', *, *, #78360, .T. ) ;
#118055 = ORIENTED_EDGE ( 'NONE', *, *, #32351, .F. ) ;
#118056 = AXIS2_PLACEMENT_3D ( 'NONE', #74704, #16397, #44602 ) ;
#118057 = CARTESIAN_POINT ( 'NONE',  ( -2.700000000000029932, 2.500000000000000000, -4.676537180435977881 ) ) ;
#118058 = VERTEX_POINT ( 'NONE', #112642 ) ;
#118059 = ORIENTED_EDGE ( 'NONE', *, *, #43160, .T. ) ;
#118060 = DIRECTION ( 'NONE',  ( -4.274815082592931898E-19, -0.9999939076577903929, -0.003490651415223739937 ) ) ;
#118062 = CIRCLE ( 'NONE', #3061, 0.06509327318403745899 ) ;
#118061 = DIRECTION ( 'NONE',  ( 0.000000000000000000, 0.000000000000000000, -1.000000000000000000 ) ) ;
#118063 = LINE ( 'NONE', #125941, #83367 ) ;
#118064 = CIRCLE ( 'NONE', #95092, 0.06509327318403745899 ) ;
#118065 = ADVANCED_FACE ( 'NONE', ( #60949 ), #121164, .T. ) ;
#118066 = DIRECTION ( 'NONE',  ( -0.000000000000000000, 1.000000000000000000, -0.000000000000000000 ) ) ;
#118068 = AXIS2_PLACEMENT_3D ( 'NONE', #10477, #22750, #3725 ) ;
#118067 = CARTESIAN_POINT ( 'NONE',  ( -1.450000000000035483, 2.500000000000000000, 6.048780366869521252 ) ) ;
#118069 = VERTEX_POINT ( 'NONE', #1381 ) ;
#118070 = CIRCLE ( 'NONE', #30269, 0.06509327318403745899 ) ;
#118071 = CARTESIAN_POINT ( 'NONE',  ( -9.150000000000009237, 2.500000000000000000, -2.957883832488653830 ) ) ;
#118072 = VERTEX_POINT ( 'NONE', #100867 ) ;
#118073 = CARTESIAN_POINT ( 'NONE',  ( 21.25104878432635758, 0.2455272941110370200, 4.189300629079955485 ) ) ;
#118074 = EDGE_LOOP ( 'NONE', ( #17780, #119260 ) ) ;
#118075 = CARTESIAN_POINT ( 'NONE',  ( -13.94999999999998685, 12.50000000000000000, -2.511473670974875727 ) ) ;
#118076 = DIRECTION ( 'NONE',  ( 0.000000000000000000, 1.000000000000000000, 0.000000000000000000 ) ) ;
#118077 = ORIENTED_EDGE ( 'NONE', *, *, #70273, .F. ) ;
#118078 = CARTESIAN_POINT ( 'NONE',  ( -5.850000000000019185, 2.500000000000000000, 2.165063509461097713 ) ) ;
#118079 = ADVANCED_FACE ( 'NONE', ( #53074 ), #11754, .T. ) ;
#118080 = CARTESIAN_POINT ( 'NONE',  ( 0.3999999999999559464, 2.500000000000000000, -4.230127018922201998 ) ) ;
#118081 = EDGE_LOOP ( 'NONE', ( #113206, #50845 ) ) ;
#118082 = CIRCLE ( 'NONE', #5202, 0.09999999999999982514 ) ;
#118083 = CARTESIAN_POINT ( 'NONE',  ( 1.249999999999953815, 12.50000000000000000, -2.792790559304616504 ) ) ;
#118084 = ORIENTED_EDGE ( 'NONE', *, *, #89318, .F. ) ;
#118085 = AXIS2_PLACEMENT_3D ( 'NONE', #48174, #97269, #38373 ) ;
#118087 = ORIENTED_EDGE ( 'NONE', *, *, #112201, .T. ) ;
#118086 = EDGE_CURVE ( 'NONE', #21308, #114987, #47276, .T. ) ;
#118088 = DIRECTION ( 'NONE',  ( 0.000000000000000000, 1.000000000000000000, 0.000000000000000000 ) ) ;
#118089 = CARTESIAN_POINT ( 'NONE',  ( 13.09999999999990195, 2.500000000000000000, -4.083716857408426826 ) ) ;
#118090 = CARTESIAN_POINT ( 'NONE',  ( 186.8802083336747444, 4.367472073101515306, 7.564683531250000925 ) ) ;
#118091 = CARTESIAN_POINT ( 'NONE',  ( -11.24999999999999822, 2.500000000000000000, 5.802370205355744659 ) ) ;
#118092 = AXIS2_PLACEMENT_3D ( 'NONE', #58036, #121297, #72211 ) ;
#118093 = DIRECTION ( 'NONE',  ( -0.000000000000000000, 1.000000000000000000, -0.000000000000000000 ) ) ;
#118094 = CIRCLE ( 'NONE', #111849, 0.09999999999999982514 ) ;
#118095 = DIRECTION ( 'NONE',  ( -0.000000000000000000, -1.000000000000000000, -0.000000000000000000 ) ) ;
#118096 = AXIS2_PLACEMENT_3D ( 'NONE', #21359, #69821, #101216 ) ;
#118097 = ORIENTED_EDGE ( 'NONE', *, *, #5381, .T. ) ;
#118098 = VECTOR ( 'NONE', #107123, 1000.000000000000000 ) ;
#118099 = DIRECTION ( 'NONE',  ( 0.000000000000000000, 1.000000000000000000, 0.000000000000000000 ) ) ;
#118101 = AXIS2_PLACEMENT_3D ( 'NONE', #32413, #93241, #94510 ) ;
#118100 = DIRECTION ( 'NONE',  ( -4.274815082592931898E-19, -0.9999939076577903929, -0.003490651415223739937 ) ) ;
#118102 = EDGE_CURVE ( 'NONE', #104178, #31905, #2024, .T. ) ;
#118103 = EDGE_LOOP ( 'NONE', ( #54232, #102986 ) ) ;
#118104 = AXIS2_PLACEMENT_3D ( 'NONE', #68835, #9277, #17119 ) ;
#118105 = CARTESIAN_POINT ( 'NONE',  ( 2.899999999999946620, 2.500000000000000000, 0.6928203230275494784 ) ) ;
#118106 = DIRECTION ( 'NONE',  ( -0.000000000000000000, -1.000000000000000000, -0.000000000000000000 ) ) ;
#118107 = DIRECTION ( 'NONE',  ( 0.000000000000000000, 1.000000000000000000, 0.000000000000000000 ) ) ;
#118108 = CARTESIAN_POINT ( 'NONE',  ( -12.09999999999999609, 2.500000000000000000, 4.230127018922196669 ) ) ;
#118109 = DIRECTION ( 'NONE',  ( 0.000000000000000000, 0.000000000000000000, -1.000000000000000000 ) ) ;
#118110 = ORIENTED_EDGE ( 'NONE', *, *, #123234, .T. ) ;
#118111 = EDGE_CURVE ( 'NONE', #82534, #23974, #128767, .T. ) ;
#118112 = CARTESIAN_POINT ( 'NONE',  ( 8.149999999999923972, 12.50000000000000000, 1.818653347947321475 ) ) ;
#118113 = CARTESIAN_POINT ( 'NONE',  ( 8.349999999999919709, 12.50000000000000000, -2.165063509461101710 ) ) ;
#118114 = EDGE_CURVE ( 'NONE', #115792, #21808, #38982, .T. ) ;
#118115 = EDGE_CURVE ( 'NONE', #64039, #129191, #121800, .T. ) ;
#118116 = EDGE_CURVE ( 'NONE', #87809, #83720, #118357, .T. ) ;
#118117 = ADVANCED_FACE ( 'NONE', ( #119876 ), #30232, .T. ) ;
#118118 = CIRCLE ( 'NONE', #15704, 0.1000000000000002554 ) ;
#118119 = EDGE_LOOP ( 'NONE', ( #78757, #6622, #36517, #58263 ) ) ;
#118120 = LINE ( 'NONE', #28469, #72007 ) ;
#118121 = VERTEX_POINT ( 'NONE', #122468 ) ;
#118122 = VERTEX_POINT ( 'NONE', #32806 ) ;
#118123 = LINE ( 'NONE', #8802, #96881 ) ;
#118124 = EDGE_CURVE ( 'NONE', #96385, #66216, #61942, .T. ) ;
#118125 = EDGE_CURVE ( 'NONE', #46700, #89750, #737, .T. ) ;
#118126 = ORIENTED_EDGE ( 'NONE', *, *, #108634, .T. ) ;
#118127 = FACE_OUTER_BOUND ( 'NONE', #526, .T. ) ;
#118128 = CARTESIAN_POINT ( 'NONE',  ( 11.89999999999990443, 2.500000000000000000, -0.2464101615137782308 ) ) ;
#118129 = EDGE_CURVE ( 'NONE', #127931, #100949, #66102, .T. ) ;
#118130 = CARTESIAN_POINT ( 'NONE',  ( 9.599999999999914380, 2.500000000000000000, -3.637306695894650055 ) ) ;
#118131 = AXIS2_PLACEMENT_3D ( 'NONE', #37196, #124281, #34627 ) ;
#118132 = VERTEX_POINT ( 'NONE', #25522 ) ;
#118133 = ADVANCED_FACE ( 'NONE', ( #43908 ), #45215, .T. ) ;
#118135 = EDGE_CURVE ( 'NONE', #8551, #27240, #53709, .T. ) ;
#118134 = CARTESIAN_POINT ( 'NONE',  ( 7.499999999999925393, 12.50000000000000000, -0.7579135962115916003 ) ) ;
#118137 = ORIENTED_EDGE ( 'NONE', *, *, #18417, .T. ) ;
#118136 = FACE_OUTER_BOUND ( 'NONE', #103675, .T. ) ;
#118138 = FACE_OUTER_BOUND ( 'NONE', #98407, .T. ) ;
#118139 = EDGE_CURVE ( 'NONE', #43500, #53553, #41026, .T. ) ;
#118140 = CARTESIAN_POINT ( 'NONE',  ( -9.150000000000009237, 2.500000000000000000, -2.857883832488653741 ) ) ;
#118141 = ADVANCED_FACE ( 'NONE', ( #63540 ), #26191, .T. ) ;
#118142 = VERTEX_POINT ( 'NONE', #64814 ) ;
#118143 = AXIS2_PLACEMENT_3D ( 'NONE', #36040, #15736, #106696 ) ;
#118144 = EDGE_LOOP ( 'NONE', ( #31863, #91671 ) ) ;
#118145 = AXIS2_PLACEMENT_3D ( 'NONE', #78444, #58150, #39805 ) ;
#118146 = ORIENTED_EDGE ( 'NONE', *, *, #115858, .F. ) ;
#118147 = DIRECTION ( 'NONE',  ( -4.274815082592931898E-19, -0.9999939076577903929, -0.003490651415223739937 ) ) ;
#118148 = DIRECTION ( 'NONE',  ( -0.000000000000000000, -1.000000000000000000, -0.000000000000000000 ) ) ;
#118149 = DIRECTION ( 'NONE',  ( -0.000000000000000000, -1.000000000000000000, -0.000000000000000000 ) ) ;
#118150 = FACE_BOUND ( 'NONE', #12646, .T. ) ;
#118151 = ORIENTED_EDGE ( 'NONE', *, *, #63455, .F. ) ;
#118152 = DIRECTION ( 'NONE',  ( 0.000000000000000000, 0.000000000000000000, -1.000000000000000000 ) ) ;
#118153 = CARTESIAN_POINT ( 'NONE',  ( -2.900000000000030553, 2.500000000000000000, 4.922947341949748257 ) ) ;
#118154 = EDGE_LOOP ( 'NONE', ( #85585, #46253, #105626, #30020, #11380, #21460, #53421, #90818 ) ) ;
#118155 = DIRECTION ( 'NONE',  ( 0.000000000000000000, -0.9999939076577903929, 0.003490651415223739937 ) ) ;
#118157 = DIRECTION ( 'NONE',  ( -0.000000000000000000, -1.000000000000000000, -0.000000000000000000 ) ) ;
#118156 = VECTOR ( 'NONE', #100453, 1000.000000000000000 ) ;
#118158 = CONICAL_SURFACE ( 'NONE', #9501, 0.1000000000000002554, 0.003490658503988666988 ) ;
#118159 = DIRECTION ( 'NONE',  ( 0.000000000000000000, -0.9999939076577903929, 0.003490651415223739937 ) ) ;
#118160 = DIRECTION ( 'NONE',  ( -0.000000000000000000, 1.000000000000000000, -0.000000000000000000 ) ) ;
#118161 = DIRECTION ( 'NONE',  ( 0.000000000000000000, 0.000000000000000000, -1.000000000000000000 ) ) ;
#118162 = DIRECTION ( 'NONE',  ( 0.000000000000000000, -0.000000000000000000, 1.000000000000000000 ) ) ;
#118163 = CARTESIAN_POINT ( 'NONE',  ( 6.049999999999932321, 2.500000000000000000, 1.818653347947321475 ) ) ;
#118164 = ORIENTED_EDGE ( 'NONE', *, *, #65682, .T. ) ;
#118165 = ORIENTED_EDGE ( 'NONE', *, *, #42302, .T. ) ;
#118166 = ORIENTED_EDGE ( 'NONE', *, *, #58146, .T. ) ;
#118167 = AXIS2_PLACEMENT_3D ( 'NONE', #1168, #90169, #69916 ) ;
#118168 = ORIENTED_EDGE ( 'NONE', *, *, #8937, .T. ) ;
#118169 = VERTEX_POINT ( 'NONE', #13777 ) ;
#118170 = CARTESIAN_POINT ( 'NONE',  ( -2.950000000000029932, 12.50000000000000000, -2.230156782645139391 ) ) ;
#118171 = CARTESIAN_POINT ( 'NONE',  ( -8.749999999999975131, 12.50000000000000000, -2.165063509461101710 ) ) ;
#118172 = ORIENTED_EDGE ( 'NONE', *, *, #124808, .F. ) ;
#118173 = FACE_BOUND ( 'NONE', #121904, .T. ) ;
#118174 = AXIS2_PLACEMENT_3D ( 'NONE', #124353, #123062, #33408 ) ;
#118175 = DIRECTION ( 'NONE',  ( 0.000000000000000000, 0.000000000000000000, -1.000000000000000000 ) ) ;
#118176 = ADVANCED_FACE ( 'NONE', ( #125027 ), #95472, .T. ) ;
#118177 = AXIS2_PLACEMENT_3D ( 'NONE', #103928, #82371, #22169 ) ;
#118178 = DIRECTION ( 'NONE',  ( 0.000000000000000000, 0.000000000000000000, 1.000000000000000000 ) ) ;
#118179 = AXIS2_PLACEMENT_3D ( 'NONE', #27145, #95886, #55949 ) ;
#118180 = EDGE_CURVE ( 'NONE', #56415, #123846, #95384, .T. ) ;
#118181 = AXIS2_PLACEMENT_3D ( 'NONE', #7272, #77315, #54448 ) ;
#118182 = CARTESIAN_POINT ( 'NONE',  ( 186.2500000000000000, 9.429780353434619030E-16, -7.700000000000000178 ) ) ;
#118183 = CARTESIAN_POINT ( 'NONE',  ( -6.071532165918824830E-15, 2.500000000000000000, -4.230127018922201998 ) ) ;
#118184 = PLANE ( 'NONE',  #114476 ) ;
#118185 = EDGE_LOOP ( 'NONE', ( #47734, #87876 ) ) ;
#118186 = CARTESIAN_POINT ( 'NONE',  ( 11.64999999999990798, 12.50000000000000000, -2.857883832488653741 ) ) ;
#118188 = EDGE_CURVE ( 'NONE', #10182, #112593, #72501, .T. ) ;
#118187 = AXIS2_PLACEMENT_3D ( 'NONE', #64935, #14546, #95711 ) ;
#118189 = VERTEX_POINT ( 'NONE', #14416 ) ;
#118190 = CIRCLE ( 'NONE', #78508, 0.06509327318403745899 ) ;
#118191 = CONICAL_SURFACE ( 'NONE', #49254, 0.1000000000000002554, 0.003490658503988666988 ) ;
#118192 = EDGE_LOOP ( 'NONE', ( #60521, #91912, #34441, #29115 ) ) ;
#118193 = ORIENTED_EDGE ( 'NONE', *, *, #11631, .T. ) ;
#118194 = DIRECTION ( 'NONE',  ( -0.000000000000000000, -1.000000000000000000, -0.000000000000000000 ) ) ;
#118195 = AXIS2_PLACEMENT_3D ( 'NONE', #113607, #114886, #114250 ) ;
#118196 = CARTESIAN_POINT ( 'NONE',  ( 6.598553918464142853, 2.500000000000000000, 8.770211965307137092 ) ) ;
#118197 = CARTESIAN_POINT ( 'NONE',  ( 0.6499999999999561684, 2.500000000000000000, 1.818653347947321475 ) ) ;
#118198 = ORIENTED_EDGE ( 'NONE', *, *, #91798, .T. ) ;
#118199 = FACE_OUTER_BOUND ( 'NONE', #123392, .T. ) ;
#118200 = AXIS2_PLACEMENT_3D ( 'NONE', #73426, #81333, #12570 ) ;
#118201 = DIRECTION ( 'NONE',  ( -0.000000000000000000, 1.000000000000000000, -0.000000000000000000 ) ) ;
#118202 = AXIS2_PLACEMENT_3D ( 'NONE', #95045, #13885, #92452 ) ;
#118203 = DIRECTION ( 'NONE',  ( 0.000000000000000000, -0.000000000000000000, 1.000000000000000000 ) ) ;
#118204 = CARTESIAN_POINT ( 'NONE',  ( 185.8593750003413732, 0.000000000000000000, 7.564683531250000925 ) ) ;
#118205 = CARTESIAN_POINT ( 'NONE',  ( 6.849999999999929479, 12.50000000000000000, -1.818653347947326138 ) ) ;
#118207 = CIRCLE ( 'NONE', #76442, 0.1000000000000002554 ) ;
#118206 = CARTESIAN_POINT ( 'NONE',  ( -12.69999999999999218, 2.500000000000000000, 4.576537180435972019 ) ) ;
#118208 = FACE_OUTER_BOUND ( 'NONE', #106722, .T. ) ;
#118209 = VERTEX_POINT ( 'NONE', #104103 ) ;
#118210 = FACE_OUTER_BOUND ( 'NONE', #42736, .T. ) ;
#118211 = ORIENTED_EDGE ( 'NONE', *, *, #105284, .T. ) ;
#118212 = VERTEX_POINT ( 'NONE', #83186 ) ;
#118213 = CARTESIAN_POINT ( 'NONE',  ( 6.049999999999932321, 2.500000000000000000, 6.841600689897072485 ) ) ;
#118214 = DIRECTION ( 'NONE',  ( 0.000000000000000000, 0.000000000000000000, 1.000000000000000000 ) ) ;
#118215 = CARTESIAN_POINT ( 'NONE',  ( -11.64999999999999680, 2.500000000000000000, 5.802370205355744659 ) ) ;
#118216 = AXIS2_PLACEMENT_3D ( 'NONE', #75348, #5956, #116562 ) ;
#118217 = ORIENTED_EDGE ( 'NONE', *, *, #26962, .T. ) ;
#118218 = ORIENTED_EDGE ( 'NONE', *, *, #48127, .F. ) ;
#118219 = EDGE_CURVE ( 'NONE', #115955, #22580, #75923, .T. ) ;
#118220 = DIRECTION ( 'NONE',  ( 0.000000000000000000, 1.000000000000000000, 0.000000000000000000 ) ) ;
#118221 = DIRECTION ( 'NONE',  ( -0.000000000000000000, 1.000000000000000000, -0.000000000000000000 ) ) ;
#118222 = CARTESIAN_POINT ( 'NONE',  ( -15.39999999999997904, 2.500000000000000000, 0.000000000000000000 ) ) ;
#118223 = VERTEX_POINT ( 'NONE', #36013 ) ;
#118224 = VERTEX_POINT ( 'NONE', #93642 ) ;
#118225 = CARTESIAN_POINT ( 'NONE',  ( -6.249999999999981348, 2.500000000000000000, 2.265063509461097357 ) ) ;
#118226 = AXIS2_PLACEMENT_3D ( 'NONE', #50564, #61701, #120604 ) ;
#118227 = ADVANCED_FACE ( 'NONE', ( #123103 ), #68273, .T. ) ;
#118228 = AXIS2_PLACEMENT_3D ( 'NONE', #19843, #7420, #68927 ) ;
#118229 = ORIENTED_EDGE ( 'NONE', *, *, #101596, .T. ) ;
#118230 = CARTESIAN_POINT ( 'NONE',  ( 7.099999999999928590, 2.500000000000000000, 3.637306695894644726 ) ) ;
#118231 = DIRECTION ( 'NONE',  ( -0.000000000000000000, 1.000000000000000000, -0.000000000000000000 ) ) ;
#118232 = ORIENTED_EDGE ( 'NONE', *, *, #52950, .T. ) ;
#118233 = DIRECTION ( 'NONE',  ( 0.000000000000000000, 0.000000000000000000, 1.000000000000000000 ) ) ;
#118234 = FACE_OUTER_BOUND ( 'NONE', #50537, .T. ) ;
#118235 = DIRECTION ( 'NONE',  ( -0.000000000000000000, 1.000000000000000000, -0.000000000000000000 ) ) ;
#118236 = EDGE_CURVE ( 'NONE', #91313, #11053, #105394, .T. ) ;
#118237 = EDGE_CURVE ( 'NONE', #65076, #106610, #80813, .T. ) ;
#118238 = PLANE ( 'NONE',  #41670 ) ;
#118239 = ORIENTED_EDGE ( 'NONE', *, *, #74835, .F. ) ;
#118240 = CONICAL_SURFACE ( 'NONE', #49314, 0.09999999999999999167, 0.003490658503988666988 ) ;
#118241 = DIRECTION ( 'NONE',  ( 0.000000000000000000, 0.000000000000000000, 1.000000000000000000 ) ) ;
#118242 = EDGE_LOOP ( 'NONE', ( #54036, #117681, #35926, #35011 ) ) ;
#118243 = ORIENTED_EDGE ( 'NONE', *, *, #78244, .F. ) ;
#118244 = EDGE_CURVE ( 'NONE', #3245, #27692, #54352, .T. ) ;
#118245 = CARTESIAN_POINT ( 'NONE',  ( -4.600000000000028066, 12.50000000000000000, -3.702399969078687292 ) ) ;
#118246 = CARTESIAN_POINT ( 'NONE',  ( 11.44999999999991047, 2.500000000000000000, 6.148780366869520009 ) ) ;
#118247 = CARTESIAN_POINT ( 'NONE',  ( -0.6500000000000403233, 12.50000000000000000, 1.883746621131358934 ) ) ;
#118248 = DIRECTION ( 'NONE',  ( -0.000000000000000000, -1.000000000000000000, -0.000000000000000000 ) ) ;
#118249 = CARTESIAN_POINT ( 'NONE',  ( -5.450000000000019718, 2.500000000000000000, 2.165063509461097713 ) ) ;
#118250 = CARTESIAN_POINT ( 'NONE',  ( 6.899999999999928413, 12.50000000000000000, -4.048810130592463530 ) ) ;
#118251 = AXIS2_PLACEMENT_3D ( 'NONE', #69539, #107544, #110120 ) ;
#118252 = AXIS2_PLACEMENT_3D ( 'NONE', #74085, #26282, #35462 ) ;
#118253 = PLANE ( 'NONE',  #92689 ) ;
#118254 = LINE ( 'NONE', #60010, #59564 ) ;
#118255 = LINE ( 'NONE', #30548, #88090 ) ;
#118256 = LINE ( 'NONE', #77675, #89835 ) ;
#118257 = ORIENTED_EDGE ( 'NONE', *, *, #97552, .F. ) ;
#118258 = PLANE ( 'NONE',  #127879 ) ;
#118259 = CARTESIAN_POINT ( 'NONE',  ( 4.149999999999941735, 12.50000000000000000, -7.188010851410854052 ) ) ;
#118260 = DIRECTION ( 'NONE',  ( 0.000000000000000000, 0.000000000000000000, -1.000000000000000000 ) ) ;
#118261 = CARTESIAN_POINT ( 'NONE',  ( -2.050000000000033129, 2.500000000000000000, 2.165063509461097713 ) ) ;
#118262 = FACE_OUTER_BOUND ( 'NONE', #70345, .T. ) ;
#118263 = ORIENTED_EDGE ( 'NONE', *, *, #103554, .T. ) ;
#118264 = DIRECTION ( 'NONE',  ( 0.000000000000000000, 1.000000000000000000, 0.000000000000000000 ) ) ;
#118265 = EDGE_CURVE ( 'NONE', #91647, #77185, #74000, .T. ) ;
#118266 = AXIS2_PLACEMENT_3D ( 'NONE', #34897, #6041, #64336 ) ;
#118267 = CARTESIAN_POINT ( 'NONE',  ( -1.850000000000033396, 2.500000000000000000, -2.511473670974877948 ) ) ;
#118269 = ORIENTED_EDGE ( 'NONE', *, *, #101586, .F. ) ;
#118268 = LINE ( 'NONE', #8306, #115238 ) ;
#118270 = ADVANCED_FACE ( 'NONE', ( #34743 ), #4576, .T. ) ;
#118271 = EDGE_CURVE ( 'NONE', #73967, #39963, #122581, .T. ) ;
#118272 = ORIENTED_EDGE ( 'NONE', *, *, #99345, .T. ) ;
#118273 = DIRECTION ( 'NONE',  ( 0.000000000000000000, 0.000000000000000000, 1.000000000000000000 ) ) ;
#118274 = VERTEX_POINT ( 'NONE', #106670 ) ;
#118275 = VERTEX_POINT ( 'NONE', #79173 ) ;
#118276 = ORIENTED_EDGE ( 'NONE', *, *, #124808, .T. ) ;
#118277 = DIRECTION ( 'NONE',  ( 0.000000000000000000, 0.000000000000000000, 1.000000000000000000 ) ) ;
#118278 = EDGE_CURVE ( 'NONE', #87285, #77424, #87033, .T. ) ;
#118279 = CIRCLE ( 'NONE', #5409, 0.1000000000000002554 ) ;
#118280 = EDGE_CURVE ( 'NONE', #119894, #33342, #84996, .T. ) ;
#118281 = EDGE_CURVE ( 'NONE', #98563, #119463, #126782, .T. ) ;
#118282 = LINE ( 'NONE', #67892, #94580 ) ;
#118283 = CARTESIAN_POINT ( 'NONE',  ( -13.94999999999998863, 12.50000000000000000, 2.511473670974877503 ) ) ;
#118284 = AXIS2_PLACEMENT_3D ( 'NONE', #61773, #10691, #30382 ) ;
#118285 = DIRECTION ( 'NONE',  ( -4.274815082592931898E-19, -0.9999939076577903929, -0.003490651415223739937 ) ) ;
#118286 = AXIS2_PLACEMENT_3D ( 'NONE', #52349, #111920, #73276 ) ;
#118287 = ORIENTED_EDGE ( 'NONE', *, *, #64657, .T. ) ;
#118288 = AXIS2_PLACEMENT_3D ( 'NONE', #25640, #127087, #56389 ) ;
#118289 = EDGE_CURVE ( 'NONE', #81973, #49584, #1371, .T. ) ;
#118291 = AXIS2_PLACEMENT_3D ( 'NONE', #100709, #91550, #121642 ) ;
#118290 = CARTESIAN_POINT ( 'NONE',  ( -3.750000000000031086, 2.500000000000000000, -5.902370205355750521 ) ) ;
#118292 = ORIENTED_EDGE ( 'NONE', *, *, #55971, .T. ) ;
#118293 = DIRECTION ( 'NONE',  ( 0.000000000000000000, 0.000000000000000000, -1.000000000000000000 ) ) ;
#118294 = CARTESIAN_POINT ( 'NONE',  ( 15.44463772191480899, -2.469073678227705848, -4.264595835270768909 ) ) ;
#118295 = CARTESIAN_POINT ( 'NONE',  ( 17.88933034088993068, 0.4802206367765988193, 4.999988745079567920 ) ) ;
#118296 = CARTESIAN_POINT ( 'NONE',  ( 10.59999999999990905, 12.50000000000000000, -3.983716857408426293 ) ) ;
#118297 = CARTESIAN_POINT ( 'NONE',  ( -12.09999999999999609, 2.500000000000000000, -4.330127018922198978 ) ) ;
#118298 = ADVANCED_FACE ( 'NONE', ( #56912 ), #18101, .T. ) ;
#118299 = ORIENTED_EDGE ( 'NONE', *, *, #19990, .F. ) ;
#118300 = ORIENTED_EDGE ( 'NONE', *, *, #98613, .T. ) ;
#118301 = ORIENTED_EDGE ( 'NONE', *, *, #2274, .T. ) ;
#118302 = ORIENTED_EDGE ( 'NONE', *, *, #4265, .T. ) ;
#118303 = ORIENTED_EDGE ( 'NONE', *, *, #90621, .F. ) ;
#118304 = CARTESIAN_POINT ( 'NONE',  ( 12.49999999999993960, 2.500000000000000000, -4.230127018922201998 ) ) ;
#118305 = CARTESIAN_POINT ( 'NONE',  ( -6.650000000000014566, 12.50000000000000000, 5.802370205355744659 ) ) ;
#118306 = CARTESIAN_POINT ( 'NONE',  ( 0.1999999999999562961, 12.50000000000000000, 4.676537180435972552 ) ) ;
#118307 = FACE_BOUND ( 'NONE', #22981, .T. ) ;
#118308 = DIRECTION ( 'NONE',  ( 0.000000000000000000, 0.000000000000000000, -1.000000000000000000 ) ) ;
#118309 = VECTOR ( 'NONE', #24821, 1000.000000000000000 ) ;
#118310 = DIRECTION ( 'NONE',  ( -4.274815082592931898E-19, -0.9999939076577903929, -0.003490651415223739937 ) ) ;
#118311 = DIRECTION ( 'NONE',  ( -0.000000000000000000, -1.000000000000000000, -0.000000000000000000 ) ) ;
#118312 = CARTESIAN_POINT ( 'NONE',  ( -0.6500000000000394351, 2.500000000000000000, 6.741600689897071952 ) ) ;
#118313 = CARTESIAN_POINT ( 'NONE',  ( 185.8802083336747444, 4.367472073101515306, 7.564683531250000925 ) ) ;
#118314 = AXIS2_PLACEMENT_3D ( 'NONE', #102098, #62188, #100169 ) ;
#118315 = CARTESIAN_POINT ( 'NONE',  ( -4.150000000000024336, 12.50000000000000000, -2.165063509461101710 ) ) ;
#118316 = CARTESIAN_POINT ( 'NONE',  ( -8.100000000000013856, 2.500000000000000000, 0.4464101615137736623 ) ) ;
#118317 = AXIS2_PLACEMENT_3D ( 'NONE', #122041, #32395, #36239 ) ;
#118318 = AXIS2_PLACEMENT_3D ( 'NONE', #101103, #103027, #83410 ) ;
#118319 = CARTESIAN_POINT ( 'NONE',  ( 1.849999999999950573, 12.50000000000000000, 2.511473670974873507 ) ) ;
#118320 = VECTOR ( 'NONE', #96248, 1000.000000000000000 ) ;
#118321 = ORIENTED_EDGE ( 'NONE', *, *, #85311, .T. ) ;
#118322 = VERTEX_POINT ( 'NONE', #87671 ) ;
#118323 = ORIENTED_EDGE ( 'NONE', *, *, #50320, .T. ) ;
#118324 = ORIENTED_EDGE ( 'NONE', *, *, #45859, .T. ) ;
#118325 = DIRECTION ( 'NONE',  ( 0.000000000000000000, 0.000000000000000000, -1.000000000000000000 ) ) ;
#118326 = DIRECTION ( 'NONE',  ( 0.000000000000000000, -0.9999939076577903929, 0.003490651415223739937 ) ) ;
#118327 = FACE_BOUND ( 'NONE', #37386, .T. ) ;
#118329 = DIRECTION ( 'NONE',  ( 0.000000000000000000, -0.9999939076577903929, 0.003490651415223739937 ) ) ;
#118328 = AXIS2_PLACEMENT_3D ( 'NONE', #35887, #75795, #115723 ) ;
#118330 = ADVANCED_FACE ( 'NONE', ( #86385 ), #15940, .T. ) ;
#118332 = CIRCLE ( 'NONE', #32593, 0.06509327318403745899 ) ;
#118331 = CIRCLE ( 'NONE', #22213, 0.1000000000000002554 ) ;
#118333 = VERTEX_POINT ( 'NONE', #38609 ) ;
#118334 = DIRECTION ( 'NONE',  ( 0.000000000000000000, 0.000000000000000000, -1.000000000000000000 ) ) ;
#118335 = DIRECTION ( 'NONE',  ( -0.000000000000000000, -1.000000000000000000, -0.000000000000000000 ) ) ;
#118336 = DIRECTION ( 'NONE',  ( 0.000000000000000000, 0.000000000000000000, 1.000000000000000000 ) ) ;
#118337 = DIRECTION ( 'NONE',  ( -4.274815082592931898E-19, -0.9999939076577903929, -0.003490651415223739937 ) ) ;
#118338 = ORIENTED_EDGE ( 'NONE', *, *, #52100, .T. ) ;
#118339 = DIRECTION ( 'NONE',  ( -0.000000000000000000, 1.000000000000000000, -0.000000000000000000 ) ) ;
#118340 = ADVANCED_FACE ( 'NONE', ( #36670 ), #67361, .T. ) ;
#118341 = ORIENTED_EDGE ( 'NONE', *, *, #115906, .F. ) ;
#118342 = ORIENTED_EDGE ( 'NONE', *, *, #25155, .T. ) ;
#118343 = FACE_OUTER_BOUND ( 'NONE', #12769, .T. ) ;
#118344 = CARTESIAN_POINT ( 'NONE',  ( 0.6499999999999561684, 2.500000000000000000, 1.918653347947321564 ) ) ;
#118345 = ORIENTED_EDGE ( 'NONE', *, *, #84847, .F. ) ;
#118346 = DIRECTION ( 'NONE',  ( 0.000000000000000000, 1.000000000000000000, 0.000000000000000000 ) ) ;
#118347 = DIRECTION ( 'NONE',  ( -0.000000000000000000, 1.000000000000000000, -0.000000000000000000 ) ) ;
#118348 = ORIENTED_EDGE ( 'NONE', *, *, #88179, .F. ) ;
#118349 = CARTESIAN_POINT ( 'NONE',  ( -9.550000000000002487, 12.50000000000000000, 6.430097255199259010 ) ) ;
#118350 = ORIENTED_EDGE ( 'NONE', *, *, #81365, .F. ) ;
#118351 = CARTESIAN_POINT ( 'NONE',  ( -12.49999999999999289, 2.500000000000000000, -0.6928203230275500335 ) ) ;
#118352 = EDGE_LOOP ( 'NONE', ( #61105, #42706, #13204, #98696 ) ) ;
#118353 = CARTESIAN_POINT ( 'NONE',  ( 186.7395833340161175, 4.445597072760133273, 7.699999999999975309 ) ) ;
#118354 = FACE_BOUND ( 'NONE', #45242, .T. ) ;
#118355 = VECTOR ( 'NONE', #106759, 1000.000000000000000 ) ;
#118356 = ORIENTED_EDGE ( 'NONE', *, *, #113232, .T. ) ;
#118357 = CIRCLE ( 'NONE', #99506, 0.06509327318403745899 ) ;
#118358 = CARTESIAN_POINT ( 'NONE',  ( 112.9991567705375388, 7.699452449333159976, -0.3520876866445218356 ) ) ;
#118359 = EDGE_LOOP ( 'NONE', ( #30972, #61620, #47719, #108705 ) ) ;
#118360 = CARTESIAN_POINT ( 'NONE',  ( -7.499999999999980460, 12.50000000000000000, -0.06509327318403970719 ) ) ;
#118361 = DIRECTION ( 'NONE',  ( 0.000000000000000000, 0.000000000000000000, -1.000000000000000000 ) ) ;
#118362 = CARTESIAN_POINT ( 'NONE',  ( 4.349999999999938360, 12.50000000000000000, 1.818653347947321475 ) ) ;
#118363 = CARTESIAN_POINT ( 'NONE',  ( -6.900000000000015454, 2.500000000000000000, 3.883716857408420431 ) ) ;
#118364 = DIRECTION ( 'NONE',  ( 0.000000000000000000, 0.000000000000000000, 1.000000000000000000 ) ) ;
#118365 = VERTEX_POINT ( 'NONE', #116487 ) ;
#118367 = ORIENTED_EDGE ( 'NONE', *, *, #95818, .F. ) ;
#118366 = VECTOR ( 'NONE', #56796, 1000.000000000000000 ) ;
#118369 = ORIENTED_EDGE ( 'NONE', *, *, #19328, .F. ) ;
#118368 = EDGE_CURVE ( 'NONE', #79214, #51306, #120519, .T. ) ;
#118370 = DIRECTION ( 'NONE',  ( 0.000000000000000000, 1.000000000000000000, 0.000000000000000000 ) ) ;
#118371 = CARTESIAN_POINT ( 'NONE',  ( 6.249999999999934275, 2.500000000000000000, -7.188010851410854052 ) ) ;
#118372 = DIRECTION ( 'NONE',  ( 0.000000000000000000, 1.000000000000000000, 0.000000000000000000 ) ) ;
#118374 = ORIENTED_EDGE ( 'NONE', *, *, #99654, .T. ) ;
#118373 = ORIENTED_EDGE ( 'NONE', *, *, #74389, .F. ) ;
#118375 = VERTEX_POINT ( 'NONE', #109245 ) ;
#118376 = CARTESIAN_POINT ( 'NONE',  ( 0.8499999999999550138, 12.50000000000000000, -5.867463478539787225 ) ) ;
#118377 = AXIS2_PLACEMENT_3D ( 'NONE', #66896, #36172, #108115 ) ;
#118379 = EDGE_CURVE ( 'NONE', #65189, #103138, #77852, .T. ) ;
#118378 = DIRECTION ( 'NONE',  ( 0.000000000000000000, 1.000000000000000000, 0.000000000000000000 ) ) ;
#118380 = CIRCLE ( 'NONE', #72425, 0.09999999999999982514 ) ;
#118381 = FACE_OUTER_BOUND ( 'NONE', #14494, .T. ) ;
#118382 = PLANE ( 'NONE',  #89928 ) ;
#118383 = DIRECTION ( 'NONE',  ( 0.000000000000000000, 0.000000000000000000, -1.000000000000000000 ) ) ;
#118384 = DIRECTION ( 'NONE',  ( 0.000000000000000000, 1.000000000000000000, 0.000000000000000000 ) ) ;
#118385 = CARTESIAN_POINT ( 'NONE',  ( 4.149999999999941735, 12.50000000000000000, -5.802370205355749988 ) ) ;
#118386 = EDGE_CURVE ( 'NONE', #61065, #5316, #16032, .T. ) ;
#118387 = EDGE_CURVE ( 'NONE', #91313, #79119, #64080, .T. ) ;
#118388 = PLANE ( 'NONE',  #75006 ) ;
#118389 = ORIENTED_EDGE ( 'NONE', *, *, #77893, .F. ) ;
#118390 = VERTEX_POINT ( 'NONE', #39260 ) ;
#118391 = LINE ( 'NONE', #119049, #63306 ) ;
#118392 = EDGE_CURVE ( 'NONE', #57054, #119412, #76598, .T. ) ;
#118393 = CARTESIAN_POINT ( 'NONE',  ( 129.5000000000000000, 0.000000000000000000, 6.000000000000000000 ) ) ;
#118394 = ORIENTED_EDGE ( 'NONE', *, *, #66103, .T. ) ;
#118395 = VERTEX_POINT ( 'NONE', #28128 ) ;
#118396 = EDGE_CURVE ( 'NONE', #3681, #48754, #107971, .T. ) ;
#118397 = CARTESIAN_POINT ( 'NONE',  ( 186.5260416670080588, -6.551208109652273848, -3.782341765625003571 ) ) ;
#118398 = CARTESIAN_POINT ( 'NONE',  ( -10.85000000000000142, 12.50000000000000000, 6.495190528383297135 ) ) ;
#118399 = VECTOR ( 'NONE', #61379, 1000.000000000000000 ) ;
#118400 = DIRECTION ( 'NONE',  ( -0.000000000000000000, 1.000000000000000000, -0.000000000000000000 ) ) ;
#118401 = DIRECTION ( 'NONE',  ( 0.000000000000000000, 1.000000000000000000, 0.000000000000000000 ) ) ;
#118402 = DIRECTION ( 'NONE',  ( 0.000000000000000000, 1.000000000000000000, 0.000000000000000000 ) ) ;
#118403 = CIRCLE ( 'NONE', #66166, 0.09999999999999999167 ) ;
#118404 = AXIS2_PLACEMENT_3D ( 'NONE', #45493, #97156, #46119 ) ;
#118405 = CARTESIAN_POINT ( 'NONE',  ( 4.349999999999939249, 2.500000000000000000, 2.511473670974873507 ) ) ;
#118406 = CARTESIAN_POINT ( 'NONE',  ( 0.1999999999999562961, 12.50000000000000000, 4.676537180435972552 ) ) ;
#118407 = CIRCLE ( 'NONE', #68224, 0.09999999999999982514 ) ;
#118408 = VECTOR ( 'NONE', #22089, 1000.000000000000000 ) ;
#118409 = CIRCLE ( 'NONE', #61990, 0.09999999999999982514 ) ;
#118410 = DIRECTION ( 'NONE',  ( 0.000000000000000000, 0.000000000000000000, 1.000000000000000000 ) ) ;
#118411 = ORIENTED_EDGE ( 'NONE', *, *, #70838, .F. ) ;
#118412 = CIRCLE ( 'NONE', #93377, 0.1000000000000002554 ) ;
#118413 = EDGE_LOOP ( 'NONE', ( #80304, #40803, #69763, #16909 ) ) ;
#118414 = ORIENTED_EDGE ( 'NONE', *, *, #70690, .F. ) ;
#118415 = ORIENTED_EDGE ( 'NONE', *, *, #749, .T. ) ;
#118416 = DIRECTION ( 'NONE',  ( -0.000000000000000000, 1.000000000000000000, -0.000000000000000000 ) ) ;
#118417 = DIRECTION ( 'NONE',  ( 0.000000000000000000, 0.000000000000000000, 1.000000000000000000 ) ) ;
#118418 = AXIS2_PLACEMENT_3D ( 'NONE', #47978, #8655, #36865 ) ;
#118419 = ORIENTED_EDGE ( 'NONE', *, *, #101435, .T. ) ;
#118420 = CARTESIAN_POINT ( 'NONE',  ( -10.65000000000000391, 2.500000000000000000, -2.511473670974873951 ) ) ;
#118421 = ADVANCED_FACE ( 'NONE', ( #8460 ), #89121, .T. ) ;
#118422 = FACE_OUTER_BOUND ( 'NONE', #43877, .T. ) ;
#118423 = CIRCLE ( 'NONE', #78737, 0.09999999999999982514 ) ;
#118424 = DIRECTION ( 'NONE',  ( 0.000000000000000000, 0.000000000000000000, 1.000000000000000000 ) ) ;
#118426 = EDGE_LOOP ( 'NONE', ( #72963, #22413, #2666, #106804 ) ) ;
#118425 = CARTESIAN_POINT ( 'NONE',  ( -3.750000000000025757, 2.500000000000000000, -2.957883832488653830 ) ) ;
#118427 = DIRECTION ( 'NONE',  ( 0.000000000000000000, 0.000000000000000000, -1.000000000000000000 ) ) ;
#118428 = EDGE_CURVE ( 'NONE', #109103, #54777, #99597, .T. ) ;
#118429 = CARTESIAN_POINT ( 'NONE',  ( 9.599999999999914380, 2.500000000000000000, 5.022947341949748790 ) ) ;
#118430 = ORIENTED_EDGE ( 'NONE', *, *, #74984, .T. ) ;
#118431 = VERTEX_POINT ( 'NONE', #108609 ) ;
#118432 = ORIENTED_EDGE ( 'NONE', *, *, #14187, .T. ) ;
#118433 = DIRECTION ( 'NONE',  ( 0.000000000000000000, -0.000000000000000000, 1.000000000000000000 ) ) ;
#118434 = EDGE_CURVE ( 'NONE', #86996, #80440, #82874, .T. ) ;
#118435 = EDGE_CURVE ( 'NONE', #72665, #2195, #87051, .T. ) ;
#118436 = EDGE_CURVE ( 'NONE', #87633, #63269, #32712, .T. ) ;
#118437 = DIRECTION ( 'NONE',  ( -0.000000000000000000, 1.000000000000000000, -0.000000000000000000 ) ) ;
#118438 = EDGE_CURVE ( 'NONE', #17267, #98189, #124716, .T. ) ;
#118439 = EDGE_LOOP ( 'NONE', ( #104573, #28880, #57017, #11771 ) ) ;
#118440 = DIRECTION ( 'NONE',  ( 0.000000000000000000, -0.9999939076577903929, 0.003490651415223739937 ) ) ;
#118441 = CARTESIAN_POINT ( 'NONE',  ( -12.29999999999999716, 2.500000000000000000, 0.3464101615137776813 ) ) ;
#118442 = LINE ( 'NONE', #108624, #108940 ) ;
#118443 = CARTESIAN_POINT ( 'NONE',  ( 6.649999999999931077, 2.500000000000000000, -6.495190528383302464 ) ) ;
#118444 = ADVANCED_FACE ( 'NONE', ( #101379 ), #11836, .T. ) ;
#118445 = ORIENTED_EDGE ( 'NONE', *, *, #10809, .F. ) ;
#118446 = EDGE_CURVE ( 'NONE', #33924, #36661, #41191, .T. ) ;
#118447 = CIRCLE ( 'NONE', #95471, 0.06509327318403745899 ) ;
#118448 = DIRECTION ( 'NONE',  ( 0.000000000000000000, 0.000000000000000000, -1.000000000000000000 ) ) ;
#118449 = EDGE_LOOP ( 'NONE', ( #27615, #2394, #40482, #104931 ) ) ;
#118450 = ORIENTED_EDGE ( 'NONE', *, *, #77740, .F. ) ;
#118451 = CARTESIAN_POINT ( 'NONE',  ( -0.4000000000000392131, 12.50000000000000000, -4.265033745738164406 ) ) ;
#118452 = CARTESIAN_POINT ( 'NONE',  ( 12.29999999999990301, 12.50000000000000000, -0.3464101615137782364 ) ) ;
#118453 = FACE_BOUND ( 'NONE', #9417, .T. ) ;
#118454 = DIRECTION ( 'NONE',  ( 0.000000000000000000, -0.000000000000000000, 1.000000000000000000 ) ) ;
#118455 = DIRECTION ( 'NONE',  ( 0.000000000000000000, 1.000000000000000000, 0.000000000000000000 ) ) ;
#118457 = VECTOR ( 'NONE', #29620, 1000.000000000000000 ) ;
#118456 = AXIS2_PLACEMENT_3D ( 'NONE', #45206, #15052, #24265 ) ;
#118458 = DIRECTION ( 'NONE',  ( -0.000000000000000000, 1.000000000000000000, -0.000000000000000000 ) ) ;
#118459 = VERTEX_POINT ( 'NONE', #12336 ) ;
#118460 = DIRECTION ( 'NONE',  ( 0.000000000000000000, 0.000000000000000000, -1.000000000000000000 ) ) ;
#118461 = FACE_OUTER_BOUND ( 'NONE', #104592, .T. ) ;
#118462 = CONICAL_SURFACE ( 'NONE', #55779, 0.09999999999999982514, 0.003490658503988666988 ) ;
#118463 = FACE_OUTER_BOUND ( 'NONE', #123991, .T. ) ;
#118464 = DIRECTION ( 'NONE',  ( 0.000000000000000000, 0.000000000000000000, 1.000000000000000000 ) ) ;
#118465 = ORIENTED_EDGE ( 'NONE', *, *, #34042, .F. ) ;
#118466 = CIRCLE ( 'NONE', #5581, 0.09999999999999982514 ) ;
#118467 = CARTESIAN_POINT ( 'NONE',  ( -7.900000000000014566, 2.500000000000000000, -4.430127018922202176 ) ) ;
#118468 = AXIS2_PLACEMENT_3D ( 'NONE', #6737, #129157, #36892 ) ;
#118469 = DIRECTION ( 'NONE',  ( 0.000000000000000000, 0.000000000000000000, -1.000000000000000000 ) ) ;
#118470 = ORIENTED_EDGE ( 'NONE', *, *, #120807, .T. ) ;
#118471 = ORIENTED_EDGE ( 'NONE', *, *, #27899, .F. ) ;
#118472 = PLANE ( 'NONE',  #14638 ) ;
#118473 = CARTESIAN_POINT ( 'NONE',  ( -10.65000000000000391, 12.50000000000000000, -2.511473670974873951 ) ) ;
#118474 = FACE_BOUND ( 'NONE', #53356, .T. ) ;
#118475 = CARTESIAN_POINT ( 'NONE',  ( 14.69205215198098102, -2.499999999999999112, -6.336420067969235959 ) ) ;
#118476 = ORIENTED_EDGE ( 'NONE', *, *, #39230, .F. ) ;
#118477 = FACE_OUTER_BOUND ( 'NONE', #69826, .T. ) ;
#118478 = ORIENTED_EDGE ( 'NONE', *, *, #86, .F. ) ;
#118479 = ORIENTED_EDGE ( 'NONE', *, *, #70316, .T. ) ;
#118480 = DIRECTION ( 'NONE',  ( -4.274815082592931898E-19, -0.9999939076577903929, -0.003490651415223739937 ) ) ;
#118481 = CARTESIAN_POINT ( 'NONE',  ( 185.6250000000000284, -8.891194145520236347, -1.633285867636356693E-15 ) ) ;
#118482 = CONICAL_SURFACE ( 'NONE', #1696, 0.1000000000000002554, 0.003490658503988666988 ) ;
#118483 = EDGE_LOOP ( 'NONE', ( #127237, #83665 ) ) ;
#118484 = DIRECTION ( 'NONE',  ( -0.000000000000000000, 1.000000000000000000, -0.000000000000000000 ) ) ;
#118485 = CONICAL_SURFACE ( 'NONE', #62080, 0.1000000000000002554, 0.003490658503988666988 ) ;
#118486 = CARTESIAN_POINT ( 'NONE',  ( 9.399999999999915090, 2.500000000000000000, 3.983716857408420964 ) ) ;
#118487 = ADVANCED_FACE ( 'NONE', ( #70621 ), #57828, .T. ) ;
#118488 = CIRCLE ( 'NONE', #95519, 0.09999999999999999167 ) ;
#118489 = DIRECTION ( 'NONE',  ( 0.000000000000000000, -0.000000000000000000, 1.000000000000000000 ) ) ;
#118490 = DIRECTION ( 'NONE',  ( 0.000000000000000000, 1.000000000000000000, 0.000000000000000000 ) ) ;
#118491 = CIRCLE ( 'NONE', #3487, 0.09999999999999982514 ) ;
#118492 = AXIS2_PLACEMENT_3D ( 'NONE', #9017, #31265, #48974 ) ;
#118493 = ORIENTED_EDGE ( 'NONE', *, *, #74247, .F. ) ;
#118494 = VECTOR ( 'NONE', #119245, 1000.000000000000000 ) ;
#118495 = FILL_AREA_STYLE ('',( #67436 ) ) ;
#118496 = DIRECTION ( 'NONE',  ( -4.274815082592931898E-19, -0.9999939076577903929, -0.003490651415223739937 ) ) ;
#118497 = DIRECTION ( 'NONE',  ( -0.000000000000000000, 1.000000000000000000, -0.000000000000000000 ) ) ;
#118498 = CARTESIAN_POINT ( 'NONE',  ( -7.900000000000014566, 12.50000000000000000, 0.7579135962115869374 ) ) ;
#118499 = ORIENTED_EDGE ( 'NONE', *, *, #40631, .T. ) ;
#118500 = CARTESIAN_POINT ( 'NONE',  ( -1.450000000000035039, 12.50000000000000000, -2.576566944158915184 ) ) ;
#118501 = EDGE_LOOP ( 'NONE', ( #64790, #111241, #110936, #37589 ) ) ;
#118502 = AXIS2_PLACEMENT_3D ( 'NONE', #73286, #3905, #13056 ) ;
#118503 = FACE_OUTER_BOUND ( 'NONE', #53233, .T. ) ;
#118504 = AXIS2_PLACEMENT_3D ( 'NONE', #74049, #123771, #45241 ) ;
#118505 = ORIENTED_EDGE ( 'NONE', *, *, #110620, .F. ) ;
#118506 = CARTESIAN_POINT ( 'NONE',  ( 0.8499999999999536815, 2.500000000000000000, 5.902370205355745192 ) ) ;
#118507 = CARTESIAN_POINT ( 'NONE',  ( 87.50000000000002842, -6.761363245278262823, -3.308765358479924590 ) ) ;
#118508 = DIRECTION ( 'NONE',  ( 0.000000000000000000, 1.000000000000000000, 0.000000000000000000 ) ) ;
#118510 = CONICAL_SURFACE ( 'NONE', #103858, 0.09999999999999982514, 0.003490658503988666988 ) ;
#118509 = VECTOR ( 'NONE', #91338, 1000.000000000000000 ) ;
#118511 = LINE ( 'NONE', #129016, #32032 ) ;
#118512 = VERTEX_POINT ( 'NONE', #81100 ) ;
#118513 = LINE ( 'NONE', #108052, #112329 ) ;
#118514 = DIRECTION ( 'NONE',  ( -0.000000000000000000, -1.000000000000000000, -0.000000000000000000 ) ) ;
#118515 = DIRECTION ( 'NONE',  ( 0.000000000000000000, 1.000000000000000000, 0.000000000000000000 ) ) ;
#118516 = DIRECTION ( 'NONE',  ( 0.000000000000000000, 0.000000000000000000, -1.000000000000000000 ) ) ;
#118517 = DIRECTION ( 'NONE',  ( 0.000000000000000000, 1.000000000000000000, 0.000000000000000000 ) ) ;
#118518 = PLANE ( 'NONE',  #55757 ) ;
#118519 = VERTEX_POINT ( 'NONE', #51643 ) ;
#118520 = EDGE_LOOP ( 'NONE', ( #103150, #30173 ) ) ;
#118521 = CARTESIAN_POINT ( 'NONE',  ( 13.74999999999989519, 12.50000000000000000, -2.922977105672691422 ) ) ;
#118522 = ORIENTED_EDGE ( 'NONE', *, *, #109077, .T. ) ;
#118523 = DIRECTION ( 'NONE',  ( -0.000000000000000000, -1.000000000000000000, -0.000000000000000000 ) ) ;
#118525 = ORIENTED_EDGE ( 'NONE', *, *, #7248, .T. ) ;
#118524 = ORIENTED_EDGE ( 'NONE', *, *, #92999, .T. ) ;
#118526 = VERTEX_POINT ( 'NONE', #102020 ) ;
#118527 = AXIS2_PLACEMENT_3D ( 'NONE', #46898, #48180, #107083 ) ;
#118528 = LINE ( 'NONE', #38722, #93882 ) ;
#118530 = EDGE_CURVE ( 'NONE', #119523, #28738, #2501, .T. ) ;
#118529 = DIRECTION ( 'NONE',  ( 0.000000000000000000, 0.000000000000000000, 1.000000000000000000 ) ) ;
#118531 = CARTESIAN_POINT ( 'NONE',  ( 10.19999999999991225, 2.500000000000000000, 3.883716857408420431 ) ) ;
#118532 = CARTESIAN_POINT ( 'NONE',  ( -8.750000000000005329, 12.50000000000000000, 5.802370205355744659 ) ) ;
#118533 = CARTESIAN_POINT ( 'NONE',  ( 185.9166666666666856, 6.668395609140176816, 3.850000000000000977 ) ) ;
#118534 = DIRECTION ( 'NONE',  ( -4.274815082592931898E-19, -0.9999939076577903929, -0.003490651415223739937 ) ) ;
#118535 = FACE_OUTER_BOUND ( 'NONE', #94392, .T. ) ;
#118536 = EDGE_CURVE ( 'NONE', #77736, #41455, #101735, .T. ) ;
#118537 = EDGE_CURVE ( 'NONE', #52488, #88829, #99692, .T. ) ;
#118538 = LINE ( 'NONE', #7289, #49796 ) ;
#118539 = EDGE_LOOP ( 'NONE', ( #58542, #128824 ) ) ;
#118541 = ORIENTED_EDGE ( 'NONE', *, *, #30251, .T. ) ;
#118540 = AXIS2_PLACEMENT_3D ( 'NONE', #57528, #56846, #17578 ) ;
#118542 = ORIENTED_EDGE ( 'NONE', *, *, #95975, .F. ) ;
#118543 = CIRCLE ( 'NONE', #20258, 0.1000000000000000472 ) ;
#118544 = EDGE_CURVE ( 'NONE', #91624, #103089, #109913, .T. ) ;
#118546 = EDGE_CURVE ( 'NONE', #66767, #83529, #71928, .T. ) ;
#118545 = CARTESIAN_POINT ( 'NONE',  ( 165.4999999999999716, 0.000000000000000000, -2.500000000000000000 ) ) ;
#118547 = ORIENTED_EDGE ( 'NONE', *, *, #48211, .T. ) ;
#118548 = VERTEX_POINT ( 'NONE', #49715 ) ;
#118549 = EDGE_CURVE ( 'NONE', #8339, #58961, #1467, .T. ) ;
#118550 = DIRECTION ( 'NONE',  ( -0.000000000000000000, 1.000000000000000000, -0.000000000000000000 ) ) ;
#118552 = CIRCLE ( 'NONE', #126883, 0.06509327318403745899 ) ;
#118551 = AXIS2_PLACEMENT_3D ( 'NONE', #8477, #66756, #48418 ) ;
#118553 = DIRECTION ( 'NONE',  ( 0.000000000000000000, 0.000000000000000000, -1.000000000000000000 ) ) ;
#118554 = DIRECTION ( 'NONE',  ( -4.274815082592931898E-19, -0.9999939076577903929, -0.003490651415223739937 ) ) ;
#118555 = FACE_OUTER_BOUND ( 'NONE', #115209, .T. ) ;
#118556 = FACE_OUTER_BOUND ( 'NONE', #56303, .T. ) ;
#118557 = ORIENTED_EDGE ( 'NONE', *, *, #84010, .T. ) ;
#118558 = CARTESIAN_POINT ( 'NONE',  ( 13.34999999999990017, 2.500000000000000000, 2.957883832488649389 ) ) ;
#118559 = CIRCLE ( 'NONE', #68382, 0.06509327318403745899 ) ;
#118560 = EDGE_LOOP ( 'NONE', ( #10325, #77222, #937, #1607 ) ) ;
#118561 = CARTESIAN_POINT ( 'NONE',  ( 1.699999999999951994, 12.50000000000000000, -0.06509327318403970719 ) ) ;
#118562 = CIRCLE ( 'NONE', #74756, 0.1000000000000002554 ) ;
#118563 = EDGE_LOOP ( 'NONE', ( #86661, #61314, #68788, #75227 ) ) ;
#118564 = DIRECTION ( 'NONE',  ( -0.000000000000000000, -1.000000000000000000, -0.000000000000000000 ) ) ;
#118565 = VERTEX_POINT ( 'NONE', #20238 ) ;
#118566 = VERTEX_POINT ( 'NONE', #50340 ) ;
#118567 = LINE ( 'NONE', #68828, #119261 ) ;
#118568 = CARTESIAN_POINT ( 'NONE',  ( -14.19999999999998685, 2.500000000000000000, -0.1000000000000001166 ) ) ;
#118569 = CARTESIAN_POINT ( 'NONE',  ( 13.34999999999989662, 2.500000000000000000, -1.372243186433550033 ) ) ;
#118570 = DIRECTION ( 'NONE',  ( 0.000000000000000000, 0.000000000000000000, 1.000000000000000000 ) ) ;
#118571 = CARTESIAN_POINT ( 'NONE',  ( 3.349999999999941025, 12.50000000000000000, 7.188010851410848723 ) ) ;
#118572 = EDGE_LOOP ( 'NONE', ( #39510, #42676 ) ) ;
#118573 = LINE ( 'NONE', #68837, #18595 ) ;
#118574 = CARTESIAN_POINT ( 'NONE',  ( -3.300000000000028244, 2.500000000000000000, 4.330127018922196314 ) ) ;
#118575 = DIRECTION ( 'NONE',  ( 0.000000000000000000, 0.000000000000000000, 1.000000000000000000 ) ) ;
#118576 = CARTESIAN_POINT ( 'NONE',  ( -9.600000000000006750, 2.500000000000000000, 5.022947341949748790 ) ) ;
#118577 = CIRCLE ( 'NONE', #3570, 0.09999999999999982514 ) ;
#118578 = CONICAL_SURFACE ( 'NONE', #24590, 0.09999999999999982514, 0.003490658503988666988 ) ;
#118579 = DIRECTION ( 'NONE',  ( 0.000000000000000000, 1.000000000000000000, 0.000000000000000000 ) ) ;
#118580 = ORIENTED_EDGE ( 'NONE', *, *, #42569, .T. ) ;
#118581 = AXIS2_PLACEMENT_3D ( 'NONE', #5568, #59880, #98460 ) ;
#118582 = ORIENTED_EDGE ( 'NONE', *, *, #110052, .T. ) ;
#118583 = EDGE_CURVE ( 'NONE', #96946, #41415, #110542, .T. ) ;
#118584 = DIRECTION ( 'NONE',  ( -0.000000000000000000, -1.000000000000000000, -0.000000000000000000 ) ) ;
#118585 = EDGE_CURVE ( 'NONE', #79172, #2432, #90241, .T. ) ;
#118586 = AXIS2_PLACEMENT_3D ( 'NONE', #90654, #989, #121402 ) ;
#118587 = EDGE_CURVE ( 'NONE', #13065, #92822, #78863, .T. ) ;
#118588 = ORIENTED_EDGE ( 'NONE', *, *, #73862, .T. ) ;
#118589 = CIRCLE ( 'NONE', #57967, 0.06509327318403745899 ) ;
#118590 = LINE ( 'NONE', #19763, #48749 ) ;
#118591 = CARTESIAN_POINT ( 'NONE',  ( 4.999999999999936939, 2.500000000000000000, -3.737306695894649700 ) ) ;
#118592 = AXIS2_PLACEMENT_3D ( 'NONE', #95868, #37603, #36323 ) ;
#118593 = AXIS2_PLACEMENT_3D ( 'NONE', #596, #60826, #110560 ) ;
#118594 = EDGE_CURVE ( 'NONE', #91624, #74274, #120610, .T. ) ;
#118595 = ORIENTED_EDGE ( 'NONE', *, *, #72742, .T. ) ;
#118596 = CARTESIAN_POINT ( 'NONE',  ( 184.3333333333333144, 6.668395609140177704, -3.849999999999998312 ) ) ;
#118598 = CIRCLE ( 'NONE', #70483, 0.1000000000000000472 ) ;
#118597 = DIRECTION ( 'NONE',  ( 0.000000000000000000, 1.000000000000000000, 0.000000000000000000 ) ) ;
#118599 = EDGE_CURVE ( 'NONE', #113021, #93976, #51000, .T. ) ;
#118600 = DIRECTION ( 'NONE',  ( 0.000000000000000000, 0.000000000000000000, 1.000000000000000000 ) ) ;
#118601 = DIRECTION ( 'NONE',  ( 0.000000000000000000, 1.000000000000000000, 0.000000000000000000 ) ) ;
#118602 = ORIENTED_EDGE ( 'NONE', *, *, #3917, .F. ) ;
#118603 = ADVANCED_FACE ( 'NONE', ( #22188 ), #121010, .T. ) ;
#118604 = EDGE_CURVE ( 'NONE', #84227, #87575, #32894, .T. ) ;
#118607 = ADVANCED_FACE ( 'NONE', ( #114405 ), #122657, .T. ) ;
#118606 = AXIS2_PLACEMENT_3D ( 'NONE', #114328, #2420, #52190 ) ;
#118605 = AXIS2_PLACEMENT_3D ( 'NONE', #72992, #112914, #23234 ) ;
#118608 = DIRECTION ( 'NONE',  ( 0.000000000000000000, 0.000000000000000000, -1.000000000000000000 ) ) ;
#118609 = EDGE_LOOP ( 'NONE', ( #124673, #66918 ) ) ;
#118610 =( BOUNDED_CURVE ( )  B_SPLINE_CURVE ( 2, ( #126810, #48244, #107151, #88139, #128098, #17475, #38446 ),
 .UNSPECIFIED., .F., .F. ) 
 B_SPLINE_CURVE_WITH_KNOTS ( ( 3, 2, 2, 3 ),
 ( 0.5714285714285719520, 0.5952380952380957879, 0.6190476190476195129, 0.6428571428571433488 ),
 .UNSPECIFIED. ) 
 CURVE ( )  GEOMETRIC_REPRESENTATION_ITEM ( )  RATIONAL_B_SPLINE_CURVE ( ( 0.9999999999999968914, 0.8660254037844418162, 1.000000000000000000, 0.8660254037844387076, 1.000000000000000000, 0.8660254037844361541, 1.000000000000002442 ) ) 
 REPRESENTATION_ITEM ( '' )  );
#118611 = DIRECTION ( 'NONE',  ( -0.000000000000000000, 1.000000000000000000, -0.000000000000000000 ) ) ;
#118612 = DIRECTION ( 'NONE',  ( 0.000000000000000000, -0.9999939076577903929, 0.003490651415223739937 ) ) ;
#118613 = EDGE_CURVE ( 'NONE', #6029, #41590, #13622, .T. ) ;
#118614 = CARTESIAN_POINT ( 'NONE',  ( 11.89999999999990798, 2.500000000000000000, -4.676537180435977881 ) ) ;
#118615 = ORIENTED_EDGE ( 'NONE', *, *, #70981, .T. ) ;
#118616 = DIRECTION ( 'NONE',  ( 0.000000000000000000, 0.000000000000000000, 1.000000000000000000 ) ) ;
#118617 = VERTEX_POINT ( 'NONE', #113116 ) ;
#118618 = CARTESIAN_POINT ( 'NONE',  ( -2.700000000000030376, 12.50000000000000000, 3.918623584224383727 ) ) ;
#118619 = CARTESIAN_POINT ( 'NONE',  ( -8.100000000000010303, 2.500000000000000000, 4.083716857408421497 ) ) ;
#118620 = AXIS2_PLACEMENT_3D ( 'NONE', #115764, #66022, #56192 ) ;
#118621 = CARTESIAN_POINT ( 'NONE',  ( 1.449999999999951772, 2.500000000000000000, -6.048780366869526581 ) ) ;
#118622 = VERTEX_POINT ( 'NONE', #17304 ) ;
#118623 = CARTESIAN_POINT ( 'NONE',  ( 8.749999999999957367, 2.500000000000000000, -6.395190528383301931 ) ) ;
#118624 = CARTESIAN_POINT ( 'NONE',  ( 185.4479166673494603, -6.668395609140176816, -3.850000000000003642 ) ) ;
#118625 = ORIENTED_EDGE ( 'NONE', *, *, #81203, .T. ) ;
#118626 = CARTESIAN_POINT ( 'NONE',  ( -10.20000000000000462, 2.500000000000000000, 0.3464101615137735735 ) ) ;
#118627 = ORIENTED_EDGE ( 'NONE', *, *, #82565, .T. ) ;
#118628 = DIRECTION ( 'NONE',  ( 0.000000000000000000, 1.000000000000000000, 0.000000000000000000 ) ) ;
#118629 = AXIS2_PLACEMENT_3D ( 'NONE', #68956, #89243, #57205 ) ;
#118630 = VECTOR ( 'NONE', #35551, 1000.000000000000000 ) ;
#118631 = ORIENTED_EDGE ( 'NONE', *, *, #67383, .F. ) ;
#118632 = CARTESIAN_POINT ( 'NONE',  ( 2.299999999999948752, 12.50000000000000000, 0.3464101615137735735 ) ) ;
#118633 = DIRECTION ( 'NONE',  ( 0.000000000000000000, 0.000000000000000000, 1.000000000000000000 ) ) ;
#118634 = ORIENTED_EDGE ( 'NONE', *, *, #76940, .T. ) ;
#118635 = ORIENTED_EDGE ( 'NONE', *, *, #84580, .F. ) ;
#118636 = DIRECTION ( 'NONE',  ( 0.000000000000000000, 0.000000000000000000, -1.000000000000000000 ) ) ;
#118637 = CARTESIAN_POINT ( 'NONE',  ( 11.64999999999990798, 12.50000000000000000, 7.188010851410848723 ) ) ;
#118638 = VERTEX_POINT ( 'NONE', #127304 ) ;
#118639 = CIRCLE ( 'NONE', #99782, 8.199999999999999289 ) ;
#118640 = DIRECTION ( 'NONE',  ( 0.000000000000000000, 0.000000000000000000, -1.000000000000000000 ) ) ;
#118641 = AXIS2_PLACEMENT_3D ( 'NONE', #20511, #90521, #40811 ) ;
#118642 = EDGE_CURVE ( 'NONE', #90643, #18500, #11935, .T. ) ;
#118643 = AXIS2_PLACEMENT_3D ( 'NONE', #102278, #42067, #121913 ) ;
#118644 = DIRECTION ( 'NONE',  ( -0.000000000000000000, -1.000000000000000000, -0.000000000000000000 ) ) ;
#118645 = DIRECTION ( 'NONE',  ( 0.000000000000000000, 1.000000000000000000, 0.000000000000000000 ) ) ;
#118646 = DIRECTION ( 'NONE',  ( 0.000000000000000000, 0.000000000000000000, 1.000000000000000000 ) ) ;
#118647 = DIRECTION ( 'NONE',  ( -0.000000000000000000, 1.000000000000000000, -0.000000000000000000 ) ) ;
#118648 = CARTESIAN_POINT ( 'NONE',  ( 3.299999999999942979, 2.500000000000000000, 4.330127018922196314 ) ) ;
#118649 = VERTEX_POINT ( 'NONE', #102650 ) ;
#118650 = ORIENTED_EDGE ( 'NONE', *, *, #21456, .F. ) ;
#118651 = ORIENTED_EDGE ( 'NONE', *, *, #12295, .F. ) ;
#118652 = ORIENTED_EDGE ( 'NONE', *, *, #46817, .F. ) ;
#118653 = DIRECTION ( 'NONE',  ( -0.000000000000000000, 1.000000000000000000, -0.000000000000000000 ) ) ;
#118654 = CARTESIAN_POINT ( 'NONE',  ( 2.299999999999946976, 12.50000000000000000, 4.741630453620009789 ) ) ;
#118655 = AXIS2_PLACEMENT_3D ( 'NONE', #72236, #90562, #121968 ) ;
#118656 = DIRECTION ( 'NONE',  ( -0.000000000000000000, -1.000000000000000000, -0.000000000000000000 ) ) ;
#118657 = VERTEX_POINT ( 'NONE', #3813 ) ;
#118658 = EDGE_CURVE ( 'NONE', #89337, #40173, #57269, .T. ) ;
#118659 = FACE_BOUND ( 'NONE', #51213, .T. ) ;
#118660 = ORIENTED_EDGE ( 'NONE', *, *, #20089, .F. ) ;
#118661 = DIRECTION ( 'NONE',  ( 0.000000000000000000, -0.9999939076577903929, 0.003490651415223739937 ) ) ;
#118662 = CARTESIAN_POINT ( 'NONE',  ( -15.19999999999998153, 2.500000000000000000, -0.4464101615137759382 ) ) ;
#118663 = DIRECTION ( 'NONE',  ( 0.000000000000000000, -0.000000000000000000, 1.000000000000000000 ) ) ;
#118664 = AXIS2_PLACEMENT_3D ( 'NONE', #129119, #60376, #100278 ) ;
#118665 = CARTESIAN_POINT ( 'NONE',  ( 129.5000000000000000, 1.500000000000000000, 2.598076211353316900 ) ) ;
#118666 = CARTESIAN_POINT ( 'NONE',  ( -13.94999999999998863, 12.50000000000000000, -1.883746621131361376 ) ) ;
#118667 = CARTESIAN_POINT ( 'NONE',  ( 3.749999999999944045, 12.50000000000000000, -7.122917578226816815 ) ) ;
#118668 = ORIENTED_EDGE ( 'NONE', *, *, #90177, .T. ) ;
#118669 = FACE_OUTER_BOUND ( 'NONE', #125539, .T. ) ;
#118670 = CARTESIAN_POINT ( 'NONE',  ( -6.700000000000019718, 2.500000000000000000, -4.230127018922201998 ) ) ;
#118671 = CIRCLE ( 'NONE', #89344, 7.700000000000000178 ) ;
#118672 = CIRCLE ( 'NONE', #81037, 0.09999999999999982514 ) ;
#118673 = CARTESIAN_POINT ( 'NONE',  ( 10.84999999999991260, 2.500000000000000000, -2.857883832488653741 ) ) ;
#118674 = ORIENTED_EDGE ( 'NONE', *, *, #92723, .T. ) ;
#118676 = ORIENTED_EDGE ( 'NONE', *, *, #52356, .T. ) ;
#118675 = CIRCLE ( 'NONE', #70655, 8.699999999999999289 ) ;
#118677 = EDGE_LOOP ( 'NONE', ( #97035, #112290 ) ) ;
#118678 = ORIENTED_EDGE ( 'NONE', *, *, #11133, .F. ) ;
#118679 = CARTESIAN_POINT ( 'NONE',  ( 12.69999999999990159, 12.50000000000000000, -3.983716857408426293 ) ) ;
#118680 = DIRECTION ( 'NONE',  ( -1.000000000000000000, 0.000000000000000000, 0.000000000000000000 ) ) ;
#118682 = ORIENTED_EDGE ( 'NONE', *, *, #8213, .T. ) ;
#118681 = ORIENTED_EDGE ( 'NONE', *, *, #23538, .F. ) ;
#118684 = VERTEX_POINT ( 'NONE', #27156 ) ;
#118683 = AXIS2_PLACEMENT_3D ( 'NONE', #95173, #5480, #115421 ) ;
#118686 = AXIS2_PLACEMENT_3D ( 'NONE', #38353, #39017, #77602 ) ;
#118685 = DIRECTION ( 'NONE',  ( 0.000000000000000000, 0.000000000000000000, -1.000000000000000000 ) ) ;
#118687 = CIRCLE ( 'NONE', #5798, 0.09999999999999982514 ) ;
#118688 = ADVANCED_FACE ( 'NONE', ( #53565 ), #85093, .T. ) ;
#118689 = DIRECTION ( 'NONE',  ( -4.274815082592931898E-19, -0.9999939076577903929, -0.003490651415223739937 ) ) ;
#118690 = CARTESIAN_POINT ( 'NONE',  ( 2.099999999999949463, 12.50000000000000000, -3.637306695894650055 ) ) ;
#118691 = DIRECTION ( 'NONE',  ( 0.000000000000000000, 0.000000000000000000, -1.000000000000000000 ) ) ;
#118692 = DIRECTION ( 'NONE',  ( 0.000000000000000000, 0.000000000000000000, 1.000000000000000000 ) ) ;
#118693 = CARTESIAN_POINT ( 'NONE',  ( 8.099999999999921485, 2.500000000000000000, 0.3464101615137735735 ) ) ;
#118694 = CARTESIAN_POINT ( 'NONE',  ( -6.650000000000019007, 2.500000000000000000, -1.472243186433550122 ) ) ;
#118695 = CIRCLE ( 'NONE', #95721, 0.09999999999999982514 ) ;
#118696 = VERTEX_POINT ( 'NONE', #4423 ) ;
#118697 = EDGE_CURVE ( 'NONE', #101221, #60915, #64163, .T. ) ;
#118698 = DIRECTION ( 'NONE',  ( 0.000000000000000000, 0.000000000000000000, 1.000000000000000000 ) ) ;
#118699 = EDGE_LOOP ( 'NONE', ( #7868, #38611 ) ) ;
#118700 = AXIS2_PLACEMENT_3D ( 'NONE', #90010, #110316, #59301 ) ;
#118701 = ORIENTED_EDGE ( 'NONE', *, *, #62355, .F. ) ;
#118702 = VERTEX_POINT ( 'NONE', #92854 ) ;
#118703 = EDGE_CURVE ( 'NONE', #50242, #13848, #26520, .T. ) ;
#118705 = ADVANCED_FACE ( 'NONE', ( #43125 ), #7508, .T. ) ;
#118704 = FACE_OUTER_BOUND ( 'NONE', #28881, .T. ) ;
#118707 = ORIENTED_EDGE ( 'NONE', *, *, #79246, .T. ) ;
#118706 = EDGE_CURVE ( 'NONE', #62255, #10677, #95570, .T. ) ;
#118708 = EDGE_CURVE ( 'NONE', #41901, #70057, #32800, .T. ) ;
#118710 = ORIENTED_EDGE ( 'NONE', *, *, #21028, .T. ) ;
#118709 = EDGE_CURVE ( 'NONE', #55123, #85856, #45400, .T. ) ;
#118711 = CARTESIAN_POINT ( 'NONE',  ( -2.100000000000034284, 2.500000000000000000, -0.1000000000000023925 ) ) ;
#118712 = DIRECTION ( 'NONE',  ( 0.000000000000000000, -0.000000000000000000, 1.000000000000000000 ) ) ;
#118713 = DIRECTION ( 'NONE',  ( 0.000000000000000000, 0.000000000000000000, 1.000000000000000000 ) ) ;
#118714 = CARTESIAN_POINT ( 'NONE',  ( -8.749999999999976907, 2.500000000000000000, -6.495190528383297135 ) ) ;
#118715 = CARTESIAN_POINT ( 'NONE',  ( -1.650000000000034772, 2.500000000000000000, 1.472243186433545459 ) ) ;
#118716 = EDGE_CURVE ( 'NONE', #47149, #120218, #129045, .T. ) ;
#118717 = VERTEX_POINT ( 'NONE', #16665 ) ;
#118718 = CARTESIAN_POINT ( 'NONE',  ( -4.800000000000024691, 2.500000000000000000, 4.776537180435972196 ) ) ;
#118719 = ADVANCED_FACE ( 'NONE', ( #123573 ), #34587, .T. ) ;
#118720 = ADVANCED_FACE ( 'NONE', ( #73843 ), #105937, .T. ) ;
#118721 = ORIENTED_EDGE ( 'NONE', *, *, #49464, .F. ) ;
#118722 = DIRECTION ( 'NONE',  ( 0.000000000000000000, 0.000000000000000000, 1.000000000000000000 ) ) ;
#118723 = ORIENTED_EDGE ( 'NONE', *, *, #30089, .T. ) ;
#118724 = CARTESIAN_POINT ( 'NONE',  ( 1.049999999999953637, 2.500000000000000000, -1.718653347947326049 ) ) ;
#118725 = DIRECTION ( 'NONE',  ( 0.000000000000000000, 1.000000000000000000, 0.000000000000000000 ) ) ;
#118726 = EDGE_LOOP ( 'NONE', ( #70816, #101398, #67072, #72244 ) ) ;
#118728 = AXIS2_PLACEMENT_3D ( 'NONE', #73742, #24023, #14804 ) ;
#118727 = DIRECTION ( 'NONE',  ( 0.000000000000000000, 0.000000000000000000, -1.000000000000000000 ) ) ;
#118729 = LINE ( 'NONE', #59185, #74996 ) ;
#118730 = ORIENTED_EDGE ( 'NONE', *, *, #87616, .F. ) ;
#118731 = VECTOR ( 'NONE', #5998, 1000.000000000000000 ) ;
#118732 = AXIS2_PLACEMENT_3D ( 'NONE', #96369, #6683, #9942 ) ;
#118733 = CARTESIAN_POINT ( 'NONE',  ( -9.150000000000005684, 12.50000000000000000, 6.430097255199259010 ) ) ;
#118734 = ORIENTED_EDGE ( 'NONE', *, *, #30650, .T. ) ;
#118735 = EDGE_LOOP ( 'NONE', ( #89199, #128845, #98678, #79237 ) ) ;
#118736 = CARTESIAN_POINT ( 'NONE',  ( 6.899999999999928413, 2.500000000000000000, -3.983716857408426293 ) ) ;
#118737 = PLANE ( 'NONE',  #43015 ) ;
#118738 = CARTESIAN_POINT ( 'NONE',  ( -6.250000000000019540, 2.500000000000000000, -7.288010851410854585 ) ) ;
#118739 = CARTESIAN_POINT ( 'NONE',  ( -12.94999999999999218, 12.50000000000000000, 2.165063509461101265 ) ) ;
#118740 = CIRCLE ( 'NONE', #60178, 0.1000000000000002554 ) ;
#118741 = PLANE ( 'NONE',  #52029 ) ;
#118742 = AXIS2_PLACEMENT_3D ( 'NONE', #23593, #121785, #43900 ) ;
#118743 = ORIENTED_EDGE ( 'NONE', *, *, #63912, .T. ) ;
#118744 = DIRECTION ( 'NONE',  ( 0.000000000000000000, 0.000000000000000000, 1.000000000000000000 ) ) ;
#118745 = EDGE_CURVE ( 'NONE', #17419, #27445, #103884, .T. ) ;
#118746 = ORIENTED_EDGE ( 'NONE', *, *, #25025, .F. ) ;
#118747 = CARTESIAN_POINT ( 'NONE',  ( 5.649999999999934630, 2.500000000000000000, -2.411473670974877859 ) ) ;
#118749 = CIRCLE ( 'NONE', #122963, 0.06509327318403745899 ) ;
#118748 = DIRECTION ( 'NONE',  ( 0.000000000000000000, 0.000000000000000000, -1.000000000000000000 ) ) ;
#118750 = ADVANCED_FACE ( 'NONE', ( #116816 ), #30748, .T. ) ;
#118751 = EDGE_LOOP ( 'NONE', ( #42095, #13408, #100209, #15172 ) ) ;
#118752 = DIRECTION ( 'NONE',  ( 0.000000000000000000, 0.000000000000000000, -1.000000000000000000 ) ) ;
#118753 = DIRECTION ( 'NONE',  ( 0.000000000000000000, 0.000000000000000000, -1.000000000000000000 ) ) ;
#118754 = CARTESIAN_POINT ( 'NONE',  ( -6.650000000000018119, 12.50000000000000000, -6.495190528383302464 ) ) ;
#118755 = EDGE_CURVE ( 'NONE', #114828, #114625, #97624, .T. ) ;
#118756 = CARTESIAN_POINT ( 'NONE',  ( -8.750000000000010658, 2.500000000000000000, -1.472243186433550122 ) ) ;
#118757 = CARTESIAN_POINT ( 'NONE',  ( -5.650000000000019895, 2.500000000000000000, 1.818653347947321475 ) ) ;
#118758 = VERTEX_POINT ( 'NONE', #40876 ) ;
#118759 = ADVANCED_FACE ( 'NONE', ( #29114 ), #108291, .T. ) ;
#118760 = VECTOR ( 'NONE', #81075, 1000.000000000000000 ) ;
#118761 = CARTESIAN_POINT ( 'NONE',  ( 0.1999999999999627909, 2.500000000000000000, 0.3464101615137758494 ) ) ;
#118762 = EDGE_CURVE ( 'NONE', #28400, #43992, #66221, .T. ) ;
#118763 = CARTESIAN_POINT ( 'NONE',  ( -1.250000000000001554, 12.50000000000000000, 2.230156782645134950 ) ) ;
#118764 = DIRECTION ( 'NONE',  ( -0.000000000000000000, -1.000000000000000000, -0.000000000000000000 ) ) ;
#118765 = AXIS2_PLACEMENT_3D ( 'NONE', #121275, #23729, #32922 ) ;
#118766 = VECTOR ( 'NONE', #49985, 1000.000000000000000 ) ;
#118767 = ORIENTED_EDGE ( 'NONE', *, *, #3386, .T. ) ;
#118768 = CIRCLE ( 'NONE', #76911, 0.06509327318403745899 ) ;
#118769 = EDGE_CURVE ( 'NONE', #79642, #8138, #118543, .T. ) ;
#118770 = DIRECTION ( 'NONE',  ( -0.000000000000000000, 1.000000000000000000, -0.000000000000000000 ) ) ;
#118771 = AXIS2_PLACEMENT_3D ( 'NONE', #51174, #21707, #10570 ) ;
#118772 = ORIENTED_EDGE ( 'NONE', *, *, #102587, .T. ) ;
#118773 = EDGE_LOOP ( 'NONE', ( #21924, #21033 ) ) ;
#118774 = DIRECTION ( 'NONE',  ( 0.000000000000000000, 0.000000000000000000, 1.000000000000000000 ) ) ;
#118775 = VECTOR ( 'NONE', #24351, 1000.000000000000000 ) ;
#118776 = EDGE_LOOP ( 'NONE', ( #126802, #121887, #3966, #71922 ) ) ;
#118777 = PLANE ( 'NONE',  #100926 ) ;
#118778 = CARTESIAN_POINT ( 'NONE',  ( -2.900000000000029221, 2.500000000000000000, -2.276824562219559311E-15 ) ) ;
#118779 = VERTEX_POINT ( 'NONE', #58567 ) ;
#118780 = DIRECTION ( 'NONE',  ( 0.000000000000000000, 0.000000000000000000, 1.000000000000000000 ) ) ;
#118782 = EDGE_LOOP ( 'NONE', ( #66408, #22345 ) ) ;
#118781 = DIRECTION ( 'NONE',  ( 0.000000000000000000, 0.000000000000000000, -1.000000000000000000 ) ) ;
#118783 = DIRECTION ( 'NONE',  ( -4.274815082592931898E-19, -0.9999939076577903929, -0.003490651415223739937 ) ) ;
#118784 = CONICAL_SURFACE ( 'NONE', #81146, 0.09999999999999982514, 0.003490658503988666988 ) ;
#118785 = LINE ( 'NONE', #17341, #101146 ) ;
#118786 = EDGE_CURVE ( 'NONE', #46382, #38829, #89937, .T. ) ;
#118787 = ORIENTED_EDGE ( 'NONE', *, *, #95679, .T. ) ;
#118789 = CIRCLE ( 'NONE', #91606, 0.1000000000000002554 ) ;
#118788 = AXIS2_PLACEMENT_3D ( 'NONE', #34219, #14542, #54477 ) ;
#118790 = ORIENTED_EDGE ( 'NONE', *, *, #41618, .T. ) ;
#118791 = ORIENTED_EDGE ( 'NONE', *, *, #100856, .F. ) ;
#118792 = DIRECTION ( 'NONE',  ( -0.000000000000000000, 1.000000000000000000, -0.000000000000000000 ) ) ;
#118793 = DIRECTION ( 'NONE',  ( 0.000000000000000000, 1.000000000000000000, 0.000000000000000000 ) ) ;
#118794 = DIRECTION ( 'NONE',  ( -0.000000000000000000, 1.000000000000000000, -0.000000000000000000 ) ) ;
#118795 = FACE_BOUND ( 'NONE', #63992, .T. ) ;
#118796 = ORIENTED_EDGE ( 'NONE', *, *, #71257, .T. ) ;
#118797 = LINE ( 'NONE', #119430, #51191 ) ;
#118798 = DIRECTION ( 'NONE',  ( 0.000000000000000000, 0.000000000000000000, -1.000000000000000000 ) ) ;
#118799 = ORIENTED_EDGE ( 'NONE', *, *, #64602, .T. ) ;
#118800 = CARTESIAN_POINT ( 'NONE',  ( 1.249999999999988454, 2.500000000000000000, -2.065063509461102065 ) ) ;
#118801 = CARTESIAN_POINT ( 'NONE',  ( -11.25000000000000000, 2.500000000000000000, 2.757883832488649656 ) ) ;
#118802 = EDGE_CURVE ( 'NONE', #72180, #97645, #39159, .T. ) ;
#118803 = DIRECTION ( 'NONE',  ( 0.000000000000000000, 1.000000000000000000, 0.000000000000000000 ) ) ;
#118804 = DIRECTION ( 'NONE',  ( 0.000000000000000000, 0.000000000000000000, -1.000000000000000000 ) ) ;
#118805 = CIRCLE ( 'NONE', #62392, 0.1000000000000002554 ) ;
#118806 = FACE_OUTER_BOUND ( 'NONE', #81067, .T. ) ;
#118807 = DIRECTION ( 'NONE',  ( 0.000000000000000000, -0.000000000000000000, 1.000000000000000000 ) ) ;
#118808 = DIRECTION ( 'NONE',  ( 0.000000000000000000, 0.000000000000000000, -1.000000000000000000 ) ) ;
#118809 = AXIS2_PLACEMENT_3D ( 'NONE', #24256, #61618, #91062 ) ;
#118810 = VECTOR ( 'NONE', #27764, 1000.000000000000000 ) ;
#118811 = VERTEX_POINT ( 'NONE', #120055 ) ;
#118812 = EDGE_LOOP ( 'NONE', ( #114911, #45729 ) ) ;
#118813 = VERTEX_POINT ( 'NONE', #68363 ) ;
#118814 = CONICAL_SURFACE ( 'NONE', #114598, 0.1000000000000002554, 0.003490658503988666988 ) ;
#118815 = AXIS2_PLACEMENT_3D ( 'NONE', #22924, #47081, #45145 ) ;
#118816 = ORIENTED_EDGE ( 'NONE', *, *, #15756, .F. ) ;
#118817 = VERTEX_POINT ( 'NONE', #99130 ) ;
#118818 = FACE_OUTER_BOUND ( 'NONE', #74033, .T. ) ;
#118819 = DIRECTION ( 'NONE',  ( -0.000000000000000000, -1.000000000000000000, -0.000000000000000000 ) ) ;
#118820 = ORIENTED_EDGE ( 'NONE', *, *, #94927, .T. ) ;
#118821 = ADVANCED_FACE ( 'NONE', ( #80787 ), #110145, .T. ) ;
#118822 = FACE_BOUND ( 'NONE', #65979, .T. ) ;
#118823 = DIRECTION ( 'NONE',  ( -4.274815082592931898E-19, -0.9999939076577903929, -0.003490651415223739937 ) ) ;
#118824 = AXIS2_PLACEMENT_3D ( 'NONE', #66201, #77957, #117213 ) ;
#118825 = AXIS2_PLACEMENT_3D ( 'NONE', #97616, #117890, #87782 ) ;
#118826 = DIRECTION ( 'NONE',  ( 0.000000000000000000, 0.000000000000000000, -1.000000000000000000 ) ) ;
#118827 = CARTESIAN_POINT ( 'NONE',  ( -7.950000000000016165, 2.500000000000000000, -6.395190528383296602 ) ) ;
#118828 = CARTESIAN_POINT ( 'NONE',  ( 3.949999999999940670, 2.500000000000000000, 1.918653347947321564 ) ) ;
#118829 = DIRECTION ( 'NONE',  ( 0.000000000000000000, 0.000000000000000000, 1.000000000000000000 ) ) ;
#118830 = EDGE_LOOP ( 'NONE', ( #85198, #3911 ) ) ;
#118831 = AXIS2_PLACEMENT_3D ( 'NONE', #94802, #88845, #59415 ) ;
#118832 = VERTEX_POINT ( 'NONE', #98457 ) ;
#118833 = ORIENTED_EDGE ( 'NONE', *, *, #2286, .F. ) ;
#118834 = EDGE_LOOP ( 'NONE', ( #84090, #13513 ) ) ;
#118835 = DIRECTION ( 'NONE',  ( -0.000000000000000000, 1.000000000000000000, -0.000000000000000000 ) ) ;
#118836 = CARTESIAN_POINT ( 'NONE',  ( 115.5000000000000000, 5.000000000000000000, 5.000000000000003553 ) ) ;
#118837 = CARTESIAN_POINT ( 'NONE',  ( 4.149999999999939959, 2.500000000000000000, 2.857883832488649301 ) ) ;
#118838 = ORIENTED_EDGE ( 'NONE', *, *, #17308, .F. ) ;
#118839 = DIRECTION ( 'NONE',  ( 0.000000000000000000, 0.000000000000000000, 1.000000000000000000 ) ) ;
#118840 = AXIS2_PLACEMENT_3D ( 'NONE', #85665, #125579, #87591 ) ;
#118841 = DIRECTION ( 'NONE',  ( -0.000000000000000000, 1.000000000000000000, -0.000000000000000000 ) ) ;
#118842 = ADVANCED_FACE ( 'NONE', ( #69657 ), #19928, .T. ) ;
#118843 = CARTESIAN_POINT ( 'NONE',  ( 2.049999999999950084, 2.500000000000000000, -6.495190528383302464 ) ) ;
#118844 = AXIS2_PLACEMENT_3D ( 'NONE', #107572, #48654, #88563 ) ;
#118845 = CARTESIAN_POINT ( 'NONE',  ( 184.4427083336747160, -6.551208109652278289, 3.782341765624995134 ) ) ;
#118846 = CARTESIAN_POINT ( 'NONE',  ( 7.099999999999928590, 2.500000000000000000, 4.330127018922196314 ) ) ;
#118847 = DIRECTION ( 'NONE',  ( -0.000000000000000000, -1.000000000000000000, -0.000000000000000000 ) ) ;
#118848 = CIRCLE ( 'NONE', #54015, 0.06509327318403743123 ) ;
#118849 = CARTESIAN_POINT ( 'NONE',  ( -5.650000000000019895, 2.500000000000000000, 6.048780366869520364 ) ) ;
#118850 = VERTEX_POINT ( 'NONE', #38278 ) ;
#118851 = CARTESIAN_POINT ( 'NONE',  ( -13.34999999999999076, 2.500000000000000000, 2.857883832488652853 ) ) ;
#118852 = ADVANCED_FACE ( 'NONE', ( #109595 ), #8792, .T. ) ;
#118853 = AXIS2_PLACEMENT_3D ( 'NONE', #117743, #97482, #126951 ) ;
#118854 = VERTEX_POINT ( 'NONE', #48745 ) ;
#118855 = ORIENTED_EDGE ( 'NONE', *, *, #59570, .F. ) ;
#118856 = FACE_OUTER_BOUND ( 'NONE', #116742, .T. ) ;
#118857 = ADVANCED_FACE ( 'NONE', ( #59873 ), #99774, .T. ) ;
#118858 = DIRECTION ( 'NONE',  ( 0.000000000000000000, -0.9999939076577903929, 0.003490651415223739937 ) ) ;
#118860 = EDGE_CURVE ( 'NONE', #58034, #69008, #80131, .T. ) ;
#118859 = DIRECTION ( 'NONE',  ( -0.000000000000000000, 1.000000000000000000, -0.000000000000000000 ) ) ;
#118861 = EDGE_CURVE ( 'NONE', #85654, #116200, #40210, .T. ) ;
#118862 = EDGE_CURVE ( 'NONE', #22575, #75000, #16210, .T. ) ;
#118863 = ORIENTED_EDGE ( 'NONE', *, *, #6973, .F. ) ;
#118864 = CONICAL_SURFACE ( 'NONE', #89525, 0.1000000000000000472, 0.003490658503988666988 ) ;
#118865 = EDGE_LOOP ( 'NONE', ( #37162, #1414 ) ) ;
#118866 = DIRECTION ( 'NONE',  ( 0.000000000000000000, 0.000000000000000000, -1.000000000000000000 ) ) ;
#118867 = AXIS2_PLACEMENT_3D ( 'NONE', #26212, #66125, #119103 ) ;
#118868 = CARTESIAN_POINT ( 'NONE',  ( 3.349999999999944578, 12.50000000000000000, -1.537336459617587581 ) ) ;
#118869 = ADVANCED_FACE ( 'NONE', ( #78860 ), #60079, .T. ) ;
#118870 = DIRECTION ( 'NONE',  ( 0.000000000000000000, 0.000000000000000000, -1.000000000000000000 ) ) ;
#118871 = EDGE_LOOP ( 'NONE', ( #23432, #104368, #64268, #99799 ) ) ;
#118872 = EDGE_CURVE ( 'NONE', #35274, #86441, #106122, .T. ) ;
#118873 = CARTESIAN_POINT ( 'NONE',  ( 9.999999999999914735, 12.50000000000000000, 0.7579135962115869374 ) ) ;
#118874 = AXIS2_PLACEMENT_3D ( 'NONE', #44622, #102881, #34825 ) ;
#118875 = EDGE_CURVE ( 'NONE', #27907, #44544, #41298, .T. ) ;
#118876 = VERTEX_POINT ( 'NONE', #110858 ) ;
#118877 = DIRECTION ( 'NONE',  ( -4.274815082592931898E-19, -0.9999939076577903929, -0.003490651415223739937 ) ) ;
#118878 = EDGE_CURVE ( 'NONE', #109309, #118684, #91237, .T. ) ;
#118879 = EDGE_CURVE ( 'NONE', #42202, #4198, #93512, .T. ) ;
#118880 = VERTEX_POINT ( 'NONE', #13302 ) ;
#118881 = CARTESIAN_POINT ( 'NONE',  ( -11.25000000000000178, 2.500000000000000000, -5.802370205355746435 ) ) ;
#118882 = CONICAL_SURFACE ( 'NONE', #108693, 0.1000000000000002554, 0.003490658503988666988 ) ;
#118883 = CARTESIAN_POINT ( 'NONE',  ( 12.04999999999990479, 2.500000000000000000, -6.595190528383302109 ) ) ;
#118884 = CARTESIAN_POINT ( 'NONE',  ( 4.149999999999941735, 2.500000000000000000, -2.957883832488653830 ) ) ;
#118885 = AXIS2_PLACEMENT_3D ( 'NONE', #57981, #57329, #118175 ) ;
#118887 = EDGE_CURVE ( 'NONE', #80402, #122002, #101923, .T. ) ;
#118886 = DIRECTION ( 'NONE',  ( -0.000000000000000000, -1.000000000000000000, -0.000000000000000000 ) ) ;
#118888 = EDGE_LOOP ( 'NONE', ( #66503, #34187, #8392, #77004 ) ) ;
#118889 = CARTESIAN_POINT ( 'NONE',  ( -11.64999999999999858, 12.50000000000000000, -1.407149913249508666 ) ) ;
#118890 = VECTOR ( 'NONE', #3555, 1000.000000000000000 ) ;
#118891 = EDGE_LOOP ( 'NONE', ( #17987, #126019, #51565, #99051 ) ) ;
#118892 = ORIENTED_EDGE ( 'NONE', *, *, #121225, .F. ) ;
#118893 = CARTESIAN_POINT ( 'NONE',  ( -4.150000000000028777, 12.50000000000000000, -5.802370205355749988 ) ) ;
#118894 = PLANE ( 'NONE',  #17746 ) ;
#118895 = DIRECTION ( 'NONE',  ( 0.000000000000000000, 0.000000000000000000, 1.000000000000000000 ) ) ;
#118896 = DIRECTION ( 'NONE',  ( -0.000000000000000000, 1.000000000000000000, -0.000000000000000000 ) ) ;
#118897 = DIRECTION ( 'NONE',  ( 0.000000000000000000, 1.000000000000000000, 0.000000000000000000 ) ) ;
#118898 = FACE_OUTER_BOUND ( 'NONE', #73610, .T. ) ;
#118899 = DIRECTION ( 'NONE',  ( 0.000000000000000000, 1.000000000000000000, 0.000000000000000000 ) ) ;
#118900 = CARTESIAN_POINT ( 'NONE',  ( 8.749999999999923617, 12.50000000000000000, -7.188010851410854052 ) ) ;
#118901 = FACE_OUTER_BOUND ( 'NONE', #84851, .T. ) ;
#118902 = CIRCLE ( 'NONE', #77134, 0.06509327318403745899 ) ;
#118903 = CONICAL_SURFACE ( 'NONE', #24910, 0.09999999999999982514, 0.003490658503988666988 ) ;
#118904 = VECTOR ( 'NONE', #89911, 1000.000000000000000 ) ;
#118905 = EDGE_LOOP ( 'NONE', ( #99091, #125746, #83656, #60588 ) ) ;
#118906 = CIRCLE ( 'NONE', #54064, 0.06509327318403745899 ) ;
#118907 = CARTESIAN_POINT ( 'NONE',  ( 2.299999999999947864, 12.50000000000000000, 3.983716857408420964 ) ) ;
#118908 = CARTESIAN_POINT ( 'NONE',  ( 1.449999999999951328, 2.500000000000000000, -1.718653347947326049 ) ) ;
#118909 = DIRECTION ( 'NONE',  ( -4.274815082592931898E-19, -0.9999939076577903929, -0.003490651415223739937 ) ) ;
#118910 = FACE_OUTER_BOUND ( 'NONE', #81428, .T. ) ;
#118911 = CARTESIAN_POINT ( 'NONE',  ( -1.650000000000034328, 2.500000000000000000, -2.757883832488654097 ) ) ;
#118912 = CIRCLE ( 'NONE', #6031, 0.09999999999999999167 ) ;
#118913 = EDGE_LOOP ( 'NONE', ( #36947, #3015, #77188, #117389 ) ) ;
#118914 = DIRECTION ( 'NONE',  ( -0.000000000000000000, -1.000000000000000000, -0.000000000000000000 ) ) ;
#118915 = ADVANCED_FACE ( 'NONE', ( #82724 ), #53796, .T. ) ;
#118916 = AXIS2_PLACEMENT_3D ( 'NONE', #96014, #27263, #26629 ) ;
#118917 = EDGE_CURVE ( 'NONE', #84838, #29011, #44068, .T. ) ;
#118918 = DIRECTION ( 'NONE',  ( -0.000000000000000000, 1.000000000000000000, -0.000000000000000000 ) ) ;
#118920 = ORIENTED_EDGE ( 'NONE', *, *, #15535, .T. ) ;
#118919 = CARTESIAN_POINT ( 'NONE',  ( 12.49999999999990408, 2.500000000000000000, -3.537306695894649966 ) ) ;
#118921 = AXIS2_PLACEMENT_3D ( 'NONE', #43632, #45559, #95933 ) ;
#118922 = ORIENTED_EDGE ( 'NONE', *, *, #109861, .T. ) ;
#118923 = ADVANCED_FACE ( 'NONE', ( #2852 ), #83360, .T. ) ;
#118924 = CARTESIAN_POINT ( 'NONE',  ( -3.150000000000032330, 2.500000000000000000, -6.048780366869526581 ) ) ;
#118925 = CIRCLE ( 'NONE', #79231, 0.1000000000000002554 ) ;
#118926 = ADVANCED_FACE ( 'NONE', ( #70952 ), #110235, .T. ) ;
#118927 = ORIENTED_EDGE ( 'NONE', *, *, #47184, .T. ) ;
#118928 = ORIENTED_EDGE ( 'NONE', *, *, #32335, .T. ) ;
#118929 = ORIENTED_EDGE ( 'NONE', *, *, #59937, .T. ) ;
#118930 = CARTESIAN_POINT ( 'NONE',  ( 5.649999999999934630, 12.50000000000000000, 6.148780366869520897 ) ) ;
#118931 = DIRECTION ( 'NONE',  ( 0.000000000000000000, -0.000000000000000000, 1.000000000000000000 ) ) ;
#118932 = FACE_OUTER_BOUND ( 'NONE', #69233, .T. ) ;
#118933 = DIRECTION ( 'NONE',  ( 0.000000000000000000, 0.000000000000000000, -1.000000000000000000 ) ) ;
#118934 = AXIS2_PLACEMENT_3D ( 'NONE', #5492, #122236, #36280 ) ;
#118935 = EDGE_LOOP ( 'NONE', ( #73446, #54734, #74635, #107913 ) ) ;
#118936 = CARTESIAN_POINT ( 'NONE',  ( 0.6499999999999543920, 2.500000000000000000, 6.841600689897072485 ) ) ;
#118937 = ORIENTED_EDGE ( 'NONE', *, *, #91218, .T. ) ;
#118938 = DIRECTION ( 'NONE',  ( -0.000000000000000000, 1.000000000000000000, -0.000000000000000000 ) ) ;
#118939 = CARTESIAN_POINT ( 'NONE',  ( 18.87984495337894586, 0.5408627091909939955, 4.542689527608590794 ) ) ;
#118940 = DIRECTION ( 'NONE',  ( 0.000000000000000000, 1.000000000000000000, 0.000000000000000000 ) ) ;
#118941 = DIRECTION ( 'NONE',  ( -0.000000000000000000, 1.000000000000000000, -0.000000000000000000 ) ) ;
#118942 = ORIENTED_EDGE ( 'NONE', *, *, #35828, .F. ) ;
#118943 = AXIS2_PLACEMENT_3D ( 'NONE', #58051, #129389, #88109 ) ;
#118944 = VERTEX_POINT ( 'NONE', #101054 ) ;
#118945 = EDGE_LOOP ( 'NONE', ( #121090, #56546, #61369, #85036 ) ) ;
#118946 = EDGE_LOOP ( 'NONE', ( #33135, #117269, #48351, #127415 ) ) ;
#118947 = ORIENTED_EDGE ( 'NONE', *, *, #36885, .F. ) ;
#118948 = DIRECTION ( 'NONE',  ( 0.000000000000000000, 0.000000000000000000, -1.000000000000000000 ) ) ;
#118949 = DIRECTION ( 'NONE',  ( 0.000000000000000000, 0.000000000000000000, 1.000000000000000000 ) ) ;
#118950 = DIRECTION ( 'NONE',  ( 0.000000000000000000, 0.000000000000000000, 1.000000000000000000 ) ) ;
#118951 = FACE_BOUND ( 'NONE', #35574, .T. ) ;
#118952 = LINE ( 'NONE', #109112, #110029 ) ;
#118953 = CARTESIAN_POINT ( 'NONE',  ( 186.1145833340161175, 6.668395609140177704, -3.849999999999998312 ) ) ;
#118954 = AXIS2_PLACEMENT_3D ( 'NONE', #87309, #105679, #6790 ) ;
#118955 = DIRECTION ( 'NONE',  ( 0.000000000000000000, 0.000000000000000000, 1.000000000000000000 ) ) ;
#118956 = CARTESIAN_POINT ( 'NONE',  ( -9.800000000000004263, 12.50000000000000000, -0.2813168883297409439 ) ) ;
#118957 = AXIS2_PLACEMENT_3D ( 'NONE', #93990, #63241, #73691 ) ;
#118958 = CARTESIAN_POINT ( 'NONE',  ( 3.749999999999978684, 2.500000000000000000, -6.395190528383301931 ) ) ;
#118959 = DIRECTION ( 'NONE',  ( 0.000000000000000000, 0.000000000000000000, -1.000000000000000000 ) ) ;
#118960 = CIRCLE ( 'NONE', #62545, 0.1000000000000002554 ) ;
#118961 = DIRECTION ( 'NONE',  ( 0.000000000000000000, 1.000000000000000000, 0.000000000000000000 ) ) ;
#118962 = EDGE_CURVE ( 'NONE', #65442, #123620, #47549, .T. ) ;
#118963 = LINE ( 'NONE', #61993, #76523 ) ;
#118964 = AXIS2_PLACEMENT_3D ( 'NONE', #108754, #78682, #98291 ) ;
#118965 = ORIENTED_EDGE ( 'NONE', *, *, #105846, .T. ) ;
#118966 = ORIENTED_EDGE ( 'NONE', *, *, #53732, .F. ) ;
#118967 = VERTEX_POINT ( 'NONE', #51969 ) ;
#118968 = VERTEX_POINT ( 'NONE', #103641 ) ;
#118969 = ADVANCED_FACE ( 'NONE', ( #73516 ), #9889, .T. ) ;
#118970 = CARTESIAN_POINT ( 'NONE',  ( 12.09999999999990195, 12.50000000000000000, 0.6928203230275494784 ) ) ;
#118971 = AXIS2_PLACEMENT_3D ( 'NONE', #116235, #68428, #18686 ) ;
#118972 = CARTESIAN_POINT ( 'NONE',  ( -5.650000000000023448, 2.500000000000000000, -6.248780366869526759 ) ) ;
#118973 = EDGE_CURVE ( 'NONE', #78706, #37294, #83058, .T. ) ;
#118974 = FACE_BOUND ( 'NONE', #45362, .T. ) ;
#118975 = CARTESIAN_POINT ( 'NONE',  ( -3.750000000000027534, 12.50000000000000000, 2.792790559304612064 ) ) ;
#118977 = CIRCLE ( 'NONE', #70867, 0.1000000000000000472 ) ;
#118976 = AXIS2_PLACEMENT_3D ( 'NONE', #83008, #65266, #3788 ) ;
#118978 = VERTEX_POINT ( 'NONE', #23792 ) ;
#118979 = DIRECTION ( 'NONE',  ( 0.000000000000000000, 0.000000000000000000, 1.000000000000000000 ) ) ;
#118980 = LINE ( 'NONE', #60716, #118408 ) ;
#118981 = ADVANCED_FACE ( 'NONE', ( #71594 ), #18286, .T. ) ;
#118982 = DIRECTION ( 'NONE',  ( 0.000000000000000000, 1.000000000000000000, 0.000000000000000000 ) ) ;
#118983 = LINE ( 'NONE', #32410, #70881 ) ;
#118984 = DIRECTION ( 'NONE',  ( -4.274815082592931898E-19, -0.9999939076577903929, -0.003490651415223739937 ) ) ;
#118985 = VERTEX_POINT ( 'NONE', #111514 ) ;
#118986 = FACE_OUTER_BOUND ( 'NONE', #35629, .T. ) ;
#118987 = ORIENTED_EDGE ( 'NONE', *, *, #28005, .T. ) ;
#118988 = ORIENTED_EDGE ( 'NONE', *, *, #117975, .T. ) ;
#118989 = AXIS2_PLACEMENT_3D ( 'NONE', #46709, #125893, #94505 ) ;
#118990 = CARTESIAN_POINT ( 'NONE',  ( -12.89999999999999147, 2.500000000000000000, 4.330127018922196314 ) ) ;
#118991 = DIRECTION ( 'NONE',  ( 0.000000000000000000, 0.000000000000000000, 1.000000000000000000 ) ) ;
#118992 = ORIENTED_EDGE ( 'NONE', *, *, #70109, .T. ) ;
#118993 = CIRCLE ( 'NONE', #47909, 0.1000000000000002554 ) ;
#118994 = CARTESIAN_POINT ( 'NONE',  ( -1.050000000000037792, 2.500000000000000000, 6.248780366869520542 ) ) ;
#118995 = CONICAL_SURFACE ( 'NONE', #114780, 0.1000000000000002554, 0.003490658503988666988 ) ;
#118996 = CARTESIAN_POINT ( 'NONE',  ( 13.29999999999990301, 2.500000000000000000, 4.330127018922196314 ) ) ;
#118997 = EDGE_LOOP ( 'NONE', ( #51976, #54449, #30974, #47349 ) ) ;
#118998 = FACE_OUTER_BOUND ( 'NONE', #58386, .T. ) ;
#118999 = ORIENTED_EDGE ( 'NONE', *, *, #11406, .F. ) ;
#119000 = CARTESIAN_POINT ( 'NONE',  ( 13.09999999999990195, 12.50000000000000000, -4.676537180435978769 ) ) ;
#119002 = EDGE_LOOP ( 'NONE', ( #11552, #92339 ) ) ;
#119001 = AXIS2_PLACEMENT_3D ( 'NONE', #71573, #3481, #112801 ) ;
#119003 = CARTESIAN_POINT ( 'NONE',  ( 186.7812500006828031, 0.000000000000000000, 7.700000000000000178 ) ) ;
#119004 = FACE_BOUND ( 'NONE', #37023, .T. ) ;
#119005 = CIRCLE ( 'NONE', #114794, 0.09999999999999982514 ) ;
#119006 = EDGE_CURVE ( 'NONE', #80728, #120532, #120700, .T. ) ;
#119007 = CONICAL_SURFACE ( 'NONE', #62589, 0.1000000000000002554, 0.003490658503988666988 ) ;
#119008 = ORIENTED_EDGE ( 'NONE', *, *, #53376, .F. ) ;
#119009 = DIRECTION ( 'NONE',  ( 0.000000000000000000, 1.000000000000000000, 0.000000000000000000 ) ) ;
#119010 = EDGE_LOOP ( 'NONE', ( #120958, #88082 ) ) ;
#119011 = DIRECTION ( 'NONE',  ( -0.000000000000000000, 1.000000000000000000, -0.000000000000000000 ) ) ;
#119012 = CARTESIAN_POINT ( 'NONE',  ( -2.100000000000034284, 2.500000000000000000, -0.1000000000000023925 ) ) ;
#119013 = ADVANCED_FACE ( 'NONE', ( #101709 ), #58016, .T. ) ;
#119014 = DIRECTION ( 'NONE',  ( 0.000000000000000000, 1.000000000000000000, 0.000000000000000000 ) ) ;
#119016 = ADVANCED_FACE ( 'NONE', ( #82050 ), #99777, .T. ) ;
#119015 = DIRECTION ( 'NONE',  ( -4.274815082592931898E-19, -0.9999939076577903929, -0.003490651415223739937 ) ) ;
#119017 = EDGE_CURVE ( 'NONE', #75397, #95423, #23136, .T. ) ;
#119018 = CARTESIAN_POINT ( 'NONE',  ( 12.89999999999990266, 12.50000000000000000, 5.022947341949748790 ) ) ;
#119020 = ADVANCED_FACE ( 'NONE', ( #15226 ), #7348, .F. ) ;
#119019 = AXIS2_PLACEMENT_3D ( 'NONE', #114766, #44096, #93214 ) ;
#119021 = EDGE_LOOP ( 'NONE', ( #19674, #56823, #37560, #28432 ) ) ;
#119022 = ORIENTED_EDGE ( 'NONE', *, *, #2226, .F. ) ;
#119024 = ORIENTED_EDGE ( 'NONE', *, *, #104631, .T. ) ;
#119023 = AXIS2_PLACEMENT_3D ( 'NONE', #108911, #41510, #31046 ) ;
#119025 = DIRECTION ( 'NONE',  ( 0.000000000000000000, 1.000000000000000000, 0.000000000000000000 ) ) ;
#119026 = CONICAL_SURFACE ( 'NONE', #108559, 0.1000000000000002554, 0.003490658503988666988 ) ;
#119027 = DIRECTION ( 'NONE',  ( 0.000000000000000000, 1.000000000000000000, 0.000000000000000000 ) ) ;
#119028 = EDGE_CURVE ( 'NONE', #78573, #47526, #64258, .T. ) ;
#119029 = CARTESIAN_POINT ( 'NONE',  ( 12.94999999999989981, 12.50000000000000000, -2.165063509461101710 ) ) ;
#119031 = VERTEX_POINT ( 'NONE', #114099 ) ;
#119030 = ORIENTED_EDGE ( 'NONE', *, *, #110394, .F. ) ;
#119032 = EDGE_LOOP ( 'NONE', ( #65952, #108971, #66483, #115740 ) ) ;
#119033 = ADVANCED_FACE ( 'NONE', ( #34916 ), #46648, .T. ) ;
#119034 = DIRECTION ( 'NONE',  ( 0.000000000000000000, 0.000000000000000000, 1.000000000000000000 ) ) ;
#119035 = CARTESIAN_POINT ( 'NONE',  ( -13.09999999999999254, 2.500000000000000000, -0.3464101615137741286 ) ) ;
#119036 = SHAPE_DEFINITION_REPRESENTATION ( #97200, #89551 ) ;
#119037 = EDGE_CURVE ( 'NONE', #84136, #101321, #55181, .T. ) ;
#119038 = DIRECTION ( 'NONE',  ( -4.274815082592931898E-19, -0.9999939076577903929, -0.003490651415223739937 ) ) ;
#119039 = CARTESIAN_POINT ( 'NONE',  ( 195.0435778713738557, -1.025030745786872263E-15, 8.040022453829767102 ) ) ;
#119040 = LINE ( 'NONE', #535, #21465 ) ;
#119041 = DIRECTION ( 'NONE',  ( 0.000000000000000000, 1.000000000000000000, 0.000000000000000000 ) ) ;
#119042 = VECTOR ( 'NONE', #25801, 1000.000000000000000 ) ;
#119043 = DIRECTION ( 'NONE',  ( 0.000000000000000000, 0.000000000000000000, 1.000000000000000000 ) ) ;
#119044 = EDGE_CURVE ( 'NONE', #38154, #124518, #74176, .T. ) ;
#119046 = EDGE_CURVE ( 'NONE', #60634, #114454, #104902, .T. ) ;
#119045 = CARTESIAN_POINT ( 'NONE',  ( 7.899999999999921307, 2.500000000000000000, -0.1000000000000023925 ) ) ;
#119047 = ORIENTED_EDGE ( 'NONE', *, *, #126734, .F. ) ;
#119048 = ORIENTED_EDGE ( 'NONE', *, *, #8366, .F. ) ;
#119049 = CARTESIAN_POINT ( 'NONE',  ( 2.099999999999949463, 2.500000000000000000, 0.5928203230275495006 ) ) ;
#119050 = CARTESIAN_POINT ( 'NONE',  ( 7.499999999999927169, 2.500000000000000000, -5.022947341949754119 ) ) ;
#119051 = ORIENTED_EDGE ( 'NONE', *, *, #89241, .F. ) ;
#119052 = EDGE_LOOP ( 'NONE', ( #37171, #17952, #49384, #33686 ) ) ;
#119053 = APPLICATION_CONTEXT ( 'automotive_design' ) ;
#119054 = CARTESIAN_POINT ( 'NONE',  ( 185.9427083336747160, -6.551208109652278289, 3.782341765624995134 ) ) ;
#119055 = CARTESIAN_POINT ( 'NONE',  ( -11.25000000000000000, 2.500000000000000000, -2.857883832488649745 ) ) ;
#119056 = CIRCLE ( 'NONE', #54211, 0.06509327318403745899 ) ;
#119057 = DIRECTION ( 'NONE',  ( 0.000000000000000000, 1.000000000000000000, 0.000000000000000000 ) ) ;
#119058 = CARTESIAN_POINT ( 'NONE',  ( 1.649999999999951505, 2.500000000000000000, 1.572243186433545548 ) ) ;
#119059 = DIRECTION ( 'NONE',  ( 0.000000000000000000, -0.000000000000000000, 1.000000000000000000 ) ) ;
#119060 = CARTESIAN_POINT ( 'NONE',  ( -10.65000000000000391, 2.500000000000000000, -2.611473670974873595 ) ) ;
#119061 = DIRECTION ( 'NONE',  ( 0.000000000000000000, 0.000000000000000000, 1.000000000000000000 ) ) ;
#119062 = AXIS2_PLACEMENT_3D ( 'NONE', #28393, #67652, #77479 ) ;
#119063 = FACE_OUTER_BOUND ( 'NONE', #68820, .T. ) ;
#119064 = VERTEX_POINT ( 'NONE', #66913 ) ;
#119066 = VECTOR ( 'NONE', #20117, 1000.000000000000000 ) ;
#119065 = CIRCLE ( 'NONE', #6174, 0.1000000000000002554 ) ;
#119067 = ORIENTED_EDGE ( 'NONE', *, *, #91991, .F. ) ;
#119068 = CIRCLE ( 'NONE', #52171, 0.06509327318403745899 ) ;
#119069 = ORIENTED_EDGE ( 'NONE', *, *, #73607, .T. ) ;
#119070 = ORIENTED_EDGE ( 'NONE', *, *, #28607, .F. ) ;
#119071 = DIRECTION ( 'NONE',  ( 0.000000000000000000, 0.000000000000000000, 1.000000000000000000 ) ) ;
#119072 = DIRECTION ( 'NONE',  ( 0.000000000000000000, 0.000000000000000000, -1.000000000000000000 ) ) ;
#119075 = ORIENTED_EDGE ( 'NONE', *, *, #30600, .F. ) ;
#119074 = CIRCLE ( 'NONE', #116991, 0.06509327318403745899 ) ;
#119073 = AXIS2_PLACEMENT_3D ( 'NONE', #116300, #46280, #65919 ) ;
#119076 = CARTESIAN_POINT ( 'NONE',  ( 1.849999999999950129, 12.50000000000000000, -6.841600689897078702 ) ) ;
#119077 = EDGE_CURVE ( 'NONE', #100531, #115634, #104279, .T. ) ;
#119078 = DIRECTION ( 'NONE',  ( 0.000000000000000000, 0.000000000000000000, 1.000000000000000000 ) ) ;
#119079 = ADVANCED_FACE ( 'NONE', ( #116025 ), #85191, .T. ) ;
#119080 = CARTESIAN_POINT ( 'NONE',  ( -10.85000000000000142, 12.50000000000000000, 6.495190528383297135 ) ) ;
#119082 = ORIENTED_EDGE ( 'NONE', *, *, #117179, .T. ) ;
#119081 = DIRECTION ( 'NONE',  ( -4.274815082592931898E-19, -0.9999939076577903929, -0.003490651415223739937 ) ) ;
#119083 = CARTESIAN_POINT ( 'NONE',  ( 176.5000000000000000, 0.000000000000000000, 0.000000000000000000 ) ) ;
#119084 = PLANE ( 'NONE',  #87492 ) ;
#119085 = ORIENTED_EDGE ( 'NONE', *, *, #26593, .T. ) ;
#119086 = EDGE_LOOP ( 'NONE', ( #87695, #29424 ) ) ;
#119087 = VERTEX_POINT ( 'NONE', #54516 ) ;
#119088 = CIRCLE ( 'NONE', #38749, 0.1000000000000000056 ) ;
#119089 = ORIENTED_EDGE ( 'NONE', *, *, #78075, .F. ) ;
#119090 = DIRECTION ( 'NONE',  ( -0.000000000000000000, -1.000000000000000000, -0.000000000000000000 ) ) ;
#119091 = DIRECTION ( 'NONE',  ( 0.000000000000000000, -0.000000000000000000, 1.000000000000000000 ) ) ;
#119092 = CARTESIAN_POINT ( 'NONE',  ( -7.300000000000014921, 2.500000000000000000, 4.676537180435972552 ) ) ;
#119093 = CIRCLE ( 'NONE', #58467, 0.09999999999999999167 ) ;
#119094 = CIRCLE ( 'NONE', #96099, 0.09999999999999982514 ) ;
#119095 = ORIENTED_EDGE ( 'NONE', *, *, #116429, .T. ) ;
#119096 = LINE ( 'NONE', #69332, #45512 ) ;
#119097 = DIRECTION ( 'NONE',  ( 0.000000000000000000, 0.000000000000000000, -1.000000000000000000 ) ) ;
#119098 = DIRECTION ( 'NONE',  ( 0.000000000000000000, 1.000000000000000000, 0.000000000000000000 ) ) ;
#119099 = DIRECTION ( 'NONE',  ( 0.000000000000000000, 0.000000000000000000, -1.000000000000000000 ) ) ;
#119100 = AXIS2_PLACEMENT_3D ( 'NONE', #113273, #112643, #123104 ) ;
#119101 = CIRCLE ( 'NONE', #33440, 0.06509327318403745899 ) ;
#119102 = ORIENTED_EDGE ( 'NONE', *, *, #92127, .F. ) ;
#119103 = DIRECTION ( 'NONE',  ( 0.000000000000000000, 0.000000000000000000, -1.000000000000000000 ) ) ;
#119104 = EDGE_LOOP ( 'NONE', ( #83104, #31659 ) ) ;
#119105 = ORIENTED_EDGE ( 'NONE', *, *, #4452, .T. ) ;
#119106 = CARTESIAN_POINT ( 'NONE',  ( -0.6500000000000394351, 2.500000000000000000, 6.841600689897072485 ) ) ;
#119107 = DIRECTION ( 'NONE',  ( 0.000000000000000000, 0.000000000000000000, -1.000000000000000000 ) ) ;
#119108 = FACE_BOUND ( 'NONE', #19192, .T. ) ;
#119109 = CIRCLE ( 'NONE', #89855, 0.09999999999999982514 ) ;
#119110 = LINE ( 'NONE', #68067, #7510 ) ;
#119111 = PLANE ( 'NONE',  #107126 ) ;
#119112 = DIRECTION ( 'NONE',  ( -0.000000000000000000, 1.000000000000000000, -0.000000000000000000 ) ) ;
#119114 = EDGE_CURVE ( 'NONE', #42431, #105649, #76753, .T. ) ;
#119113 = CIRCLE ( 'NONE', #108641, 0.1000000000000002554 ) ;
#119115 = AXIS2_PLACEMENT_3D ( 'NONE', #51188, #72112, #112677 ) ;
#119116 = VERTEX_POINT ( 'NONE', #4763 ) ;
#119117 = CARTESIAN_POINT ( 'NONE',  ( -0.6000000000000323963, 2.500000000000000000, -0.3464101615137759604 ) ) ;
#119118 = CARTESIAN_POINT ( 'NONE',  ( 11.64999999999990798, 12.50000000000000000, -2.792790559304616504 ) ) ;
#119119 = DIRECTION ( 'NONE',  ( -0.000000000000000000, -1.000000000000000000, -0.000000000000000000 ) ) ;
#119120 = CARTESIAN_POINT ( 'NONE',  ( 0.8499999999999557909, 2.500000000000000000, -7.088010851410853519 ) ) ;
#119121 = VERTEX_POINT ( 'NONE', #5420 ) ;
#119122 = AXIS2_PLACEMENT_3D ( 'NONE', #112022, #122490, #63569 ) ;
#119123 = ADVANCED_FACE ( 'NONE', ( #44725 ), #91448, .T. ) ;
#119124 = FACE_OUTER_BOUND ( 'NONE', #93333, .T. ) ;
#119125 = DIRECTION ( 'NONE',  ( 0.000000000000000000, 0.000000000000000000, -1.000000000000000000 ) ) ;
#119126 = AXIS2_PLACEMENT_3D ( 'NONE', #43376, #42076, #83295 ) ;
#119127 = EDGE_LOOP ( 'NONE', ( #36815, #83041, #49560, #10407 ) ) ;
#119128 = ORIENTED_EDGE ( 'NONE', *, *, #125840, .F. ) ;
#119129 = ADVANCED_FACE ( 'NONE', ( #27013 ), #5746, .T. ) ;
#119130 = DIRECTION ( 'NONE',  ( 0.000000000000000000, 0.000000000000000000, 1.000000000000000000 ) ) ;
#119132 = EDGE_CURVE ( 'NONE', #74569, #23572, #114734, .T. ) ;
#119131 = CARTESIAN_POINT ( 'NONE',  ( -5.000000000000023093, 12.50000000000000000, 5.022947341949748790 ) ) ;
#119133 = FACE_BOUND ( 'NONE', #85883, .T. ) ;
#119134 = CARTESIAN_POINT ( 'NONE',  ( 5.199999999999935341, 12.50000000000000000, -3.983716857408426293 ) ) ;
#119135 = DIRECTION ( 'NONE',  ( -0.000000000000000000, 1.000000000000000000, -0.000000000000000000 ) ) ;
#119136 = ORIENTED_EDGE ( 'NONE', *, *, #7306, .T. ) ;
#119137 = CARTESIAN_POINT ( 'NONE',  ( -9.350000000000006750, 2.500000000000000000, -2.611473670974877592 ) ) ;
#119138 = ADVANCED_FACE ( 'NONE', ( #75449 ), #30919, .T. ) ;
#119139 = CARTESIAN_POINT ( 'NONE',  ( 185.3750000000000284, 8.891194145520236347, 5.444286225454521982E-16 ) ) ;
#119140 = ORIENTED_EDGE ( 'NONE', *, *, #106639, .T. ) ;
#119141 = CARTESIAN_POINT ( 'NONE',  ( 13.54999999999989591, 2.500000000000000000, -1.718653347947326049 ) ) ;
#119142 = CARTESIAN_POINT ( 'NONE',  ( -9.200000000000006395, 2.500000000000000000, -2.385244779468109755E-15 ) ) ;
#119143 = PLANE ( 'NONE',  #121720 ) ;
#119144 = AXIS2_PLACEMENT_3D ( 'NONE', #10357, #109857, #40489 ) ;
#119145 = CARTESIAN_POINT ( 'NONE',  ( -6.650000000000014566, 2.500000000000000000, 2.265063509461097357 ) ) ;
#119146 = EDGE_LOOP ( 'NONE', ( #86223, #106602 ) ) ;
#119148 = CIRCLE ( 'NONE', #106532, 0.09999999999999982514 ) ;
#119147 = CIRCLE ( 'NONE', #79460, 0.09999999999999982514 ) ;
#119149 = CARTESIAN_POINT ( 'NONE',  ( -0.4000000000000339950, 12.50000000000000000, 0.7579135962115892688 ) ) ;
#119150 = DIRECTION ( 'NONE',  ( 0.000000000000000000, 1.000000000000000000, 0.000000000000000000 ) ) ;
#119151 = CARTESIAN_POINT ( 'NONE',  ( 16.56034315062901641, 0.8287392047036494791, -6.090234455234604383 ) ) ;
#119152 = VERTEX_POINT ( 'NONE', #105570 ) ;
#119153 = EDGE_LOOP ( 'NONE', ( #30731, #90891 ) ) ;
#119154 = DIRECTION ( 'NONE',  ( 0.000000000000000000, 1.000000000000000000, 0.000000000000000000 ) ) ;
#119155 = ORIENTED_EDGE ( 'NONE', *, *, #118585, .T. ) ;
#119156 = LINE ( 'NONE', #79249, #32362 ) ;
#119159 = CARTESIAN_POINT ( 'NONE',  ( -8.150000000000009237, 2.500000000000000000, 6.741600689897071952 ) ) ;
#119158 = VECTOR ( 'NONE', #89014, 1000.000000000000000 ) ;
#119157 = CIRCLE ( 'NONE', #77398, 0.1000000000000002554 ) ;
#119160 = EDGE_CURVE ( 'NONE', #61030, #73196, #112484, .T. ) ;
#119161 = CARTESIAN_POINT ( 'NONE',  ( -11.64999999999999680, 2.500000000000000000, 7.188010851410848723 ) ) ;
#119162 = VERTEX_POINT ( 'NONE', #106214 ) ;
#119163 = CARTESIAN_POINT ( 'NONE',  ( -5.850000000000019185, 12.50000000000000000, 2.230156782645134950 ) ) ;
#119164 = CARTESIAN_POINT ( 'NONE',  ( -3.150000000000029221, 2.500000000000000000, 2.411473670974873862 ) ) ;
#119165 = LINE ( 'NONE', #89070, #94554 ) ;
#119166 = DIRECTION ( 'NONE',  ( 0.000000000000000000, 0.000000000000000000, 1.000000000000000000 ) ) ;
#119167 = CARTESIAN_POINT ( 'NONE',  ( 3.749999999999938716, 2.500000000000000000, 7.088010851410848190 ) ) ;
#119168 = EDGE_CURVE ( 'NONE', #119203, #99284, #86561, .T. ) ;
#119169 = DIRECTION ( 'NONE',  ( 0.000000000000000000, 0.000000000000000000, 1.000000000000000000 ) ) ;
#119170 = EDGE_CURVE ( 'NONE', #23744, #61622, #35132, .T. ) ;
#119171 = ORIENTED_EDGE ( 'NONE', *, *, #62134, .T. ) ;
#119172 = ORIENTED_EDGE ( 'NONE', *, *, #50626, .T. ) ;
#119173 = DIRECTION ( 'NONE',  ( -0.000000000000000000, 1.000000000000000000, -0.000000000000000000 ) ) ;
#119174 = EDGE_LOOP ( 'NONE', ( #41382, #124579, #62661, #17074 ) ) ;
#119175 = CARTESIAN_POINT ( 'NONE',  ( 106.6738984060675079, 6.002110804423450574, 4.823747364179781449 ) ) ;
#119176 = EDGE_CURVE ( 'NONE', #101758, #17235, #3709, .T. ) ;
#119178 = ORIENTED_EDGE ( 'NONE', *, *, #110627, .T. ) ;
#119177 = ORIENTED_EDGE ( 'NONE', *, *, #28699, .T. ) ;
#119179 = ADVANCED_FACE ( 'NONE', ( #127152 ), #114516, .T. ) ;
#119180 = ORIENTED_EDGE ( 'NONE', *, *, #33888, .F. ) ;
#119181 = EDGE_CURVE ( 'NONE', #31716, #31853, #39343, .T. ) ;
#119182 = CARTESIAN_POINT ( 'NONE',  ( 17.50000000000000000, 2.083333333333335258, -3.999999999999996447 ) ) ;
#119183 = EDGE_CURVE ( 'NONE', #97290, #85218, #120787, .T. ) ;
#119184 = CIRCLE ( 'NONE', #39783, 0.06509327318403745899 ) ;
#119185 = CARTESIAN_POINT ( 'NONE',  ( -2.300000000000033573, 12.50000000000000000, -3.918623584224389056 ) ) ;
#119186 = CIRCLE ( 'NONE', #43895, 0.06509327318403745899 ) ;
#119187 = DIRECTION ( 'NONE',  ( 0.000000000000000000, 0.000000000000000000, -1.000000000000000000 ) ) ;
#119188 = SURFACE_SIDE_STYLE ('',( #77967 ) ) ;
#119189 = EDGE_CURVE ( 'NONE', #113481, #86732, #20414, .T. ) ;
#119190 = PLANE ( 'NONE',  #51420 ) ;
#119191 = DIRECTION ( 'NONE',  ( -0.000000000000000000, 1.000000000000000000, -0.000000000000000000 ) ) ;
#119192 = CARTESIAN_POINT ( 'NONE',  ( -3.150000000000030109, 12.50000000000000000, -2.511473670974877948 ) ) ;
#119193 = CARTESIAN_POINT ( 'NONE',  ( 5.399999999999936406, 12.50000000000000000, -5.022947341949754119 ) ) ;
#119194 = DIRECTION ( 'NONE',  ( 0.000000000000000000, 0.000000000000000000, -1.000000000000000000 ) ) ;
#119197 = EDGE_CURVE ( 'NONE', #56994, #125139, #108268, .T. ) ;
#119196 = AXIS2_PLACEMENT_3D ( 'NONE', #14279, #75152, #34606 ) ;
#119195 = DIRECTION ( 'NONE',  ( -0.000000000000000000, 1.000000000000000000, -0.000000000000000000 ) ) ;
#119198 = ORIENTED_EDGE ( 'NONE', *, *, #764, .T. ) ;
#119199 = ADVANCED_FACE ( 'NONE', ( #59051 ), #78039, .T. ) ;
#119200 = EDGE_LOOP ( 'NONE', ( #66044, #11337, #23895, #19471 ) ) ;
#119201 = CARTESIAN_POINT ( 'NONE',  ( -2.100000000000033840, 2.500000000000000000, 3.637306695894644726 ) ) ;
#119202 = ORIENTED_EDGE ( 'NONE', *, *, #58363, .F. ) ;
#119203 = VERTEX_POINT ( 'NONE', #111 ) ;
#119204 = DIRECTION ( 'NONE',  ( -4.274815082592931898E-19, -0.9999939076577903929, -0.003490651415223739937 ) ) ;
#119205 = AXIS2_PLACEMENT_3D ( 'NONE', #60707, #53468, #90800 ) ;
#119206 = VECTOR ( 'NONE', #64824, 1000.000000000000000 ) ;
#119207 = DIRECTION ( 'NONE',  ( 0.000000000000000000, -0.000000000000000000, 1.000000000000000000 ) ) ;
#119208 = CIRCLE ( 'NONE', #66951, 0.1000000000000002554 ) ;
#119209 = CARTESIAN_POINT ( 'NONE',  ( -0.8500000000000382805, 2.500000000000000000, -1.372243186433550033 ) ) ;
#119210 = FACE_OUTER_BOUND ( 'NONE', #88144, .T. ) ;
#119211 = LINE ( 'NONE', #60315, #71886 ) ;
#119212 = ORIENTED_EDGE ( 'NONE', *, *, #127895, .F. ) ;
#119213 = CIRCLE ( 'NONE', #104624, 0.1000000000000002554 ) ;
#119214 = ORIENTED_EDGE ( 'NONE', *, *, #115934, .T. ) ;
#119215 = CARTESIAN_POINT ( 'NONE',  ( 11.44999999999990514, 12.50000000000000000, -6.148780366869526226 ) ) ;
#119216 = ORIENTED_EDGE ( 'NONE', *, *, #85012, .T. ) ;
#119217 = DIRECTION ( 'NONE',  ( -0.000000000000000000, 1.000000000000000000, -0.000000000000000000 ) ) ;
#119218 = AXIS2_PLACEMENT_3D ( 'NONE', #47170, #37983, #117162 ) ;
#119219 = ORIENTED_EDGE ( 'NONE', *, *, #50167, .F. ) ;
#119220 = ORIENTED_EDGE ( 'NONE', *, *, #23708, .F. ) ;
#119221 = CARTESIAN_POINT ( 'NONE',  ( 10.44999999999991047, 12.50000000000000000, -6.495190528383302464 ) ) ;
#119222 = CARTESIAN_POINT ( 'NONE',  ( 10.84999999999991260, 2.500000000000000000, 5.902370205355745192 ) ) ;
#119223 = LINE ( 'NONE', #88, #84297 ) ;
#119224 = EDGE_CURVE ( 'NONE', #109349, #102868, #89144, .T. ) ;
#119225 = DIRECTION ( 'NONE',  ( -0.000000000000000000, -1.000000000000000000, -0.000000000000000000 ) ) ;
#119226 = CARTESIAN_POINT ( 'NONE',  ( 7.099999999999928590, 2.500000000000000000, -5.122947341949753763 ) ) ;
#119227 = EDGE_LOOP ( 'NONE', ( #67281, #98255 ) ) ;
#119228 = CARTESIAN_POINT ( 'NONE',  ( -13.29999999999998828, 2.500000000000000000, 4.330127018922196314 ) ) ;
#119229 = DIRECTION ( 'NONE',  ( -0.000000000000000000, 1.000000000000000000, -0.000000000000000000 ) ) ;
#119230 = CARTESIAN_POINT ( 'NONE',  ( -9.600000000000006750, 12.50000000000000000, 5.022947341949748790 ) ) ;
#119231 = CARTESIAN_POINT ( 'NONE',  ( 3.349999999999945466, 2.500000000000000000, -6.595190528383302109 ) ) ;
#119233 = EDGE_CURVE ( 'NONE', #17511, #111104, #93602, .T. ) ;
#119232 = DIRECTION ( 'NONE',  ( -0.000000000000000000, -1.000000000000000000, -0.000000000000000000 ) ) ;
#119234 = ORIENTED_EDGE ( 'NONE', *, *, #128508, .T. ) ;
#119235 = ORIENTED_EDGE ( 'NONE', *, *, #41302, .F. ) ;
#119236 = FACE_OUTER_BOUND ( 'NONE', #75344, .T. ) ;
#119237 = AXIS2_PLACEMENT_3D ( 'NONE', #11645, #32611, #72514 ) ;
#119238 = ORIENTED_EDGE ( 'NONE', *, *, #48014, .T. ) ;
#119239 = DIRECTION ( 'NONE',  ( 0.000000000000000000, 0.000000000000000000, 1.000000000000000000 ) ) ;
#119240 = FACE_OUTER_BOUND ( 'NONE', #92753, .T. ) ;
#119242 = VECTOR ( 'NONE', #121370, 1000.000000000000000 ) ;
#119241 = AXIS2_PLACEMENT_3D ( 'NONE', #85275, #113449, #72257 ) ;
#119243 = VERTEX_POINT ( 'NONE', #9298 ) ;
#119244 = DIRECTION ( 'NONE',  ( 0.000000000000000000, 0.000000000000000000, 1.000000000000000000 ) ) ;
#119245 = DIRECTION ( 'NONE',  ( 0.000000000000000000, -1.000000000000000000, 0.000000000000000000 ) ) ;
#119246 = DIRECTION ( 'NONE',  ( 0.000000000000000000, 0.000000000000000000, 1.000000000000000000 ) ) ;
#119247 = CARTESIAN_POINT ( 'NONE',  ( -7.300000000000014921, 2.500000000000000000, 4.676537180435972552 ) ) ;
#119248 = PLANE ( 'NONE',  #68688 ) ;
#119249 = ORIENTED_EDGE ( 'NONE', *, *, #30969, .T. ) ;
#119250 = CARTESIAN_POINT ( 'NONE',  ( 59.74179236529985815, 3.401974343112436738, -5.439312642699807299 ) ) ;
#119251 = CARTESIAN_POINT ( 'NONE',  ( -12.49999999999995737, 12.50000000000000000, 4.330127018922196314 ) ) ;
#119252 = DIRECTION ( 'NONE',  ( -0.000000000000000000, -1.000000000000000000, -0.000000000000000000 ) ) ;
#119253 = ADVANCED_FACE ( 'NONE', ( #17817 ), #72762, .T. ) ;
#119254 = EDGE_LOOP ( 'NONE', ( #128879, #123522, #4475, #95439 ) ) ;
#119255 = DIRECTION ( 'NONE',  ( -0.000000000000000000, 1.000000000000000000, -0.000000000000000000 ) ) ;
#119256 = ORIENTED_EDGE ( 'NONE', *, *, #78108, .T. ) ;
#119257 = PLANE ( 'NONE',  #121168 ) ;
#119258 = CARTESIAN_POINT ( 'NONE',  ( 8.749999999999921840, 12.50000000000000000, 2.792790559304612064 ) ) ;
#119259 = CARTESIAN_POINT ( 'NONE',  ( 11.04999999999990656, 12.50000000000000000, -6.148780366869526226 ) ) ;
#119260 = ORIENTED_EDGE ( 'NONE', *, *, #129246, .F. ) ;
#119261 = VECTOR ( 'NONE', #98940, 1000.000000000000000 ) ;
#119262 = EDGE_CURVE ( 'NONE', #44544, #27907, #87325, .T. ) ;
#119263 = CARTESIAN_POINT ( 'NONE',  ( 6.049999999999932321, 12.50000000000000000, 1.818653347947321475 ) ) ;
#119264 = VECTOR ( 'NONE', #64619, 1000.000000000000000 ) ;
#119265 = CARTESIAN_POINT ( 'NONE',  ( 185.4895833340161175, -4.445597072760163471, -7.699999999999919353 ) ) ;
#119266 = EDGE_CURVE ( 'NONE', #43427, #88605, #27627, .T. ) ;
#119267 = VERTEX_POINT ( 'NONE', #68208 ) ;
#119268 = EDGE_CURVE ( 'NONE', #123245, #59339, #68548, .T. ) ;
#119269 = DIRECTION ( 'NONE',  ( 0.000000000000000000, 0.000000000000000000, 1.000000000000000000 ) ) ;
#119270 = ADVANCED_FACE ( 'NONE', ( #49887 ), #5846, .T. ) ;
#119271 = ORIENTED_EDGE ( 'NONE', *, *, #20753, .F. ) ;
#119272 = CIRCLE ( 'NONE', #92083, 0.1000000000000000472 ) ;
#119273 = FACE_OUTER_BOUND ( 'NONE', #25278, .T. ) ;
#119274 = ORIENTED_EDGE ( 'NONE', *, *, #29805, .F. ) ;
#119275 = DIRECTION ( 'NONE',  ( 0.000000000000000000, -0.9999939076577903929, 0.003490651415223739937 ) ) ;
#119276 = CARTESIAN_POINT ( 'NONE',  ( 6.899999999999926636, 12.50000000000000000, -0.2813168883297408329 ) ) ;
#119277 = ADVANCED_FACE ( 'NONE', ( #59716 ), #57766, .T. ) ;
#119278 = EDGE_LOOP ( 'NONE', ( #70608, #61769, #40707, #21238 ) ) ;
#119279 = ORIENTED_EDGE ( 'NONE', *, *, #10663, .F. ) ;
#119280 = EDGE_CURVE ( 'NONE', #61052, #95146, #102013, .T. ) ;
#119281 = CARTESIAN_POINT ( 'NONE',  ( -8.350000000000008527, 12.50000000000000000, 5.802370205355744659 ) ) ;
#119282 = DIRECTION ( 'NONE',  ( 0.000000000000000000, 0.000000000000000000, 1.000000000000000000 ) ) ;
#119283 = VERTEX_POINT ( 'NONE', #18470 ) ;
#119284 = DIRECTION ( 'NONE',  ( -4.274815082592931898E-19, -0.9999939076577903929, -0.003490651415223739937 ) ) ;
#119285 = CARTESIAN_POINT ( 'NONE',  ( 186.4010416670080588, -4.367472073101520635, 7.564683531249999149 ) ) ;
#119286 = CIRCLE ( 'NONE', #106762, 0.1000000000000002554 ) ;
#119287 = CARTESIAN_POINT ( 'NONE',  ( 9.599999999999914380, 2.500000000000000000, -5.122947341949753763 ) ) ;
#119288 = CARTESIAN_POINT ( 'NONE',  ( 105.7595978339907390, 7.458259062902370395, 4.481802286990411055 ) ) ;
#119289 = DIRECTION ( 'NONE',  ( 0.000000000000000000, -1.000000000000000000, 0.000000000000000000 ) ) ;
#119290 = DIRECTION ( 'NONE',  ( 0.000000000000000000, -0.9999939076577903929, 0.003490651415223739937 ) ) ;
#119291 = CARTESIAN_POINT ( 'NONE',  ( 3.949999999999942446, 12.50000000000000000, -6.776507416713040577 ) ) ;
#119292 = ORIENTED_EDGE ( 'NONE', *, *, #43227, .F. ) ;
#119293 = EDGE_LOOP ( 'NONE', ( #47455, #58880, #20940, #108897 ) ) ;
#119294 = EDGE_LOOP ( 'NONE', ( #80706, #51937, #93930, #82257 ) ) ;
#119295 = ORIENTED_EDGE ( 'NONE', *, *, #56164, .T. ) ;
#119296 = CIRCLE ( 'NONE', #21010, 0.1000000000000002554 ) ;
#119297 = FACE_OUTER_BOUND ( 'NONE', #99789, .T. ) ;
#119298 = CARTESIAN_POINT ( 'NONE',  ( -8.100000000000013856, 12.50000000000000000, -3.983716857408426293 ) ) ;
#119299 = CARTESIAN_POINT ( 'NONE',  ( 0.3999999999999619971, 12.50000000000000000, -0.06509327318403752838 ) ) ;
#119300 = ORIENTED_EDGE ( 'NONE', *, *, #123411, .F. ) ;
#119301 = FACE_BOUND ( 'NONE', #28696, .T. ) ;
#119302 = EDGE_LOOP ( 'NONE', ( #108076, #99994 ) ) ;
#119303 = FACE_OUTER_BOUND ( 'NONE', #74278, .T. ) ;
#119304 = CARTESIAN_POINT ( 'NONE',  ( 0.6499999999999566125, 12.50000000000000000, -6.213873640053564351 ) ) ;
#119305 = DIRECTION ( 'NONE',  ( -4.274815082592931898E-19, -0.9999939076577903929, -0.003490651415223739937 ) ) ;
#119306 = LINE ( 'NONE', #48015, #74336 ) ;
#119307 = CARTESIAN_POINT ( 'NONE',  ( -7.500000000000016875, 2.500000000000000000, 0.5928203230275495006 ) ) ;
#119308 = CARTESIAN_POINT ( 'NONE',  ( -8.100000000000013856, 2.500000000000000000, -3.983716857408426293 ) ) ;
#119309 = CARTESIAN_POINT ( 'NONE',  ( 6.049999999999934097, 2.500000000000000000, 6.248780366869521430 ) ) ;
#119310 = CARTESIAN_POINT ( 'NONE',  ( 6.649999999999929301, 12.50000000000000000, -2.099970236277064473 ) ) ;
#119311 = DIRECTION ( 'NONE',  ( 0.000000000000000000, 0.000000000000000000, 1.000000000000000000 ) ) ;
#119312 = DIRECTION ( 'NONE',  ( -0.000000000000000000, 1.000000000000000000, -0.000000000000000000 ) ) ;
#119313 = VERTEX_POINT ( 'NONE', #8629 ) ;
#119314 = ORIENTED_EDGE ( 'NONE', *, *, #3678, .T. ) ;
#119315 = ORIENTED_EDGE ( 'NONE', *, *, #5932, .F. ) ;
#119316 = ORIENTED_EDGE ( 'NONE', *, *, #121702, .F. ) ;
#119317 = CARTESIAN_POINT ( 'NONE',  ( 12.49999999999990585, 2.500000000000000000, 3.537306695894645081 ) ) ;
#119319 = EDGE_CURVE ( 'NONE', #66544, #76524, #16306, .T. ) ;
#119318 = AXIS2_PLACEMENT_3D ( 'NONE', #89743, #49836, #91031 ) ;
#119320 = DIRECTION ( 'NONE',  ( 0.000000000000000000, -0.9999939076577903929, 0.003490651415223739937 ) ) ;
#119321 = TOROIDAL_SURFACE ( 'NONE', #98387, 9.000000000000001776, 1.000000000000000000 ) ;
#119322 = EDGE_CURVE ( 'NONE', #32088, #124819, #91724, .T. ) ;
#119323 = AXIS2_PLACEMENT_3D ( 'NONE', #116130, #103747, #34377 ) ;
#119325 = EDGE_LOOP ( 'NONE', ( #42892, #73925, #9753, #42376 ) ) ;
#119324 = ORIENTED_EDGE ( 'NONE', *, *, #43595, .F. ) ;
#119326 = ORIENTED_EDGE ( 'NONE', *, *, #14691, .T. ) ;
#119327 = EDGE_CURVE ( 'NONE', #123047, #118212, #83154, .T. ) ;
#119328 = DIRECTION ( 'NONE',  ( -4.274815082592931898E-19, -0.9999939076577903929, -0.003490651415223739937 ) ) ;
#119329 = EDGE_CURVE ( 'NONE', #93441, #47940, #32187, .T. ) ;
#119330 = CIRCLE ( 'NONE', #16887, 0.06509327318403745899 ) ;
#119331 = FACE_OUTER_BOUND ( 'NONE', #28356, .T. ) ;
#119332 = LINE ( 'NONE', #89236, #122976 ) ;
#119333 = CARTESIAN_POINT ( 'NONE',  ( 7.049999999999928768, 12.50000000000000000, -2.165063509461101710 ) ) ;
#119334 = EDGE_CURVE ( 'NONE', #52069, #94129, #43449, .T. ) ;
#119335 = PLANE ( 'NONE',  #9545 ) ;
#119336 = LINE ( 'NONE', #9398, #10018 ) ;
#119337 = AXIS2_PLACEMENT_3D ( 'NONE', #3598, #101809, #23227 ) ;
#119338 = PLANE ( 'NONE',  #84491 ) ;
#119339 = VERTEX_POINT ( 'NONE', #32824 ) ;
#119341 = ADVANCED_FACE ( 'NONE', ( #52439 ), #110708, .T. ) ;
#119340 = DIRECTION ( 'NONE',  ( 0.000000000000000000, 0.000000000000000000, 1.000000000000000000 ) ) ;
#119342 = ORIENTED_EDGE ( 'NONE', *, *, #38696, .T. ) ;
#119343 = EDGE_CURVE ( 'NONE', #37520, #18828, #31518, .T. ) ;
#119344 = EDGE_LOOP ( 'NONE', ( #6136, #8395, #99458, #26116 ) ) ;
#119345 = VERTEX_POINT ( 'NONE', #42652 ) ;
#119346 = LINE ( 'NONE', #29688, #40026 ) ;
#119347 = ORIENTED_EDGE ( 'NONE', *, *, #47323, .F. ) ;
#119348 = VERTEX_POINT ( 'NONE', #112016 ) ;
#119349 = CARTESIAN_POINT ( 'NONE',  ( -4.600000000000028066, 2.500000000000000000, -3.637306695894650055 ) ) ;
#119350 = AXIS2_PLACEMENT_3D ( 'NONE', #20816, #119011, #88913 ) ;
#119351 = LINE ( 'NONE', #19879, #103947 ) ;
#119352 = DIRECTION ( 'NONE',  ( 0.000000000000000000, 0.000000000000000000, -1.000000000000000000 ) ) ;
#119353 = FACE_OUTER_BOUND ( 'NONE', #94524, .T. ) ;
#119354 = DIRECTION ( 'NONE',  ( 0.000000000000000000, 0.000000000000000000, -1.000000000000000000 ) ) ;
#119355 = ORIENTED_EDGE ( 'NONE', *, *, #91256, .T. ) ;
#119356 = DIRECTION ( 'NONE',  ( -0.000000000000000000, 1.000000000000000000, -0.000000000000000000 ) ) ;
#119357 = AXIS2_PLACEMENT_3D ( 'NONE', #7812, #8447, #96189 ) ;
#119358 = AXIS2_PLACEMENT_3D ( 'NONE', #30526, #78971, #39710 ) ;
#119359 = ORIENTED_EDGE ( 'NONE', *, *, #116901, .T. ) ;
#119360 = CARTESIAN_POINT ( 'NONE',  ( -3.300000000000027800, 12.50000000000000000, -4.395220292106239768 ) ) ;
#119361 = VERTEX_POINT ( 'NONE', #11220 ) ;
#119362 = DIRECTION ( 'NONE',  ( 0.000000000000000000, 0.000000000000000000, -1.000000000000000000 ) ) ;
#119363 = DIRECTION ( 'NONE',  ( -0.000000000000000000, 1.000000000000000000, -0.000000000000000000 ) ) ;
#119364 = ORIENTED_EDGE ( 'NONE', *, *, #86204, .T. ) ;
#119365 = DIRECTION ( 'NONE',  ( -0.000000000000000000, -1.000000000000000000, -0.000000000000000000 ) ) ;
#119366 = FACE_OUTER_BOUND ( 'NONE', #94846, .T. ) ;
#119367 = ORIENTED_EDGE ( 'NONE', *, *, #23125, .F. ) ;
#119368 = VECTOR ( 'NONE', #68163, 1000.000000000000000 ) ;
#119369 = DIRECTION ( 'NONE',  ( -0.000000000000000000, 1.000000000000000000, -0.000000000000000000 ) ) ;
#119370 = ORIENTED_EDGE ( 'NONE', *, *, #32070, .T. ) ;
#119371 = EDGE_LOOP ( 'NONE', ( #22459, #90508, #105475, #109538 ) ) ;
#119372 = DIRECTION ( 'NONE',  ( 0.000000000000000000, 0.000000000000000000, -1.000000000000000000 ) ) ;
#119373 = CARTESIAN_POINT ( 'NONE',  ( 8.099999999999923261, 2.500000000000000000, 4.083716857408420609 ) ) ;
#119374 = CARTESIAN_POINT ( 'NONE',  ( 184.0052083336747160, -6.551208109652278289, 3.782341765624995134 ) ) ;
#119375 = DIRECTION ( 'NONE',  ( 0.000000000000000000, 1.000000000000000000, 0.000000000000000000 ) ) ;
#119376 = CIRCLE ( 'NONE', #104783, 0.06509327318403745899 ) ;
#119377 = AXIS2_PLACEMENT_3D ( 'NONE', #70985, #111548, #92550 ) ;
#119379 = EDGE_CURVE ( 'NONE', #110270, #3522, #20439, .T. ) ;
#119378 = DIRECTION ( 'NONE',  ( -0.000000000000000000, -1.000000000000000000, -0.000000000000000000 ) ) ;
#119380 = VERTEX_POINT ( 'NONE', #40716 ) ;
#119381 = CARTESIAN_POINT ( 'NONE',  ( 184.1979166673494603, 6.668395609140176816, 3.850000000000000977 ) ) ;
#119382 = ORIENTED_EDGE ( 'NONE', *, *, #113728, .T. ) ;
#119383 = DIRECTION ( 'NONE',  ( 0.000000000000000000, 0.000000000000000000, -1.000000000000000000 ) ) ;
#119384 = DIRECTION ( 'NONE',  ( -0.000000000000000000, 1.000000000000000000, -0.000000000000000000 ) ) ;
#119385 = AXIS2_PLACEMENT_3D ( 'NONE', #62487, #102401, #12702 ) ;
#119386 = AXIS2_PLACEMENT_3D ( 'NONE', #116928, #17435, #56709 ) ;
#119387 = FACE_OUTER_BOUND ( 'NONE', #104255, .T. ) ;
#119388 = CARTESIAN_POINT ( 'NONE',  ( 5.849999999999933920, 12.50000000000000000, -2.165063509461101710 ) ) ;
#119389 = FACE_OUTER_BOUND ( 'NONE', #93132, .T. ) ;
#119390 = CARTESIAN_POINT ( 'NONE',  ( 5.199999999999937117, 2.500000000000000000, -4.676537180435978769 ) ) ;
#119391 = DIRECTION ( 'NONE',  ( -1.000000000000000000, 0.000000000000000000, 0.000000000000000000 ) ) ;
#119392 = ORIENTED_EDGE ( 'NONE', *, *, #34492, .F. ) ;
#119393 = DIRECTION ( 'NONE',  ( 0.000000000000000000, 0.000000000000000000, 1.000000000000000000 ) ) ;
#119394 = CARTESIAN_POINT ( 'NONE',  ( -7.950000000000009059, 2.500000000000000000, 6.495190528383297135 ) ) ;
#119395 = CARTESIAN_POINT ( 'NONE',  ( -14.79999999999998472, 2.500000000000000000, 0.3464101615137758494 ) ) ;
#119396 = EDGE_LOOP ( 'NONE', ( #17898, #117979, #90401, #23923 ) ) ;
#119397 = CARTESIAN_POINT ( 'NONE',  ( -3.300000000000027800, 2.500000000000000000, -4.430127018922202176 ) ) ;
#119398 = ORIENTED_EDGE ( 'NONE', *, *, #72322, .T. ) ;
#119399 = EDGE_LOOP ( 'NONE', ( #28038, #37432, #47792, #31448 ) ) ;
#119400 = LINE ( 'NONE', #70326, #126230 ) ;
#119401 = AXIS2_PLACEMENT_3D ( 'NONE', #79932, #103294, #64643 ) ;
#119402 = CIRCLE ( 'NONE', #79710, 0.06509327318403745899 ) ;
#119403 = EDGE_LOOP ( 'NONE', ( #107211, #22740 ) ) ;
#119404 = CARTESIAN_POINT ( 'NONE',  ( -8.100000000000013856, 12.50000000000000000, 0.3464101615137736845 ) ) ;
#119405 = DIRECTION ( 'NONE',  ( 0.000000000000000000, 1.000000000000000000, 0.000000000000000000 ) ) ;
#119406 = VERTEX_POINT ( 'NONE', #1403 ) ;
#119407 = EDGE_CURVE ( 'NONE', #98598, #97339, #106218, .T. ) ;
#119409 = CARTESIAN_POINT ( 'NONE',  ( -6.050000000000018474, 2.500000000000000000, 2.511473670974873507 ) ) ;
#119408 = VECTOR ( 'NONE', #5893, 1000.000000000000000 ) ;
#119410 = CIRCLE ( 'NONE', #115285, 0.1000000000000000472 ) ;
#119412 = VERTEX_POINT ( 'NONE', #112657 ) ;
#119411 = CARTESIAN_POINT ( 'NONE',  ( 10.84999999999991260, 2.500000000000000000, 5.902370205355745192 ) ) ;
#119413 = AXIS2_PLACEMENT_3D ( 'NONE', #108871, #57209, #107602 ) ;
#119414 = DIRECTION ( 'NONE',  ( 0.000000000000000000, 0.000000000000000000, -1.000000000000000000 ) ) ;
#119415 = EDGE_CURVE ( 'NONE', #54453, #35207, #89488, .T. ) ;
#119416 = EDGE_CURVE ( 'NONE', #51297, #32033, #122947, .T. ) ;
#119417 = VERTEX_POINT ( 'NONE', #62910 ) ;
#119418 = EDGE_LOOP ( 'NONE', ( #128259, #28415 ) ) ;
#119419 = ORIENTED_EDGE ( 'NONE', *, *, #33421, .F. ) ;
#119420 = CARTESIAN_POINT ( 'NONE',  ( 1.849999999999949685, 2.500000000000000000, 1.818653347947321475 ) ) ;
#119421 = DIRECTION ( 'NONE',  ( 0.000000000000000000, 1.000000000000000000, 0.000000000000000000 ) ) ;
#119422 = ADVANCED_FACE ( 'NONE', ( #2678 ), #13141, .T. ) ;
#119423 = EDGE_CURVE ( 'NONE', #54678, #8118, #53896, .T. ) ;
#119424 = DIRECTION ( 'NONE',  ( 0.000000000000000000, 0.000000000000000000, 1.000000000000000000 ) ) ;
#119425 = EDGE_CURVE ( 'NONE', #12097, #72485, #93022, .T. ) ;
#119426 = FACE_BOUND ( 'NONE', #83738, .T. ) ;
#119428 = ADVANCED_FACE ( 'NONE', ( #21706 ), #81094, .T. ) ;
#119427 = ORIENTED_EDGE ( 'NONE', *, *, #124164, .F. ) ;
#119429 = EDGE_CURVE ( 'NONE', #51134, #83059, #97801, .T. ) ;
#119430 = CARTESIAN_POINT ( 'NONE',  ( 108.0000000000000142, 8.500000000000000000, -0.2500000000000000000 ) ) ;
#119431 = LINE ( 'NONE', #109633, #52341 ) ;
#119432 = ORIENTED_EDGE ( 'NONE', *, *, #43362, .T. ) ;
#119433 = DIRECTION ( 'NONE',  ( -0.000000000000000000, 1.000000000000000000, -0.000000000000000000 ) ) ;
#119434 = FACE_OUTER_BOUND ( 'NONE', #106584, .T. ) ;
#119435 = DIRECTION ( 'NONE',  ( 0.000000000000000000, -0.9999939076577903929, 0.003490651415223739937 ) ) ;
#119436 = FACE_OUTER_BOUND ( 'NONE', #3947, .T. ) ;
#119437 = DIRECTION ( 'NONE',  ( -0.000000000000000000, 1.000000000000000000, -0.000000000000000000 ) ) ;
#119438 = ADVANCED_FACE ( 'NONE', ( #71419 ), #51814, .T. ) ;
#119439 = DIRECTION ( 'NONE',  ( 0.000000000000000000, 1.000000000000000000, 0.000000000000000000 ) ) ;
#119440 = DIRECTION ( 'NONE',  ( 0.000000000000000000, 0.000000000000000000, -1.000000000000000000 ) ) ;
#119441 = CIRCLE ( 'NONE', #117368, 0.06509327318403745899 ) ;
#119442 = CIRCLE ( 'NONE', #102710, 0.06509327318403745899 ) ;
#119443 = EDGE_LOOP ( 'NONE', ( #109989, #119650, #65295, #13691 ) ) ;
#119444 = EDGE_LOOP ( 'NONE', ( #110409, #44481, #24594, #59818 ) ) ;
#119445 = EDGE_LOOP ( 'NONE', ( #127111, #1878, #73644, #114121 ) ) ;
#119446 = ORIENTED_EDGE ( 'NONE', *, *, #3599, .F. ) ;
#119447 = ORIENTED_EDGE ( 'NONE', *, *, #71510, .T. ) ;
#119448 = FACE_OUTER_BOUND ( 'NONE', #74874, .T. ) ;
#119449 = DIRECTION ( 'NONE',  ( 0.000000000000000000, 0.000000000000000000, 1.000000000000000000 ) ) ;
#119450 = ORIENTED_EDGE ( 'NONE', *, *, #30492, .T. ) ;
#119451 = FACE_BOUND ( 'NONE', #30712, .T. ) ;
#119452 = CONICAL_SURFACE ( 'NONE', #23305, 0.1000000000000002554, 0.003490658503988666988 ) ;
#119453 = CARTESIAN_POINT ( 'NONE',  ( -12.29999999999999716, 2.500000000000000000, -3.983716857408423628 ) ) ;
#119454 = CONICAL_SURFACE ( 'NONE', #65068, 0.1000000000000000472, 0.003490658503988666988 ) ;
#119455 = VECTOR ( 'NONE', #58703, 1000.000000000000000 ) ;
#119456 = DIRECTION ( 'NONE',  ( -0.000000000000000000, -1.000000000000000000, -0.000000000000000000 ) ) ;
#119457 = DIRECTION ( 'NONE',  ( 0.000000000000000000, 0.000000000000000000, -1.000000000000000000 ) ) ;
#119458 = CARTESIAN_POINT ( 'NONE',  ( -2.900000000000030109, 2.500000000000000000, -3.637306695894650055 ) ) ;
#119459 = PLANE ( 'NONE',  #74225 ) ;
#119460 = FACE_OUTER_BOUND ( 'NONE', #63143, .T. ) ;
#119461 = VERTEX_POINT ( 'NONE', #3344 ) ;
#119462 = CIRCLE ( 'NONE', #106941, 0.1000000000000002554 ) ;
#119463 = VERTEX_POINT ( 'NONE', #14431 ) ;
#119464 = CIRCLE ( 'NONE', #8737, 0.06509327318403745899 ) ;
#119465 = ORIENTED_EDGE ( 'NONE', *, *, #912, .F. ) ;
#119466 = EDGE_LOOP ( 'NONE', ( #64071, #52936 ) ) ;
#119467 = VERTEX_POINT ( 'NONE', #3977 ) ;
#119468 = AXIS2_PLACEMENT_3D ( 'NONE', #87510, #117597, #97984 ) ;
#119469 = EDGE_CURVE ( 'NONE', #73868, #67061, #43540, .T. ) ;
#119470 = CARTESIAN_POINT ( 'NONE',  ( -12.89999999999999147, 2.500000000000000000, -4.430127018922199511 ) ) ;
#119471 = CARTESIAN_POINT ( 'NONE',  ( 10.84999999999990905, 2.500000000000000000, -6.395190528383301931 ) ) ;
#119472 = ADVANCED_FACE ( 'NONE', ( #106054 ), #18473, .T. ) ;
#119473 = ORIENTED_EDGE ( 'NONE', *, *, #84386, .F. ) ;
#119474 = CARTESIAN_POINT ( 'NONE',  ( -6.700000000000019718, 2.500000000000000000, 0.09999999999999761857 ) ) ;
#119475 = AXIS2_PLACEMENT_3D ( 'NONE', #111551, #31085, #90616 ) ;
#119476 = EDGE_CURVE ( 'NONE', #83800, #129352, #5261, .T. ) ;
#119477 = DIRECTION ( 'NONE',  ( 0.000000000000000000, 1.000000000000000000, 0.000000000000000000 ) ) ;
#119478 = EDGE_CURVE ( 'NONE', #54197, #109690, #104742, .T. ) ;
#119479 = CARTESIAN_POINT ( 'NONE',  ( -8.750000000000007105, 12.50000000000000000, 7.188010851410848723 ) ) ;
#119480 = CIRCLE ( 'NONE', #88065, 0.06509327318403745899 ) ;
#119482 = CARTESIAN_POINT ( 'NONE',  ( 185.9843750003414016, -8.734944146203032389, -1.604583208406768146E-15 ) ) ;
#119481 = ADVANCED_BREP_SHAPE_REPRESENTATION ( '', ( #58374, #108296 ), #79070 ) ;
#119483 = CARTESIAN_POINT ( 'NONE',  ( 5.649999999999932854, 2.500000000000000000, 1.818653347947321475 ) ) ;
#119484 = CARTESIAN_POINT ( 'NONE',  ( 13.14999999999989733, 12.50000000000000000, -1.753560074763288457 ) ) ;
#119485 = DIRECTION ( 'NONE',  ( 1.000000000000000000, 0.000000000000000000, -7.228014483236698281E-17 ) ) ;
#119486 = EDGE_CURVE ( 'NONE', #56423, #61621, #8001, .T. ) ;
#119487 = VERTEX_POINT ( 'NONE', #26208 ) ;
#119488 = DIRECTION ( 'NONE',  ( 0.000000000000000000, 0.000000000000000000, -1.000000000000000000 ) ) ;
#119489 = EDGE_CURVE ( 'NONE', #64836, #28738, #91633, .T. ) ;
#119490 = EDGE_CURVE ( 'NONE', #54227, #30984, #34758, .T. ) ;
#119491 = ORIENTED_EDGE ( 'NONE', *, *, #3762, .T. ) ;
#119492 = EDGE_CURVE ( 'NONE', #23452, #99397, #15057, .T. ) ;
#119493 = VERTEX_POINT ( 'NONE', #53731 ) ;
#119494 = CARTESIAN_POINT ( 'NONE',  ( -13.29999999999999005, 2.500000000000000000, -4.430127018922199511 ) ) ;
#119495 = FACE_OUTER_BOUND ( 'NONE', #80855, .T. ) ;
#119496 = DIRECTION ( 'NONE',  ( 0.000000000000000000, 0.000000000000000000, -1.000000000000000000 ) ) ;
#119497 = VERTEX_POINT ( 'NONE', #43929 ) ;
#119498 = EDGE_CURVE ( 'NONE', #122996, #2794, #103480, .T. ) ;
#119499 = VERTEX_POINT ( 'NONE', #16356 ) ;
#119500 = DIRECTION ( 'NONE',  ( -0.000000000000000000, 1.000000000000000000, -0.000000000000000000 ) ) ;
#119501 = DIRECTION ( 'NONE',  ( -0.000000000000000000, -1.000000000000000000, -0.000000000000000000 ) ) ;
#119502 = LINE ( 'NONE', #30515, #8035 ) ;
#119504 = DIRECTION ( 'NONE',  ( 0.000000000000000000, 0.000000000000000000, 1.000000000000000000 ) ) ;
#119503 = CONICAL_SURFACE ( 'NONE', #63076, 0.1000000000000000472, 0.003490658503988666988 ) ;
#119505 = ORIENTED_EDGE ( 'NONE', *, *, #33618, .F. ) ;
#119506 = CIRCLE ( 'NONE', #25403, 0.06509327318403741736 ) ;
#119507 = CIRCLE ( 'NONE', #46345, 0.09999999999999982514 ) ;
#119508 = DIRECTION ( 'NONE',  ( -0.000000000000000000, 1.000000000000000000, -0.000000000000000000 ) ) ;
#119509 = EDGE_LOOP ( 'NONE', ( #13467, #80101 ) ) ;
#119510 = DIRECTION ( 'NONE',  ( -0.000000000000000000, 1.000000000000000000, -0.000000000000000000 ) ) ;
#119511 = CIRCLE ( 'NONE', #35896, 0.1000000000000002554 ) ;
#119512 = ORIENTED_EDGE ( 'NONE', *, *, #114447, .T. ) ;
#119513 = DIRECTION ( 'NONE',  ( -0.000000000000000000, 1.000000000000000000, -0.000000000000000000 ) ) ;
#119514 = VECTOR ( 'NONE', #22611, 1000.000000000000000 ) ;
#119515 = DIRECTION ( 'NONE',  ( 0.000000000000000000, 1.000000000000000000, 0.000000000000000000 ) ) ;
#119516 = CARTESIAN_POINT ( 'NONE',  ( 10.64999999999990976, 2.500000000000000000, 2.511473670974873507 ) ) ;
#119517 = CIRCLE ( 'NONE', #81855, 0.1000000000000000472 ) ;
#119518 = ADVANCED_FACE ( 'NONE', ( #44560 ), #93690, .T. ) ;
#119519 = DIRECTION ( 'NONE',  ( 0.000000000000000000, 0.000000000000000000, 1.000000000000000000 ) ) ;
#119520 = ORIENTED_EDGE ( 'NONE', *, *, #48435, .T. ) ;
#119521 = VECTOR ( 'NONE', #58624, 1000.000000000000000 ) ;
#119522 = DIRECTION ( 'NONE',  ( 0.000000000000000000, 0.000000000000000000, 1.000000000000000000 ) ) ;
#119523 = VERTEX_POINT ( 'NONE', #55660 ) ;
#119524 = EDGE_LOOP ( 'NONE', ( #67348, #78199 ) ) ;
#119525 = DIRECTION ( 'NONE',  ( -0.000000000000000000, -1.000000000000000000, -0.000000000000000000 ) ) ;
#119526 = CARTESIAN_POINT ( 'NONE',  ( 1.849999999999950573, 2.500000000000000000, 2.611473670974873151 ) ) ;
#119527 = FACE_OUTER_BOUND ( 'NONE', #96045, .T. ) ;
#119528 = CARTESIAN_POINT ( 'NONE',  ( 187.0260416670080588, -6.551208109652273848, -3.782341765625003571 ) ) ;
#119529 = CARTESIAN_POINT ( 'NONE',  ( 8.549999999999922551, 2.500000000000000000, 2.511473670974873507 ) ) ;
#119530 = DIRECTION ( 'NONE',  ( 0.000000000000000000, 0.000000000000000000, 1.000000000000000000 ) ) ;
#119532 = ADVANCED_FACE ( 'NONE', ( #123738 ), #112576, .T. ) ;
#119531 = DIRECTION ( 'NONE',  ( 0.000000000000000000, 0.000000000000000000, -1.000000000000000000 ) ) ;
#119533 = CARTESIAN_POINT ( 'NONE',  ( 10.84999999999991260, 12.50000000000000000, 5.737276932171707422 ) ) ;
#119534 = CARTESIAN_POINT ( 'NONE',  ( 6.449999999999931788, 12.50000000000000000, -6.083687093685488989 ) ) ;
#119535 = CIRCLE ( 'NONE', #65243, 0.1000000000000002554 ) ;
#119536 = CONICAL_SURFACE ( 'NONE', #67274, 0.09999999999999982514, 0.003490658503988666988 ) ;
#119537 = ORIENTED_EDGE ( 'NONE', *, *, #107997, .T. ) ;
#119538 = DIRECTION ( 'NONE',  ( 0.000000000000000000, 0.000000000000000000, 1.000000000000000000 ) ) ;
#119539 = EDGE_CURVE ( 'NONE', #89688, #32515, #37275, .T. ) ;
#119540 = CARTESIAN_POINT ( 'NONE',  ( -10.45000000000000107, 2.500000000000000000, 2.165063509461097713 ) ) ;
#119541 = CARTESIAN_POINT ( 'NONE',  ( 9.599999999999917932, 2.500000000000000000, -2.276824562219559311E-15 ) ) ;
#119542 = DIRECTION ( 'NONE',  ( 0.000000000000000000, 0.000000000000000000, 1.000000000000000000 ) ) ;
#119543 = DIRECTION ( 'NONE',  ( 0.000000000000000000, -0.9999939076577903929, 0.003490651415223739937 ) ) ;
#119544 = VECTOR ( 'NONE', #83689, 1000.000000000000000 ) ;
#119545 = ORIENTED_EDGE ( 'NONE', *, *, #64008, .F. ) ;
#119546 = DIRECTION ( 'NONE',  ( 0.000000000000000000, 0.000000000000000000, -1.000000000000000000 ) ) ;
#119547 = AXIS2_PLACEMENT_3D ( 'NONE', #26343, #44692, #85877 ) ;
#119548 = AXIS2_PLACEMENT_3D ( 'NONE', #72398, #93319, #92670 ) ;
#119549 = CARTESIAN_POINT ( 'NONE',  ( 0.4499999999999573785, 12.50000000000000000, -6.495190528383302464 ) ) ;
#119551 = ORIENTED_EDGE ( 'NONE', *, *, #41172, .F. ) ;
#119550 = LINE ( 'NONE', #127457, #334 ) ;
#119552 = AXIS2_PLACEMENT_3D ( 'NONE', #24601, #4282, #64513 ) ;
#119553 = ORIENTED_EDGE ( 'NONE', *, *, #36681, .F. ) ;
#119554 = DIRECTION ( 'NONE',  ( 1.000000000000000000, -0.000000000000000000, -0.000000000000000000 ) ) ;
#119555 = ORIENTED_EDGE ( 'NONE', *, *, #90954, .T. ) ;
#119556 = VERTEX_POINT ( 'NONE', #35387 ) ;
#119558 = VERTEX_POINT ( 'NONE', #25538 ) ;
#119557 = CONICAL_SURFACE ( 'NONE', #84062, 0.09999999999999999167, 0.003490658503988666988 ) ;
#119559 = VECTOR ( 'NONE', #57342, 1000.000000000000000 ) ;
#119560 = DIRECTION ( 'NONE',  ( 0.000000000000000000, 0.000000000000000000, 1.000000000000000000 ) ) ;
#119561 = CIRCLE ( 'NONE', #111236, 0.1000000000000002554 ) ;
#119562 = CARTESIAN_POINT ( 'NONE',  ( 8.099999999999923261, 2.500000000000000000, -4.776537180435978414 ) ) ;
#119563 = CARTESIAN_POINT ( 'NONE',  ( -13.74999999999995381, 12.50000000000000000, 2.165063509461101265 ) ) ;
#119564 = DIRECTION ( 'NONE',  ( 0.000000000000000000, -0.000000000000000000, 1.000000000000000000 ) ) ;
#119565 = ORIENTED_EDGE ( 'NONE', *, *, #80193, .F. ) ;
#119566 = EDGE_CURVE ( 'NONE', #83925, #79983, #68651, .T. ) ;
#119567 = AXIS2_PLACEMENT_3D ( 'NONE', #112709, #110756, #23036 ) ;
#119568 = DIRECTION ( 'NONE',  ( 0.000000000000000000, 0.000000000000000000, 1.000000000000000000 ) ) ;
#119569 = ORIENTED_EDGE ( 'NONE', *, *, #41476, .F. ) ;
#119570 = DIRECTION ( 'NONE',  ( 0.000000000000000000, 1.000000000000000000, 0.000000000000000000 ) ) ;
#119571 = CARTESIAN_POINT ( 'NONE',  ( 19.08853762629104978, 0.5565172523999983856, 4.470057054643344685 ) ) ;
#119572 = DIRECTION ( 'NONE',  ( 0.000000000000000000, 0.000000000000000000, 1.000000000000000000 ) ) ;
#119573 = CARTESIAN_POINT ( 'NONE',  ( -5.200000000000022382, 2.500000000000000000, 0.3464101615137735735 ) ) ;
#119574 = ORIENTED_EDGE ( 'NONE', *, *, #13179, .T. ) ;
#119575 = ORIENTED_EDGE ( 'NONE', *, *, #86951, .F. ) ;
#119576 = VERTEX_POINT ( 'NONE', #45851 ) ;
#119577 = EDGE_LOOP ( 'NONE', ( #124461, #124903, #8688, #27103 ) ) ;
#119578 = ORIENTED_EDGE ( 'NONE', *, *, #79504, .F. ) ;
#119579 = DIRECTION ( 'NONE',  ( 0.000000000000000000, -0.000000000000000000, 1.000000000000000000 ) ) ;
#119580 = LINE ( 'NONE', #19456, #104162 ) ;
#119581 = ADVANCED_FACE ( 'NONE', ( #85757 ), #70705, .T. ) ;
#119582 = EDGE_CURVE ( 'NONE', #56299, #50883, #121595, .T. ) ;
#119583 = DIRECTION ( 'NONE',  ( -0.000000000000000000, -1.000000000000000000, -0.000000000000000000 ) ) ;
#119584 = EDGE_CURVE ( 'NONE', #110814, #51534, #85375, .T. ) ;
#119585 = FACE_BOUND ( 'NONE', #98401, .T. ) ;
#119586 = EDGE_CURVE ( 'NONE', #116584, #70542, #28957, .T. ) ;
#119587 = DIRECTION ( 'NONE',  ( 0.000000000000000000, 0.000000000000000000, 1.000000000000000000 ) ) ;
#119588 = CARTESIAN_POINT ( 'NONE',  ( 12.04999999999990834, 2.500000000000000000, -2.165063509461101710 ) ) ;
#119589 = DIRECTION ( 'NONE',  ( 0.000000000000000000, -0.000000000000000000, 1.000000000000000000 ) ) ;
#119590 = DIRECTION ( 'NONE',  ( 0.000000000000000000, 1.000000000000000000, 0.000000000000000000 ) ) ;
#119591 = AXIS2_PLACEMENT_3D ( 'NONE', #109118, #19464, #90786 ) ;
#119592 = AXIS2_PLACEMENT_3D ( 'NONE', #49162, #19016, #58964 ) ;
#119593 = CARTESIAN_POINT ( 'NONE',  ( -0.6500000000000394351, 12.50000000000000000, 6.841600689897072485 ) ) ;
#119594 = LINE ( 'NONE', #88859, #783 ) ;
#119595 = ADVANCED_FACE ( 'NONE', ( #33863 ), #108355, .T. ) ;
#119596 = DIRECTION ( 'NONE',  ( 0.000000000000000000, 0.000000000000000000, 1.000000000000000000 ) ) ;
#119597 = EDGE_CURVE ( 'NONE', #85559, #96252, #102104, .T. ) ;
#119599 = ADVANCED_FACE ( 'NONE', ( #43080 ), #123038, .T. ) ;
#119598 = VECTOR ( 'NONE', #42833, 1000.000000000000000 ) ;
#119601 = CARTESIAN_POINT ( 'NONE',  ( -7.700000000000012612, 12.50000000000000000, 4.676537180435972552 ) ) ;
#119600 = AXIS2_PLACEMENT_3D ( 'NONE', #2016, #41962, #62251 ) ;
#119602 = VECTOR ( 'NONE', #13723, 1000.000000000000000 ) ;
#119603 = VERTEX_POINT ( 'NONE', #14214 ) ;
#119604 = EDGE_LOOP ( 'NONE', ( #49738, #73200 ) ) ;
#119605 = ORIENTED_EDGE ( 'NONE', *, *, #127322, .T. ) ;
#119606 = ORIENTED_EDGE ( 'NONE', *, *, #72377, .T. ) ;
#119607 = CIRCLE ( 'NONE', #102873, 0.1000000000000000472 ) ;
#119608 = LINE ( 'NONE', #99988, #37644 ) ;
#119609 = VECTOR ( 'NONE', #77172, 1000.000000000000000 ) ;
#119610 = FACE_OUTER_BOUND ( 'NONE', #79797, .T. ) ;
#119611 = FACE_BOUND ( 'NONE', #78693, .T. ) ;
#119612 = AXIS2_PLACEMENT_3D ( 'NONE', #54187, #15526, #45013 ) ;
#119613 = DIRECTION ( 'NONE',  ( 0.000000000000000000, 0.000000000000000000, 1.000000000000000000 ) ) ;
#119614 = ORIENTED_EDGE ( 'NONE', *, *, #31895, .T. ) ;
#119615 = CARTESIAN_POINT ( 'NONE',  ( -13.94999999999998685, 2.500000000000000000, -2.411473670974875638 ) ) ;
#119616 = DIRECTION ( 'NONE',  ( 0.000000000000000000, 1.000000000000000000, 0.000000000000000000 ) ) ;
#119617 = DIRECTION ( 'NONE',  ( -0.000000000000000000, 1.000000000000000000, -0.000000000000000000 ) ) ;
#119618 = CARTESIAN_POINT ( 'NONE',  ( 6.449999999999931788, 2.500000000000000000, 6.148780366869520009 ) ) ;
#119619 = ORIENTED_EDGE ( 'NONE', *, *, #12192, .T. ) ;
#119620 = FACE_OUTER_BOUND ( 'NONE', #103337, .T. ) ;
#119621 = ORIENTED_EDGE ( 'NONE', *, *, #3509, .T. ) ;
#119622 = ORIENTED_EDGE ( 'NONE', *, *, #108875, .F. ) ;
#119623 = CARTESIAN_POINT ( 'NONE',  ( 1.249999999999950262, 2.500000000000000000, 7.088010851410848190 ) ) ;
#119624 = FACE_OUTER_BOUND ( 'NONE', #82823, .T. ) ;
#119625 = ORIENTED_EDGE ( 'NONE', *, *, #59498, .F. ) ;
#119626 = AXIS2_PLACEMENT_3D ( 'NONE', #80127, #68360, #18622 ) ;
#119627 = CARTESIAN_POINT ( 'NONE',  ( -10.40000000000000213, 12.50000000000000000, 0.6277270498435120194 ) ) ;
#119628 = CARTESIAN_POINT ( 'NONE',  ( -7.100000000000017408, 2.500000000000000000, -5.022947341949754119 ) ) ;
#119629 = ORIENTED_EDGE ( 'NONE', *, *, #124723, .T. ) ;
#119630 = CARTESIAN_POINT ( 'NONE',  ( -0.4000000000000396572, 2.500000000000000000, 4.330127018922196314 ) ) ;
#119631 = VERTEX_POINT ( 'NONE', #120960 ) ;
#119632 = FACE_OUTER_BOUND ( 'NONE', #40468, .T. ) ;
#119633 = EDGE_CURVE ( 'NONE', #15440, #82143, #24742, .T. ) ;
#119634 = ORIENTED_EDGE ( 'NONE', *, *, #109735, .F. ) ;
#119635 = CARTESIAN_POINT ( 'NONE',  ( 0.8499999999999557909, 2.500000000000000000, -6.495190528383302464 ) ) ;
#119636 = CIRCLE ( 'NONE', #63213, 3.000000000000000000 ) ;
#119637 = EDGE_CURVE ( 'NONE', #120463, #78289, #92139, .T. ) ;
#119638 = AXIS2_PLACEMENT_3D ( 'NONE', #70870, #70227, #110779 ) ;
#119639 = EDGE_LOOP ( 'NONE', ( #48242, #59720, #74820, #117331 ) ) ;
#119640 = CONICAL_SURFACE ( 'NONE', #98806, 0.09999999999999982514, 0.003490658503988666988 ) ;
#119642 = ADVANCED_FACE ( 'NONE', ( #11652 ), #113066, .T. ) ;
#119641 = DIRECTION ( 'NONE',  ( 0.000000000000000000, 0.000000000000000000, -1.000000000000000000 ) ) ;
#119643 = ORIENTED_EDGE ( 'NONE', *, *, #82552, .F. ) ;
#119644 = DIRECTION ( 'NONE',  ( 0.000000000000000000, 0.000000000000000000, 1.000000000000000000 ) ) ;
#119645 = DIRECTION ( 'NONE',  ( -0.000000000000000000, 1.000000000000000000, -0.000000000000000000 ) ) ;
#119646 = DIRECTION ( 'NONE',  ( 0.000000000000000000, 0.000000000000000000, 1.000000000000000000 ) ) ;
#119647 = CARTESIAN_POINT ( 'NONE',  ( -6.250000000000015987, 12.50000000000000000, 1.472243186433545459 ) ) ;
#119648 = DIRECTION ( 'NONE',  ( 0.000000000000000000, 0.000000000000000000, 1.000000000000000000 ) ) ;
#119649 = CIRCLE ( 'NONE', #59031, 0.06509327318403741736 ) ;
#119650 = ORIENTED_EDGE ( 'NONE', *, *, #40572, .T. ) ;
#119651 = EDGE_CURVE ( 'NONE', #91958, #93869, #99956, .T. ) ;
#119652 = ORIENTED_EDGE ( 'NONE', *, *, #78886, .T. ) ;
#119653 = AXIS2_PLACEMENT_3D ( 'NONE', #52468, #13173, #75330 ) ;
#119654 = EDGE_LOOP ( 'NONE', ( #62264, #2149, #121841, #99206 ) ) ;
#119655 = FACE_OUTER_BOUND ( 'NONE', #23182, .T. ) ;
#119657 = VECTOR ( 'NONE', #22302, 1000.000000000000000 ) ;
#119656 = DIRECTION ( 'NONE',  ( 0.000000000000000000, 1.000000000000000000, 0.000000000000000000 ) ) ;
#119658 = CIRCLE ( 'NONE', #127981, 0.09999999999999982514 ) ;
#119659 = CARTESIAN_POINT ( 'NONE',  ( 8.549999999999918998, 2.500000000000000000, -1.818653347947326138 ) ) ;
#119661 = ORIENTED_EDGE ( 'NONE', *, *, #101620, .T. ) ;
#119660 = ORIENTED_EDGE ( 'NONE', *, *, #62147, .T. ) ;
#119662 = ORIENTED_EDGE ( 'NONE', *, *, #120180, .T. ) ;
#119663 = DIRECTION ( 'NONE',  ( 0.000000000000000000, 1.000000000000000000, 0.000000000000000000 ) ) ;
#119664 = CIRCLE ( 'NONE', #107137, 0.06509327318403745899 ) ;
#119665 = EDGE_LOOP ( 'NONE', ( #39709, #10893 ) ) ;
#119666 = CARTESIAN_POINT ( 'NONE',  ( -1.050000000000037348, 2.500000000000000000, -2.511473670974877948 ) ) ;
#119667 = DIRECTION ( 'NONE',  ( 0.000000000000000000, 1.000000000000000000, 0.000000000000000000 ) ) ;
#119668 = AXIS2_PLACEMENT_3D ( 'NONE', #49781, #47842, #87095 ) ;
#119669 = CARTESIAN_POINT ( 'NONE',  ( 13.94999999999989626, 12.50000000000000000, 2.511473670974873507 ) ) ;
#119670 = CARTESIAN_POINT ( 'NONE',  ( -10.45000000000000462, 2.500000000000000000, -6.395190528383298378 ) ) ;
#119671 = DIRECTION ( 'NONE',  ( 0.000000000000000000, 0.000000000000000000, 1.000000000000000000 ) ) ;
#119672 = CARTESIAN_POINT ( 'NONE',  ( -6.850000000000013856, 2.500000000000000000, 2.511473670974873507 ) ) ;
#119673 = DIRECTION ( 'NONE',  ( 0.000000000000000000, 0.000000000000000000, 1.000000000000000000 ) ) ;
#119674 = EDGE_LOOP ( 'NONE', ( #100736, #110049, #90427, #77985 ) ) ;
#119675 = ORIENTED_EDGE ( 'NONE', *, *, #81486, .T. ) ;
#119676 = CARTESIAN_POINT ( 'NONE',  ( -14.14999999999998614, 2.500000000000000000, -2.165063509461099489 ) ) ;
#119677 = ORIENTED_EDGE ( 'NONE', *, *, #128961, .F. ) ;
#119678 = ORIENTED_EDGE ( 'NONE', *, *, #62292, .T. ) ;
#119679 = AXIS2_PLACEMENT_3D ( 'NONE', #94417, #114706, #25047 ) ;
#119680 = CARTESIAN_POINT ( 'NONE',  ( 185.5677083336747160, -4.367472073101514418, -7.564683531250002702 ) ) ;
#119681 = DIRECTION ( 'NONE',  ( 0.000000000000000000, 0.000000000000000000, 1.000000000000000000 ) ) ;
#119682 = DIRECTION ( 'NONE',  ( 0.000000000000000000, 1.000000000000000000, 0.000000000000000000 ) ) ;
#119683 = DIRECTION ( 'NONE',  ( 0.000000000000000000, 0.000000000000000000, 1.000000000000000000 ) ) ;
#119684 = CARTESIAN_POINT ( 'NONE',  ( 3.149999999999946176, 12.50000000000000000, -6.148780366869526226 ) ) ;
#119685 = ADVANCED_FACE ( 'NONE', ( #31953 ), #111116, .T. ) ;
#119686 = CONICAL_SURFACE ( 'NONE', #128108, 0.1000000000000002554, 0.003490658503988666988 ) ;
#119687 = CARTESIAN_POINT ( 'NONE',  ( 4.149999999999938183, 2.500000000000000000, 2.265063509461097357 ) ) ;
#119688 = CARTESIAN_POINT ( 'NONE',  ( 8.149999999999923972, 12.50000000000000000, -6.148780366869526226 ) ) ;
#119689 = AXIS2_PLACEMENT_3D ( 'NONE', #22277, #34011, #91638 ) ;
#119690 = AXIS2_PLACEMENT_3D ( 'NONE', #85078, #15017, #115152 ) ;
#119691 = DIRECTION ( 'NONE',  ( -0.000000000000000000, -1.000000000000000000, -0.000000000000000000 ) ) ;
#119692 = AXIS2_PLACEMENT_3D ( 'NONE', #23576, #6474, #34050 ) ;
#119693 = ORIENTED_EDGE ( 'NONE', *, *, #71457, .F. ) ;
#119694 = AXIS2_PLACEMENT_3D ( 'NONE', #54204, #11690, #23444 ) ;
#119695 = AXIS2_PLACEMENT_3D ( 'NONE', #63853, #103778, #101203 ) ;
#119696 = VERTEX_POINT ( 'NONE', #112446 ) ;
#119698 = ADVANCED_FACE ( 'NONE', ( #61419 ), #49890, .T. ) ;
#119697 = CIRCLE ( 'NONE', #73722, 0.1000000000000002554 ) ;
#119699 = CIRCLE ( 'NONE', #73725, 0.1000000000000002554 ) ;
#119700 = VERTEX_POINT ( 'NONE', #91503 ) ;
#119702 = ORIENTED_EDGE ( 'NONE', *, *, #26984, .T. ) ;
#119701 = ADVANCED_FACE ( 'NONE', ( #22785 ), #71878, .T. ) ;
#119703 = DIRECTION ( 'NONE',  ( 0.000000000000000000, 1.000000000000000000, 0.000000000000000000 ) ) ;
#119704 = LINE ( 'NONE', #58234, #81279 ) ;
#119705 = AXIS2_PLACEMENT_3D ( 'NONE', #51464, #42279, #22649 ) ;
#119706 = ORIENTED_EDGE ( 'NONE', *, *, #93035, .F. ) ;
#119707 = CARTESIAN_POINT ( 'NONE',  ( -11.44999999999999751, 2.500000000000000000, 6.741600689897071952 ) ) ;
#119708 = CARTESIAN_POINT ( 'NONE',  ( -4.999999999999986677, 12.50000000000000000, 4.330127018922196314 ) ) ;
#119709 = DIRECTION ( 'NONE',  ( -4.274815082592931898E-19, -0.9999939076577903929, -0.003490651415223739937 ) ) ;
#119711 = ORIENTED_EDGE ( 'NONE', *, *, #84438, .F. ) ;
#119710 = CARTESIAN_POINT ( 'NONE',  ( -4.400000000000025224, 2.500000000000000000, -0.3464101615137783474 ) ) ;
#119712 = ADVANCED_FACE ( 'NONE', ( #63334 ), #53987, .T. ) ;
#119713 = CARTESIAN_POINT ( 'NONE',  ( -3.150000000000029665, 2.500000000000000000, 6.941600689897073018 ) ) ;
#119715 = CARTESIAN_POINT ( 'NONE',  ( 175.5000000000000000, 0.000000000000000000, 1.500000000000000000 ) ) ;
#119714 = CONICAL_SURFACE ( 'NONE', #4773, 0.1000000000000000472, 0.003490658503988666988 ) ;
#119716 = EDGE_LOOP ( 'NONE', ( #26523, #17020 ) ) ;
#119717 = EDGE_LOOP ( 'NONE', ( #66957, #20576, #111075, #23872 ) ) ;
#119718 = EDGE_LOOP ( 'NONE', ( #20522, #77836 ) ) ;
#119719 = VERTEX_POINT ( 'NONE', #12283 ) ;
#119720 = CARTESIAN_POINT ( 'NONE',  ( 16.56576425165006583, -1.500000000000000666, 6.084390597445813675 ) ) ;
#119722 = CIRCLE ( 'NONE', #111393, 0.06509327318403745899 ) ;
#119721 = CARTESIAN_POINT ( 'NONE',  ( 4.799999999999935874, 2.500000000000000000, 0.4464101615137735513 ) ) ;
#119723 = CARTESIAN_POINT ( 'NONE',  ( -3.150000000000032330, 2.500000000000000000, -6.148780366869526226 ) ) ;
#119724 = AXIS2_PLACEMENT_3D ( 'NONE', #112068, #23681, #43337 ) ;
#119725 = ADVANCED_FACE ( 'NONE', ( #42418 ), #104154, .T. ) ;
#119726 = VERTEX_POINT ( 'NONE', #43717 ) ;
#119727 = DIRECTION ( 'NONE',  ( 0.000000000000000000, 0.000000000000000000, 1.000000000000000000 ) ) ;
#119728 = CARTESIAN_POINT ( 'NONE',  ( 3.349999999999941913, 2.500000000000000000, 6.395190528383296602 ) ) ;
#119729 = PLANE ( 'NONE',  #127829 ) ;
#119730 = PLANE ( 'NONE',  #67195 ) ;
#119731 = AXIS2_PLACEMENT_3D ( 'NONE', #20270, #79208, #60223 ) ;
#119732 = VECTOR ( 'NONE', #108578, 1000.000000000000000 ) ;
#119734 = ADVANCED_FACE ( 'NONE', ( #6314 ), #120874, .T. ) ;
#119733 = VECTOR ( 'NONE', #77945, 1000.000000000000000 ) ;
#119735 = ORIENTED_EDGE ( 'NONE', *, *, #97767, .F. ) ;
#119736 = LINE ( 'NONE', #73064, #112704 ) ;
#119737 = CIRCLE ( 'NONE', #100958, 0.09999999999999982514 ) ;
#119738 = ORIENTED_EDGE ( 'NONE', *, *, #18192, .T. ) ;
#119739 = ORIENTED_EDGE ( 'NONE', *, *, #17297, .T. ) ;
#119740 = DIRECTION ( 'NONE',  ( -0.000000000000000000, 1.000000000000000000, -0.000000000000000000 ) ) ;
#119741 = EDGE_CURVE ( 'NONE', #112974, #20780, #64441, .T. ) ;
#119742 = EDGE_CURVE ( 'NONE', #128672, #101827, #74918, .T. ) ;
#119743 = CARTESIAN_POINT ( 'NONE',  ( -2.100000000000033396, 2.500000000000000000, -0.6928203230275542523 ) ) ;
#119744 = EDGE_CURVE ( 'NONE', #75000, #124476, #86165, .T. ) ;
#119745 = FACE_BOUND ( 'NONE', #34269, .T. ) ;
#119746 = ADVANCED_FACE ( 'NONE', ( #116282 ), #49992, .T. ) ;
#119747 = LINE ( 'NONE', #30754, #17884 ) ;
#119749 = DIRECTION ( 'NONE',  ( 0.000000000000000000, 1.000000000000000000, 0.000000000000000000 ) ) ;
#119748 = AXIS2_PLACEMENT_3D ( 'NONE', #4458, #71285, #32043 ) ;
#119751 = DIRECTION ( 'NONE',  ( -0.000000000000000000, -1.000000000000000000, -0.000000000000000000 ) ) ;
#119750 = CONICAL_SURFACE ( 'NONE', #19394, 0.1000000000000002554, 0.003490658503988666988 ) ;
#119752 = CIRCLE ( 'NONE', #33991, 0.1000000000000002554 ) ;
#119753 = ADVANCED_FACE ( 'NONE', ( #24702 ), #4378, .T. ) ;
#119754 = CARTESIAN_POINT ( 'NONE',  ( 0.6499999999999561684, 12.50000000000000000, 1.883746621131358934 ) ) ;
#119755 = DIRECTION ( 'NONE',  ( 0.000000000000000000, 0.000000000000000000, 1.000000000000000000 ) ) ;
#119756 = EDGE_CURVE ( 'NONE', #29817, #62380, #41581, .T. ) ;
#119757 = DIRECTION ( 'NONE',  ( 0.000000000000000000, 1.000000000000000000, 0.000000000000000000 ) ) ;
#119758 = AXIS2_PLACEMENT_3D ( 'NONE', #103198, #13517, #53469 ) ;
#119759 = CARTESIAN_POINT ( 'NONE',  ( 4.399999999999939071, 2.500000000000000000, -0.2464101615137782308 ) ) ;
#119760 = VERTEX_POINT ( 'NONE', #115639 ) ;
#119761 = CARTESIAN_POINT ( 'NONE',  ( -1.450000000000035927, 2.500000000000000000, -6.148780366869526226 ) ) ;
#119762 = EDGE_CURVE ( 'NONE', #43692, #129541, #64528, .T. ) ;
#119763 = ADVANCED_FACE ( 'NONE', ( #77016 ), #31112, .T. ) ;
#119764 = FACE_OUTER_BOUND ( 'NONE', #68984, .T. ) ;
#119765 = AXIS2_PLACEMENT_3D ( 'NONE', #121555, #31908, #92099 ) ;
#119766 = VERTEX_POINT ( 'NONE', #34541 ) ;
#119767 = ORIENTED_EDGE ( 'NONE', *, *, #105442, .T. ) ;
#119768 = DIRECTION ( 'NONE',  ( -0.000000000000000000, -1.000000000000000000, -0.000000000000000000 ) ) ;
#119769 = EDGE_CURVE ( 'NONE', #74448, #44266, #52032, .T. ) ;
#119770 = CARTESIAN_POINT ( 'NONE',  ( 10.59999999999990905, 12.50000000000000000, 3.918623584224382839 ) ) ;
#119771 = FACE_BOUND ( 'NONE', #123071, .T. ) ;
#119772 = EDGE_CURVE ( 'NONE', #103467, #39602, #60356, .T. ) ;
#119773 = DIRECTION ( 'NONE',  ( -0.000000000000000000, 1.000000000000000000, -0.000000000000000000 ) ) ;
#119774 = DIRECTION ( 'NONE',  ( 0.000000000000000000, -0.000000000000000000, 1.000000000000000000 ) ) ;
#119776 = VERTEX_POINT ( 'NONE', #116923 ) ;
#119775 = CONICAL_SURFACE ( 'NONE', #88361, 0.1000000000000000472, 0.003490658503988666988 ) ;
#119778 = CIRCLE ( 'NONE', #40378, 0.09999999999999982514 ) ;
#119777 = DIRECTION ( 'NONE',  ( 0.000000000000000000, 0.000000000000000000, 1.000000000000000000 ) ) ;
#119779 = CARTESIAN_POINT ( 'NONE',  ( 4.999999999999936939, 2.500000000000000000, -3.637306695894650055 ) ) ;
#119780 = ORIENTED_EDGE ( 'NONE', *, *, #103535, .F. ) ;
#119781 = DIRECTION ( 'NONE',  ( 0.000000000000000000, 1.000000000000000000, 0.000000000000000000 ) ) ;
#119782 = CARTESIAN_POINT ( 'NONE',  ( -7.300000000000014921, 2.500000000000000000, 4.676537180435972552 ) ) ;
#119783 = AXIS2_PLACEMENT_3D ( 'NONE', #71113, #120860, #29911 ) ;
#119784 = AXIS2_PLACEMENT_3D ( 'NONE', #65389, #47062, #96144 ) ;
#119785 = CIRCLE ( 'NONE', #48699, 0.1000000000000000472 ) ;
#119786 = CARTESIAN_POINT ( 'NONE',  ( 185.6979166673494603, 6.668395609140176816, 3.850000000000000977 ) ) ;
#119787 = DIRECTION ( 'NONE',  ( 0.000000000000000000, 1.000000000000000000, 0.000000000000000000 ) ) ;
#119788 = AXIS2_PLACEMENT_3D ( 'NONE', #87187, #48576, #101 ) ;
#119790 = ORIENTED_EDGE ( 'NONE', *, *, #86536, .T. ) ;
#119789 = AXIS2_PLACEMENT_3D ( 'NONE', #100558, #112324, #62588 ) ;
#119791 = VECTOR ( 'NONE', #92563, 1000.000000000000000 ) ;
#119792 = CARTESIAN_POINT ( 'NONE',  ( -5.400000000000019895, 2.500000000000000000, 4.430127018922196847 ) ) ;
#119793 = LINE ( 'NONE', #49145, #14277 ) ;
#119794 = CARTESIAN_POINT ( 'NONE',  ( 6.249999999999967137, 2.500000000000000000, -2.265063509461101798 ) ) ;
#119795 = AXIS2_PLACEMENT_3D ( 'NONE', #92788, #90842, #1171 ) ;
#119796 = DIRECTION ( 'NONE',  ( 0.000000000000000000, 0.000000000000000000, -1.000000000000000000 ) ) ;
#119798 = ORIENTED_EDGE ( 'NONE', *, *, #113394, .F. ) ;
#119797 = AXIS2_PLACEMENT_3D ( 'NONE', #84598, #13907, #55776 ) ;
#119799 = ORIENTED_EDGE ( 'NONE', *, *, #14574, .F. ) ;
#119800 = CARTESIAN_POINT ( 'NONE',  ( 12.49999999999990585, 12.50000000000000000, 3.637306695894644726 ) ) ;
#119801 = AXIS2_PLACEMENT_3D ( 'NONE', #45988, #125803, #36167 ) ;
#119802 = ORIENTED_EDGE ( 'NONE', *, *, #28589, .F. ) ;
#119803 = DIRECTION ( 'NONE',  ( -0.000000000000000000, 1.000000000000000000, -0.000000000000000000 ) ) ;
#119804 = CARTESIAN_POINT ( 'NONE',  ( 87.50000000000001421, -7.032605354647523122, 2.693424153406290600 ) ) ;
#119805 = EDGE_CURVE ( 'NONE', #44454, #108519, #56704, .T. ) ;
#119806 = LINE ( 'NONE', #38700, #92649 ) ;
#119807 = ORIENTED_EDGE ( 'NONE', *, *, #101348, .F. ) ;
#119809 = ADVANCED_FACE ( 'NONE', ( #16779 ), #102203, .T. ) ;
#119808 = DIRECTION ( 'NONE',  ( -4.274815082592931898E-19, -0.9999939076577903929, -0.003490651415223739937 ) ) ;
#119810 = DIRECTION ( 'NONE',  ( 0.000000000000000000, 0.000000000000000000, -1.000000000000000000 ) ) ;
#119811 = CARTESIAN_POINT ( 'NONE',  ( 1.249999999999952482, 2.500000000000000000, -5.802370205355749988 ) ) ;
#119812 = CARTESIAN_POINT ( 'NONE',  ( -10.20000000000000462, 2.500000000000000000, -4.576537180435972907 ) ) ;
#119813 = DIRECTION ( 'NONE',  ( 0.000000000000000000, 1.000000000000000000, 0.000000000000000000 ) ) ;
#119814 = CARTESIAN_POINT ( 'NONE',  ( -6.250000000000019540, 12.50000000000000000, -7.188010851410854052 ) ) ;
#119815 = AXIS2_PLACEMENT_3D ( 'NONE', #71441, #59731, #122 ) ;
#119816 = ORIENTED_EDGE ( 'NONE', *, *, #73, .F. ) ;
#119817 = EDGE_LOOP ( 'NONE', ( #43061, #125838 ) ) ;
#119818 = DIRECTION ( 'NONE',  ( 0.000000000000000000, 1.000000000000000000, 0.000000000000000000 ) ) ;
#119819 = VERTEX_POINT ( 'NONE', #54786 ) ;
#119820 = CARTESIAN_POINT ( 'NONE',  ( 17.50000000000000000, 2.500000000000000000, 4.000000000000000888 ) ) ;
#119822 = VERTEX_POINT ( 'NONE', #94718 ) ;
#119821 = ORIENTED_EDGE ( 'NONE', *, *, #9936, .F. ) ;
#119823 = VERTEX_POINT ( 'NONE', #124836 ) ;
#119824 = DIRECTION ( 'NONE',  ( -4.274815082592931898E-19, -0.9999939076577903929, -0.003490651415223739937 ) ) ;
#119825 = CONICAL_SURFACE ( 'NONE', #103099, 0.1000000000000002554, 0.003490658503988666988 ) ;
#119826 = DIRECTION ( 'NONE',  ( 0.000000000000000000, -0.000000000000000000, 1.000000000000000000 ) ) ;
#119827 = CIRCLE ( 'NONE', #63397, 0.09999999999999982514 ) ;
#119828 = FACE_OUTER_BOUND ( 'NONE', #17955, .T. ) ;
#119829 = FACE_OUTER_BOUND ( 'NONE', #85666, .T. ) ;
#119830 = DIRECTION ( 'NONE',  ( -4.274815082592931898E-19, -0.9999939076577903929, -0.003490651415223739937 ) ) ;
#119831 = DIRECTION ( 'NONE',  ( -0.000000000000000000, 1.000000000000000000, -0.000000000000000000 ) ) ;
#119832 = CARTESIAN_POINT ( 'NONE',  ( -3.350000000000031619, 2.500000000000000000, -5.802370205355749988 ) ) ;
#119833 = LINE ( 'NONE', #50447, #84266 ) ;
#119834 = VECTOR ( 'NONE', #35894, 1000.000000000000000 ) ;
#119835 = AXIS2_PLACEMENT_3D ( 'NONE', #105842, #26641, #35189 ) ;
#119836 = CARTESIAN_POINT ( 'NONE',  ( 6.249999999999932498, 2.500000000000000000, -5.902370205355750521 ) ) ;
#119837 = ORIENTED_EDGE ( 'NONE', *, *, #95058, .T. ) ;
#119838 = VECTOR ( 'NONE', #128708, 1000.000000000000000 ) ;
#119839 = ORIENTED_EDGE ( 'NONE', *, *, #93634, .T. ) ;
#119840 = AXIS2_PLACEMENT_3D ( 'NONE', #65465, #58721, #105404 ) ;
#119841 = DIRECTION ( 'NONE',  ( 0.000000000000000000, 1.000000000000000000, 0.000000000000000000 ) ) ;
#119842 = ORIENTED_EDGE ( 'NONE', *, *, #106983, .T. ) ;
#119843 = ORIENTED_EDGE ( 'NONE', *, *, #24299, .F. ) ;
#119844 = DIRECTION ( 'NONE',  ( 0.000000000000000000, 0.000000000000000000, -1.000000000000000000 ) ) ;
#119845 = DIRECTION ( 'NONE',  ( 0.000000000000000000, 0.000000000000000000, 1.000000000000000000 ) ) ;
#119846 = EDGE_CURVE ( 'NONE', #34866, #28525, #35180, .T. ) ;
#119847 = CARTESIAN_POINT ( 'NONE',  ( 186.8645833340161175, -6.668395609140180369, 3.849999999999994760 ) ) ;
#119848 = FACE_OUTER_BOUND ( 'NONE', #107885, .T. ) ;
#119849 = CONICAL_SURFACE ( 'NONE', #17423, 0.1000000000000002554, 0.003490658503988666988 ) ;
#119850 = DIRECTION ( 'NONE',  ( -0.000000000000000000, -1.000000000000000000, -0.000000000000000000 ) ) ;
#119851 = AXIS2_PLACEMENT_3D ( 'NONE', #80103, #38918, #89271 ) ;
#119852 = AXIS2_PLACEMENT_3D ( 'NONE', #71857, #101955, #10346 ) ;
#119853 = DIRECTION ( 'NONE',  ( 0.000000000000000000, 0.000000000000000000, -1.000000000000000000 ) ) ;
#119854 = EDGE_LOOP ( 'NONE', ( #99851, #91440 ) ) ;
#119855 = AXIS2_PLACEMENT_3D ( 'NONE', #48808, #30463, #119449 ) ;
#119856 = ORIENTED_EDGE ( 'NONE', *, *, #85888, .F. ) ;
#119857 = DIRECTION ( 'NONE',  ( -0.000000000000000000, 1.000000000000000000, -0.000000000000000000 ) ) ;
#119858 = ORIENTED_EDGE ( 'NONE', *, *, #90194, .F. ) ;
#119859 = CARTESIAN_POINT ( 'NONE',  ( -9.999999999999969802, 12.50000000000000000, -2.276824562219559311E-15 ) ) ;
#119860 = ORIENTED_EDGE ( 'NONE', *, *, #108587, .F. ) ;
#119861 = ADVANCED_FACE ( 'NONE', ( #65245 ), #85460, .T. ) ;
#119862 = EDGE_CURVE ( 'NONE', #93340, #110466, #127249, .T. ) ;
#119863 = ORIENTED_EDGE ( 'NONE', *, *, #65688, .F. ) ;
#119864 = DIRECTION ( 'NONE',  ( -0.000000000000000000, -1.000000000000000000, -0.000000000000000000 ) ) ;
#119865 = DIRECTION ( 'NONE',  ( -4.274815082592931898E-19, -0.9999939076577903929, -0.003490651415223739937 ) ) ;
#119866 = DIRECTION ( 'NONE',  ( 0.000000000000000000, 0.000000000000000000, 1.000000000000000000 ) ) ;
#119867 = DIRECTION ( 'NONE',  ( -0.000000000000000000, 1.000000000000000000, -0.000000000000000000 ) ) ;
#119868 = CARTESIAN_POINT ( 'NONE',  ( 17.50000000000000000, 0.4166666666666649088, 4.000000000000000888 ) ) ;
#119869 = VERTEX_POINT ( 'NONE', #5683 ) ;
#119870 = DIRECTION ( 'NONE',  ( 0.000000000000000000, 1.000000000000000000, 0.000000000000000000 ) ) ;
#119872 = AXIS2_PLACEMENT_3D ( 'NONE', #73959, #113889, #102760 ) ;
#119871 = DIRECTION ( 'NONE',  ( 0.000000000000000000, -0.9999939076577903929, 0.003490651415223739937 ) ) ;
#119873 = AXIS2_PLACEMENT_3D ( 'NONE', #58651, #78942, #109011 ) ;
#119874 = EDGE_CURVE ( 'NONE', #16094, #8551, #72955, .T. ) ;
#119875 = CARTESIAN_POINT ( 'NONE',  ( -8.950000000000009948, 12.50000000000000000, 2.511473670974873507 ) ) ;
#119876 = FACE_OUTER_BOUND ( 'NONE', #105382, .T. ) ;
#119877 = DIRECTION ( 'NONE',  ( 0.000000000000000000, 0.000000000000000000, -1.000000000000000000 ) ) ;
#119878 = VERTEX_POINT ( 'NONE', #50151 ) ;
#119879 = AXIS2_PLACEMENT_3D ( 'NONE', #37000, #126668, #8165 ) ;
#119880 = CONICAL_SURFACE ( 'NONE', #80172, 0.09999999999999982514, 0.003490658503988666988 ) ;
#119881 = AXIS2_PLACEMENT_3D ( 'NONE', #18838, #26735, #58140 ) ;
#119882 = ORIENTED_EDGE ( 'NONE', *, *, #81357, .T. ) ;
#119883 = CIRCLE ( 'NONE', #107352, 0.06509327318403745899 ) ;
#119884 = AXIS2_PLACEMENT_3D ( 'NONE', #99108, #88632, #49375 ) ;
#119885 = CARTESIAN_POINT ( 'NONE',  ( 2.499999999999947153, 2.500000000000000000, -3.737306695894649700 ) ) ;
#119886 = ORIENTED_EDGE ( 'NONE', *, *, #93776, .F. ) ;
#119887 = DIRECTION ( 'NONE',  ( -4.274815082592931898E-19, -0.9999939076577903929, -0.003490651415223739937 ) ) ;
#119888 = LINE ( 'NONE', #70784, #92017 ) ;
#119889 = CONICAL_SURFACE ( 'NONE', #57195, 0.1000000000000002554, 0.003490658503988666988 ) ;
#119890 = CIRCLE ( 'NONE', #13265, 0.06509327318403745899 ) ;
#119891 = VECTOR ( 'NONE', #99663, 1000.000000000000000 ) ;
#119892 = AXIS2_PLACEMENT_3D ( 'NONE', #46910, #86817, #105821 ) ;
#119893 = CONICAL_SURFACE ( 'NONE', #80102, 0.09999999999999999167, 0.003490658503988666988 ) ;
#119894 = VERTEX_POINT ( 'NONE', #120169 ) ;
#119895 = CARTESIAN_POINT ( 'NONE',  ( 184.2083333333333144, -4.445597072760115509, -7.700000000000001954 ) ) ;
#119896 = DIRECTION ( 'NONE',  ( -0.000000000000000000, 1.000000000000000000, -0.000000000000000000 ) ) ;
#119897 = CARTESIAN_POINT ( 'NONE',  ( 3.349999999999941913, 2.500000000000000000, 5.802370205355744659 ) ) ;
#119898 = DIRECTION ( 'NONE',  ( 0.000000000000000000, 1.000000000000000000, 0.000000000000000000 ) ) ;
#119899 = EDGE_CURVE ( 'NONE', #73855, #121027, #78968, .T. ) ;
#119900 = CARTESIAN_POINT ( 'NONE',  ( 4.149999999999939959, 2.500000000000000000, -6.495190528383302464 ) ) ;
#119901 = EDGE_LOOP ( 'NONE', ( #129181, #30749 ) ) ;
#119902 = EDGE_CURVE ( 'NONE', #56812, #70717, #10256, .T. ) ;
#119903 = CARTESIAN_POINT ( 'NONE',  ( 43.06183256894050260, 3.066944586325434319, -4.904925618674059962 ) ) ;
#119904 = CARTESIAN_POINT ( 'NONE',  ( 7.099999999999928590, 12.50000000000000000, 3.637306695894644726 ) ) ;
#119905 = EDGE_CURVE ( 'NONE', #69440, #70666, #104252, .T. ) ;
#119906 = CARTESIAN_POINT ( 'NONE',  ( -8.350000000000008527, 2.500000000000000000, 7.088010851410848190 ) ) ;
#119907 = AXIS2_PLACEMENT_3D ( 'NONE', #51189, #1418, #19108 ) ;
#119908 = ORIENTED_EDGE ( 'NONE', *, *, #57458, .T. ) ;
#119909 = EDGE_CURVE ( 'NONE', #32951, #92601, #368, .T. ) ;
#119910 = ADVANCED_FACE ( 'NONE', ( #30522 ), #100053, .T. ) ;
#119911 = ORIENTED_EDGE ( 'NONE', *, *, #73303, .F. ) ;
#119912 = LINE ( 'NONE', #51827, #50179 ) ;
#119913 = DIRECTION ( 'NONE',  ( 0.000000000000000000, 0.000000000000000000, 1.000000000000000000 ) ) ;
#119914 = EDGE_CURVE ( 'NONE', #108686, #16687, #75007, .T. ) ;
#119915 = CARTESIAN_POINT ( 'NONE',  ( 12.69999999999990337, 2.500000000000000000, -4.576537180435978236 ) ) ;
#119916 = CONICAL_SURFACE ( 'NONE', #23781, 0.1000000000000002554, 0.003490658503988666988 ) ;
#119917 = VERTEX_POINT ( 'NONE', #129370 ) ;
#119918 = AXIS2_PLACEMENT_3D ( 'NONE', #66953, #106882, #107549 ) ;
#119919 = VECTOR ( 'NONE', #55989, 1000.000000000000000 ) ;
#119920 = CARTESIAN_POINT ( 'NONE',  ( 5.399999999999936406, 12.50000000000000000, -3.637306695894650055 ) ) ;
#119921 = EDGE_CURVE ( 'NONE', #57691, #13400, #59988, .T. ) ;
#119922 = CARTESIAN_POINT ( 'NONE',  ( 12.69999999999989804, 2.500000000000000000, 0.3464101615137735735 ) ) ;
#119923 = ORIENTED_EDGE ( 'NONE', *, *, #26637, .F. ) ;
#119924 = CARTESIAN_POINT ( 'NONE',  ( -10.40000000000000213, 2.500000000000000000, 4.330127018922196314 ) ) ;
#119925 = AXIS2_PLACEMENT_3D ( 'NONE', #39146, #99976, #29946 ) ;
#119926 = ORIENTED_EDGE ( 'NONE', *, *, #44132, .F. ) ;
#119927 = CIRCLE ( 'NONE', #63501, 0.06509327318403745899 ) ;
#119928 = ADVANCED_FACE ( 'NONE', ( #10214 ), #40330, .T. ) ;
#119929 = CARTESIAN_POINT ( 'NONE',  ( 6.449999999999930012, 2.500000000000000000, 6.841600689897072485 ) ) ;
#119930 = AXIS2_PLACEMENT_3D ( 'NONE', #90016, #70398, #21288 ) ;
#119931 = AXIS2_PLACEMENT_3D ( 'NONE', #14736, #75605, #44889 ) ;
#119932 = EDGE_LOOP ( 'NONE', ( #69297, #68811, #10203, #32103 ) ) ;
#119933 = DIRECTION ( 'NONE',  ( 0.000000000000000000, 1.000000000000000000, 0.000000000000000000 ) ) ;
#119934 = DIRECTION ( 'NONE',  ( 0.000000000000000000, 0.000000000000000000, 1.000000000000000000 ) ) ;
#119935 = ORIENTED_EDGE ( 'NONE', *, *, #23366, .F. ) ;
#119936 = ORIENTED_EDGE ( 'NONE', *, *, #7245, .T. ) ;
#119937 = AXIS2_PLACEMENT_3D ( 'NONE', #125438, #35773, #47530 ) ;
#119938 = DIRECTION ( 'NONE',  ( -0.000000000000000000, -1.000000000000000000, -0.000000000000000000 ) ) ;
#119939 = DIRECTION ( 'NONE',  ( 0.000000000000000000, 0.000000000000000000, -1.000000000000000000 ) ) ;
#119940 = EDGE_LOOP ( 'NONE', ( #106155, #66488 ) ) ;
#119941 = DIRECTION ( 'NONE',  ( -0.000000000000000000, -1.000000000000000000, -0.000000000000000000 ) ) ;
#119942 = CARTESIAN_POINT ( 'NONE',  ( 187.1510416670080588, 4.367472073101518859, -7.564683531249999149 ) ) ;
#119943 = AXIS2_PLACEMENT_3D ( 'NONE', #36860, #46037, #126525 ) ;
#119944 = DIRECTION ( 'NONE',  ( 0.000000000000000000, 0.000000000000000000, 1.000000000000000000 ) ) ;
#119945 = AXIS2_PLACEMENT_3D ( 'NONE', #129355, #86816, #109019 ) ;
#119946 = CARTESIAN_POINT ( 'NONE',  ( 103.0665022457567943, 8.661908772191825534, -0.8295545705914831869 ) ) ;
#119947 = DIRECTION ( 'NONE',  ( -0.000000000000000000, 1.000000000000000000, -0.000000000000000000 ) ) ;
#119948 = DIRECTION ( 'NONE',  ( 0.000000000000000000, 0.000000000000000000, 1.000000000000000000 ) ) ;
#119949 = AXIS2_PLACEMENT_3D ( 'NONE', #125888, #36252, #76171 ) ;
#119950 = CARTESIAN_POINT ( 'NONE',  ( 1.649999999999950617, 2.500000000000000000, -2.265063509461101798 ) ) ;
#119951 = CIRCLE ( 'NONE', #2882, 0.09999999999999982514 ) ;
#119952 = EDGE_LOOP ( 'NONE', ( #62112, #33080 ) ) ;
#119953 = VERTEX_POINT ( 'NONE', #109711 ) ;
#119954 = ORIENTED_EDGE ( 'NONE', *, *, #42787, .F. ) ;
#119955 = CARTESIAN_POINT ( 'NONE',  ( -14.34999999999998543, 12.50000000000000000, -2.511473670974875727 ) ) ;
#119956 = CARTESIAN_POINT ( 'NONE',  ( -0.6500000000000394351, 12.50000000000000000, 2.511473670974873507 ) ) ;
#119957 = DIRECTION ( 'NONE',  ( 0.000000000000000000, 0.000000000000000000, 1.000000000000000000 ) ) ;
#119959 = VERTEX_POINT ( 'NONE', #69775 ) ;
#119958 = EDGE_LOOP ( 'NONE', ( #52649, #78882, #117232, #33504 ) ) ;
#119960 = FACE_BOUND ( 'NONE', #14459, .T. ) ;
#119961 = EDGE_LOOP ( 'NONE', ( #34722, #33124 ) ) ;
#119962 = CARTESIAN_POINT ( 'NONE',  ( -0.4000000000000392131, 2.500000000000000000, -5.022947341949754119 ) ) ;
#119963 = CARTESIAN_POINT ( 'NONE',  ( 14.99999999999989164, 2.500000000000000000, 0.5928203230275495006 ) ) ;
#119964 = LINE ( 'NONE', #30316, #36737 ) ;
#119965 = EDGE_CURVE ( 'NONE', #126837, #73054, #20044, .T. ) ;
#119966 = CARTESIAN_POINT ( 'NONE',  ( -12.89999999999999325, 2.500000000000000000, -3.737306695894647035 ) ) ;
#119967 = DIRECTION ( 'NONE',  ( -0.000000000000000000, 1.000000000000000000, -0.000000000000000000 ) ) ;
#119968 = DIRECTION ( 'NONE',  ( -0.000000000000000000, -1.000000000000000000, -0.000000000000000000 ) ) ;
#119969 = CARTESIAN_POINT ( 'NONE',  ( -7.499999999999976907, 2.500000000000000000, 4.430127018922196847 ) ) ;
#119970 = CIRCLE ( 'NONE', #2894, 0.1000000000000000472 ) ;
#119971 = DIRECTION ( 'NONE',  ( 0.000000000000000000, 1.000000000000000000, 0.000000000000000000 ) ) ;
#119972 = CARTESIAN_POINT ( 'NONE',  ( 14.39999999999989555, 2.500000000000000000, -0.3464101615137782364 ) ) ;
#119973 = EDGE_CURVE ( 'NONE', #97481, #126422, #70796, .T. ) ;
#119974 = AXIS2_PLACEMENT_3D ( 'NONE', #50062, #100427, #10724 ) ;
#119976 = EDGE_LOOP ( 'NONE', ( #31471, #28581, #88362, #95700 ) ) ;
#119975 = CIRCLE ( 'NONE', #86511, 0.09999999999999982514 ) ;
#119977 = ORIENTED_EDGE ( 'NONE', *, *, #111957, .T. ) ;
#119978 = ORIENTED_EDGE ( 'NONE', *, *, #28497, .T. ) ;
#119979 = ORIENTED_EDGE ( 'NONE', *, *, #77983, .F. ) ;
#119981 = VECTOR ( 'NONE', #42906, 1000.000000000000000 ) ;
#119980 = LINE ( 'NONE', #100345, #22814 ) ;
#119982 = AXIS2_PLACEMENT_3D ( 'NONE', #1372, #61611, #31493 ) ;
#119983 = CARTESIAN_POINT ( 'NONE',  ( 9.349999999999916156, 2.500000000000000000, 6.841600689897072485 ) ) ;
#119985 = EDGE_LOOP ( 'NONE', ( #124117, #97128, #63742, #54670 ) ) ;
#119984 = ORIENTED_EDGE ( 'NONE', *, *, #101281, .F. ) ;
#119986 = ORIENTED_EDGE ( 'NONE', *, *, #48427, .F. ) ;
#119987 = CARTESIAN_POINT ( 'NONE',  ( 7.699999999999925571, 12.50000000000000000, 3.983716857408420076 ) ) ;
#119988 = VECTOR ( 'NONE', #84310, 1000.000000000000000 ) ;
#119989 = CIRCLE ( 'NONE', #15406, 0.06509327318403741736 ) ;
#119990 = CONICAL_SURFACE ( 'NONE', #36474, 0.1000000000000002554, 0.003490658503988666988 ) ;
#119991 = FACE_OUTER_BOUND ( 'NONE', #30850, .T. ) ;
#119992 = CARTESIAN_POINT ( 'NONE',  ( 9.149999999999916866, 2.500000000000000000, -2.957883832488653830 ) ) ;
#119993 = DIRECTION ( 'NONE',  ( 0.000000000000000000, 1.000000000000000000, 0.000000000000000000 ) ) ;
#119994 = FACE_OUTER_BOUND ( 'NONE', #55064, .T. ) ;
#119995 = DIRECTION ( 'NONE',  ( 0.000000000000000000, 0.000000000000000000, -1.000000000000000000 ) ) ;
#119996 = CIRCLE ( 'NONE', #9173, 0.1000000000000002554 ) ;
#119997 = DIRECTION ( 'NONE',  ( -4.274815082592931898E-19, -0.9999939076577903929, -0.003490651415223739937 ) ) ;
#119998 = ORIENTED_EDGE ( 'NONE', *, *, #106428, .F. ) ;
#119999 = CARTESIAN_POINT ( 'NONE',  ( 5.649999999999934630, 2.500000000000000000, 6.148780366869520897 ) ) ;
#120000 = VERTEX_POINT ( 'NONE', #48201 ) ;
#120001 = VERTEX_POINT ( 'NONE', #69122 ) ;
#120002 = ORIENTED_EDGE ( 'NONE', *, *, #18673, .F. ) ;
#120003 = CIRCLE ( 'NONE', #17574, 0.09999999999999982514 ) ;
#120004 = DIRECTION ( 'NONE',  ( 0.000000000000000000, 0.000000000000000000, -1.000000000000000000 ) ) ;
#120005 = VERTEX_POINT ( 'NONE', #58035 ) ;
#120006 = ORIENTED_EDGE ( 'NONE', *, *, #36483, .F. ) ;
#120007 = CIRCLE ( 'NONE', #17579, 0.1000000000000002554 ) ;
#120008 = CARTESIAN_POINT ( 'NONE',  ( 115.5000000000000000, -2.000000000000000000, 2.000000000000003553 ) ) ;
#120009 = EDGE_CURVE ( 'NONE', #74917, #122022, #91727, .T. ) ;
#120010 = DIRECTION ( 'NONE',  ( 0.000000000000000000, 1.000000000000000000, 0.000000000000000000 ) ) ;
#120011 = DIRECTION ( 'NONE',  ( 0.000000000000000000, 0.000000000000000000, -1.000000000000000000 ) ) ;
#120012 = CARTESIAN_POINT ( 'NONE',  ( 3.349999999999943689, 2.500000000000000000, 2.165063509461097713 ) ) ;
#120013 = DIRECTION ( 'NONE',  ( 0.000000000000000000, -0.000000000000000000, 1.000000000000000000 ) ) ;
#120014 = EDGE_LOOP ( 'NONE', ( #64340, #16672 ) ) ;
#120015 = CARTESIAN_POINT ( 'NONE',  ( 9.799999999999913669, 2.500000000000000000, -3.883716857408426648 ) ) ;
#120016 = AXIS2_PLACEMENT_3D ( 'NONE', #9674, #69889, #39801 ) ;
#120017 = ADVANCED_FACE ( 'NONE', ( #29224 ), #20638, .T. ) ;
#120018 = AXIS2_PLACEMENT_3D ( 'NONE', #3364, #94306, #14451 ) ;
#120019 = ORIENTED_EDGE ( 'NONE', *, *, #122019, .T. ) ;
#120020 = CARTESIAN_POINT ( 'NONE',  ( 16.55712542097768392, -0.2763552092527354342, 6.093697598458595266 ) ) ;
#120021 = EDGE_LOOP ( 'NONE', ( #118084, #25390, #111732, #7247 ) ) ;
#120022 = CARTESIAN_POINT ( 'NONE',  ( 110.2387336715401318, 7.457814704407476292, 4.482516261046311179 ) ) ;
#120023 = CARTESIAN_POINT ( 'NONE',  ( -9.600000000000008527, 12.50000000000000000, -3.637306695894645614 ) ) ;
#120024 = ORIENTED_EDGE ( 'NONE', *, *, #40794, .F. ) ;
#120026 = EDGE_CURVE ( 'NONE', #11005, #3528, #37364, .T. ) ;
#120025 = FACE_OUTER_BOUND ( 'NONE', #114767, .T. ) ;
#120028 = AXIS2_PLACEMENT_3D ( 'NONE', #8199, #81471, #31721 ) ;
#120027 = DIRECTION ( 'NONE',  ( 0.000000000000000000, -0.000000000000000000, 1.000000000000000000 ) ) ;
#120029 = EDGE_CURVE ( 'NONE', #61538, #48101, #24830, .T. ) ;
#120030 = ORIENTED_EDGE ( 'NONE', *, *, #67693, .T. ) ;
#120031 = CONICAL_SURFACE ( 'NONE', #15543, 0.1000000000000002554, 0.003490658503988666988 ) ;
#120032 = ADVANCED_FACE ( 'NONE', ( #108404 ), #110509, .T. ) ;
#120033 = LINE ( 'NONE', #63041, #34225 ) ;
#120034 = EDGE_LOOP ( 'NONE', ( #13434, #43955, #72817, #7014 ) ) ;
#120035 = ORIENTED_EDGE ( 'NONE', *, *, #82880, .T. ) ;
#120036 = DIRECTION ( 'NONE',  ( 0.000000000000000000, 0.000000000000000000, 1.000000000000000000 ) ) ;
#120037 = CARTESIAN_POINT ( 'NONE',  ( -0.8500000000000386136, 2.500000000000000000, 7.188010851410848723 ) ) ;
#120038 = EDGE_CURVE ( 'NONE', #30034, #12327, #54074, .T. ) ;
#120039 = LINE ( 'NONE', #118738, #125335 ) ;
#120040 = DIRECTION ( 'NONE',  ( 0.000000000000000000, 1.000000000000000000, 0.000000000000000000 ) ) ;
#120041 = CARTESIAN_POINT ( 'NONE',  ( -10.65000000000000213, 12.50000000000000000, 6.083687093685482772 ) ) ;
#120042 = EDGE_LOOP ( 'NONE', ( #111484, #65469 ) ) ;
#120043 = CIRCLE ( 'NONE', #32422, 0.06509327318403745899 ) ;
#120044 = AXIS2_PLACEMENT_3D ( 'NONE', #1653, #11483, #119269 ) ;
#120045 = DIRECTION ( 'NONE',  ( -0.000000000000000000, -1.000000000000000000, -0.000000000000000000 ) ) ;
#120046 = CONICAL_SURFACE ( 'NONE', #101255, 0.1000000000000000472, 0.003490658503988666988 ) ;
#120047 = VERTEX_POINT ( 'NONE', #109033 ) ;
#120048 = CIRCLE ( 'NONE', #17624, 0.09999999999999999167 ) ;
#120049 = CARTESIAN_POINT ( 'NONE',  ( 7.699999999999925571, 2.500000000000000000, 3.983716857408420076 ) ) ;
#120050 = CARTESIAN_POINT ( 'NONE',  ( 4.149999999999941735, 12.50000000000000000, -1.472243186433550122 ) ) ;
#120051 = CARTESIAN_POINT ( 'NONE',  ( 186.7968750003414300, 8.734944146203032389, 5.348610694689227483E-16 ) ) ;
#120052 = DIRECTION ( 'NONE',  ( 0.000000000000000000, 0.000000000000000000, 1.000000000000000000 ) ) ;
#120053 = CARTESIAN_POINT ( 'NONE',  ( 1.649999999999951061, 12.50000000000000000, -6.495190528383302464 ) ) ;
#120054 = FACE_OUTER_BOUND ( 'NONE', #42116, .T. ) ;
#120055 = CARTESIAN_POINT ( 'NONE',  ( 11.84999999999990727, 12.50000000000000000, 6.213873640053558134 ) ) ;
#120056 = ORIENTED_EDGE ( 'NONE', *, *, #30876, .T. ) ;
#120057 = DIRECTION ( 'NONE',  ( 0.000000000000000000, 0.000000000000000000, 1.000000000000000000 ) ) ;
#120059 = FACE_OUTER_BOUND ( 'NONE', #40712, .T. ) ;
#120058 = CIRCLE ( 'NONE', #63630, 0.06509327318403745899 ) ;
#120060 = DIRECTION ( 'NONE',  ( 0.000000000000000000, 1.000000000000000000, 0.000000000000000000 ) ) ;
#120061 = AXIS2_PLACEMENT_3D ( 'NONE', #38750, #30692, #6635 ) ;
#120062 = CIRCLE ( 'NONE', #120152, 0.06509327318403745899 ) ;
#120063 = CONICAL_SURFACE ( 'NONE', #11387, 0.1000000000000002554, 0.003490658503988666988 ) ;
#120064 = VERTEX_POINT ( 'NONE', #59340 ) ;
#120065 = ADVANCED_FACE ( 'NONE', ( #104833 ), #81269, .T. ) ;
#120066 = CARTESIAN_POINT ( 'NONE',  ( 3.349999999999945466, 12.50000000000000000, -7.188010851410854052 ) ) ;
#120067 = AXIS2_PLACEMENT_3D ( 'NONE', #78050, #125850, #97050 ) ;
#120068 = AXIS2_PLACEMENT_3D ( 'NONE', #9075, #58198, #50953 ) ;
#120069 = VERTEX_POINT ( 'NONE', #96305 ) ;
#120070 = CIRCLE ( 'NONE', #40675, 0.1000000000000002554 ) ;
#120071 = ORIENTED_EDGE ( 'NONE', *, *, #112691, .F. ) ;
#120072 = CARTESIAN_POINT ( 'NONE',  ( 2.899999999999943956, 2.500000000000000000, 4.330127018922196314 ) ) ;
#120073 = ADVANCED_FACE ( 'NONE', ( #15813 ), #95040, .T. ) ;
#120074 = ORIENTED_EDGE ( 'NONE', *, *, #80307, .T. ) ;
#120075 = CARTESIAN_POINT ( 'NONE',  ( 12.89999999999989910, 2.500000000000000000, -0.6928203230275542523 ) ) ;
#120077 = ADVANCED_FACE ( 'NONE', ( #15153 ), #104343, .T. ) ;
#120076 = DIRECTION ( 'NONE',  ( -0.000000000000000000, -1.000000000000000000, -0.000000000000000000 ) ) ;
#120078 = EDGE_CURVE ( 'NONE', #73868, #49718, #45303, .T. ) ;
#120080 = VERTEX_POINT ( 'NONE', #16447 ) ;
#120079 = VECTOR ( 'NONE', #45690, 1000.000000000000000 ) ;
#120081 = CIRCLE ( 'NONE', #40680, 0.1000000000000000472 ) ;
#120082 = AXIS2_PLACEMENT_3D ( 'NONE', #64085, #15613, #33985 ) ;
#120083 = DIRECTION ( 'NONE',  ( -0.000000000000000000, -1.000000000000000000, -0.000000000000000000 ) ) ;
#120084 = EDGE_CURVE ( 'NONE', #34772, #74521, #6126, .T. ) ;
#120085 = CARTESIAN_POINT ( 'NONE',  ( 3.749999999999944045, 12.50000000000000000, -2.792790559304616504 ) ) ;
#120086 = AXIS2_PLACEMENT_3D ( 'NONE', #43104, #63361, #83016 ) ;
#120087 = DIRECTION ( 'NONE',  ( 0.000000000000000000, 0.000000000000000000, -1.000000000000000000 ) ) ;
#120088 = ORIENTED_EDGE ( 'NONE', *, *, #53147, .F. ) ;
#120089 = ADVANCED_FACE ( 'NONE', ( #75376 ), #41672, .T. ) ;
#120090 = ADVANCED_FACE ( 'NONE', ( #66845 ), #29142, .T. ) ;
#120091 = ORIENTED_EDGE ( 'NONE', *, *, #27775, .F. ) ;
#120092 = VERTEX_POINT ( 'NONE', #26301 ) ;
#120093 = DIRECTION ( 'NONE',  ( 0.000000000000000000, 1.000000000000000000, 0.000000000000000000 ) ) ;
#120094 = FACE_OUTER_BOUND ( 'NONE', #88452, .T. ) ;
#120095 = DIRECTION ( 'NONE',  ( 0.000000000000000000, 1.000000000000000000, 0.000000000000000000 ) ) ;
#120096 = FACE_BOUND ( 'NONE', #32084, .T. ) ;
#120097 = EDGE_LOOP ( 'NONE', ( #50343, #74078 ) ) ;
#120098 = DIRECTION ( 'NONE',  ( 0.000000000000000000, 0.000000000000000000, 1.000000000000000000 ) ) ;
#120099 = CARTESIAN_POINT ( 'NONE',  ( 8.749999999999953815, 2.500000000000000000, 6.395190528383296602 ) ) ;
#120100 = AXIS2_PLACEMENT_3D ( 'NONE', #106190, #25045, #64954 ) ;
#120101 = VERTEX_POINT ( 'NONE', #17745 ) ;
#120102 = CARTESIAN_POINT ( 'NONE',  ( -6.650000000000014566, 2.500000000000000000, 6.395190528383296602 ) ) ;
#120103 = DIRECTION ( 'NONE',  ( -0.000000000000000000, 1.000000000000000000, -0.000000000000000000 ) ) ;
#120104 = CARTESIAN_POINT ( 'NONE',  ( 0.3999999999999568345, 2.500000000000000000, -3.537306695894649966 ) ) ;
#120105 = CARTESIAN_POINT ( 'NONE',  ( 14.54999999999989235, 12.50000000000000000, -2.165063509461101710 ) ) ;
#120106 = DIRECTION ( 'NONE',  ( -0.000000000000000000, 1.000000000000000000, -0.000000000000000000 ) ) ;
#120107 = CARTESIAN_POINT ( 'NONE',  ( 2.699999999999947331, 2.500000000000000000, -0.3464101615137783474 ) ) ;
#120108 = EDGE_CURVE ( 'NONE', #111656, #115693, #121064, .T. ) ;
#120109 = DIRECTION ( 'NONE',  ( -0.000000000000000000, -1.000000000000000000, -0.000000000000000000 ) ) ;
#120110 = ORIENTED_EDGE ( 'NONE', *, *, #86940, .F. ) ;
#120111 = ORIENTED_EDGE ( 'NONE', *, *, #113779, .F. ) ;
#120112 = ORIENTED_EDGE ( 'NONE', *, *, #50319, .T. ) ;
#120113 = VERTEX_POINT ( 'NONE', #85207 ) ;
#120114 = CARTESIAN_POINT ( 'NONE',  ( 5.449999999999936229, 2.500000000000000000, 6.395190528383296602 ) ) ;
#120115 = DIRECTION ( 'NONE',  ( 0.000000000000000000, -0.000000000000000000, 1.000000000000000000 ) ) ;
#120116 = EDGE_CURVE ( 'NONE', #35149, #9410, #110596, .T. ) ;
#120117 = EDGE_LOOP ( 'NONE', ( #93044, #116347, #35353, #14779 ) ) ;
#120118 = FACE_BOUND ( 'NONE', #109210, .T. ) ;
#120119 = DIRECTION ( 'NONE',  ( 0.000000000000000000, 1.000000000000000000, 0.000000000000000000 ) ) ;
#120120 = CIRCLE ( 'NONE', #97129, 0.06509327318403745899 ) ;
#120121 = LINE ( 'NONE', #51398, #120267 ) ;
#120122 = CYLINDRICAL_SURFACE ( 'NONE', #74254, 1.388921157871086942 ) ;
#120123 = AXIS2_PLACEMENT_3D ( 'NONE', #24315, #5304, #64237 ) ;
#120124 = DIRECTION ( 'NONE',  ( -0.000000000000000000, -1.000000000000000000, -0.000000000000000000 ) ) ;
#120125 = CARTESIAN_POINT ( 'NONE',  ( -1.850000000000033396, 12.50000000000000000, -1.753560074763288457 ) ) ;
#120126 = DIRECTION ( 'NONE',  ( 0.000000000000000000, -0.9999939076577903929, 0.003490651415223739937 ) ) ;
#120127 = DIRECTION ( 'NONE',  ( 0.000000000000000000, 1.000000000000000000, 0.000000000000000000 ) ) ;
#120128 = ORIENTED_EDGE ( 'NONE', *, *, #120029, .T. ) ;
#120129 = EDGE_LOOP ( 'NONE', ( #52329, #56011, #82, #54249 ) ) ;
#120130 = ADVANCED_FACE ( 'NONE', ( #25633 ), #27076, .T. ) ;
#120131 = AXIS2_PLACEMENT_3D ( 'NONE', #17686, #69362, #47812 ) ;
#120132 = ORIENTED_EDGE ( 'NONE', *, *, #56090, .F. ) ;
#120133 = ORIENTED_EDGE ( 'NONE', *, *, #45750, .T. ) ;
#120134 = AXIS2_PLACEMENT_3D ( 'NONE', #59287, #49466, #67787 ) ;
#120135 = VERTEX_POINT ( 'NONE', #47231 ) ;
#120136 = ORIENTED_EDGE ( 'NONE', *, *, #13938, .T. ) ;
#120137 = DIRECTION ( 'NONE',  ( 0.000000000000000000, 0.000000000000000000, 1.000000000000000000 ) ) ;
#120139 = CIRCLE ( 'NONE', #118068, 0.09999999999999982514 ) ;
#120138 = CARTESIAN_POINT ( 'NONE',  ( -7.300000000000018474, 12.50000000000000000, -3.983716857408426293 ) ) ;
#120140 = ORIENTED_EDGE ( 'NONE', *, *, #109392, .F. ) ;
#120141 = CARTESIAN_POINT ( 'NONE',  ( 4.999999999999935163, 12.50000000000000000, 3.637306695894644726 ) ) ;
#120142 = CARTESIAN_POINT ( 'NONE',  ( -3.550000000000027800, 2.500000000000000000, 6.248780366869520542 ) ) ;
#120143 = CARTESIAN_POINT ( 'NONE',  ( 184.5260416670080588, -6.551208109652273848, -3.782341765625003571 ) ) ;
#120144 = CARTESIAN_POINT ( 'NONE',  ( 6.449999999999931788, 12.50000000000000000, 6.148780366869520009 ) ) ;
#120145 = CARTESIAN_POINT ( 'NONE',  ( -9.600000000000006750, 2.500000000000000000, -0.6928203230275542523 ) ) ;
#120146 = EDGE_LOOP ( 'NONE', ( #75050, #51262 ) ) ;
#120147 = DIRECTION ( 'NONE',  ( 0.000000000000000000, 0.000000000000000000, -1.000000000000000000 ) ) ;
#120148 = ORIENTED_EDGE ( 'NONE', *, *, #96914, .T. ) ;
#120150 = EDGE_LOOP ( 'NONE', ( #99424, #58997 ) ) ;
#120149 = VECTOR ( 'NONE', #95552, 1000.000000000000000 ) ;
#120151 = CARTESIAN_POINT ( 'NONE',  ( -7.100000000000017408, 2.500000000000000000, -0.7928203230275543412 ) ) ;
#120152 = AXIS2_PLACEMENT_3D ( 'NONE', #81538, #71713, #103758 ) ;
#120153 = PLANE ( 'NONE',  #88644 ) ;
#120154 = CIRCLE ( 'NONE', #59549, 0.1000000000000000472 ) ;
#120155 = DIRECTION ( 'NONE',  ( -0.000000000000000000, -1.000000000000000000, -0.000000000000000000 ) ) ;
#120156 = ORIENTED_EDGE ( 'NONE', *, *, #106338, .F. ) ;
#120157 = VERTEX_POINT ( 'NONE', #105505 ) ;
#120158 = CARTESIAN_POINT ( 'NONE',  ( -5.450000000000019718, 12.50000000000000000, 6.495190528383297135 ) ) ;
#120159 = AXIS2_PLACEMENT_3D ( 'NONE', #88096, #110194, #60471 ) ;
#120160 = AXIS2_PLACEMENT_3D ( 'NONE', #29354, #117047, #67286 ) ;
#120161 = CIRCLE ( 'NONE', #95122, 0.06509327318403745899 ) ;
#120162 = DIRECTION ( 'NONE',  ( -0.000000000000000000, -1.000000000000000000, -0.000000000000000000 ) ) ;
#120163 = CARTESIAN_POINT ( 'NONE',  ( -12.09999999999999609, 2.500000000000000000, -4.922947341949750921 ) ) ;
#120164 = CARTESIAN_POINT ( 'NONE',  ( 12.89999999999989733, 2.500000000000000000, 0.09999999999999761857 ) ) ;
#120165 = ORIENTED_EDGE ( 'NONE', *, *, #99194, .T. ) ;
#120166 = CIRCLE ( 'NONE', #19917, 0.09999999999999982514 ) ;
#120167 = CARTESIAN_POINT ( 'NONE',  ( -5.650000000000023448, 2.500000000000000000, -6.841600689897078702 ) ) ;
#120168 = ORIENTED_EDGE ( 'NONE', *, *, #85868, .T. ) ;
#120169 = CARTESIAN_POINT ( 'NONE',  ( 176.5000000000000000, 6.123233995736766282E-16, 5.000000000000000000 ) ) ;
#120170 = AXIS2_PLACEMENT_3D ( 'NONE', #106496, #38422, #67178 ) ;
#120172 = EDGE_CURVE ( 'NONE', #54857, #49033, #55746, .T. ) ;
#120171 = CIRCLE ( 'NONE', #84660, 0.09999999999999982514 ) ;
#120173 = ORIENTED_EDGE ( 'NONE', *, *, #99237, .F. ) ;
#120174 = CARTESIAN_POINT ( 'NONE',  ( -11.69999999999999929, 2.500000000000000000, 1.734723475976807094E-15 ) ) ;
#120175 = DIRECTION ( 'NONE',  ( -0.000000000000000000, 1.000000000000000000, -0.000000000000000000 ) ) ;
#120176 = DIRECTION ( 'NONE',  ( 0.000000000000000000, 0.000000000000000000, 1.000000000000000000 ) ) ;
#120177 = AXIS2_PLACEMENT_3D ( 'NONE', #78349, #71092, #51466 ) ;
#120178 = ADVANCED_FACE ( 'NONE', ( #45945 ), #24923, .T. ) ;
#120179 = DIRECTION ( 'NONE',  ( 0.000000000000000000, 1.000000000000000000, 0.000000000000000000 ) ) ;
#120180 = EDGE_CURVE ( 'NONE', #98287, #54837, #50077, .T. ) ;
#120181 = EDGE_LOOP ( 'NONE', ( #55699, #89492, #58283, #19914 ) ) ;
#120182 = DIRECTION ( 'NONE',  ( 0.000000000000000000, 0.000000000000000000, 1.000000000000000000 ) ) ;
#120183 = ADVANCED_FACE ( 'NONE', ( #27557 ), #54177, .T. ) ;
#120184 = DIRECTION ( 'NONE',  ( 0.000000000000000000, 0.000000000000000000, 1.000000000000000000 ) ) ;
#120185 = ORIENTED_EDGE ( 'NONE', *, *, #87978, .T. ) ;
#120186 = EDGE_CURVE ( 'NONE', #91471, #124289, #45855, .T. ) ;
#120187 = ORIENTED_EDGE ( 'NONE', *, *, #52665, .F. ) ;
#120188 = EDGE_CURVE ( 'NONE', #121037, #16096, #39618, .T. ) ;
#120189 = ORIENTED_EDGE ( 'NONE', *, *, #80516, .F. ) ;
#120190 = DIRECTION ( 'NONE',  ( 0.000000000000000000, -0.000000000000000000, 1.000000000000000000 ) ) ;
#120191 = DIRECTION ( 'NONE',  ( 0.000000000000000000, 0.000000000000000000, -1.000000000000000000 ) ) ;
#120192 = CARTESIAN_POINT ( 'NONE',  ( -4.600000000000025402, 2.500000000000000000, -2.385244779468109755E-15 ) ) ;
#120193 = ADVANCED_FACE ( 'NONE', ( #108712 ), #119007, .T. ) ;
#120194 = DIRECTION ( 'NONE',  ( 0.000000000000000000, 1.000000000000000000, 0.000000000000000000 ) ) ;
#120195 = CIRCLE ( 'NONE', #7297, 0.09999999999999999167 ) ;
#120196 = CARTESIAN_POINT ( 'NONE',  ( -1.450000000000035483, 2.500000000000000000, 1.818653347947321475 ) ) ;
#120197 = DIRECTION ( 'NONE',  ( -0.000000000000000000, -1.000000000000000000, -0.000000000000000000 ) ) ;
#120198 = DIRECTION ( 'NONE',  ( 0.000000000000000000, -0.9999939076577903929, 0.003490651415223739937 ) ) ;
#120199 = DIRECTION ( 'NONE',  ( -0.000000000000000000, 1.000000000000000000, -0.000000000000000000 ) ) ;
#120200 = FACE_OUTER_BOUND ( 'NONE', #2585, .T. ) ;
#120201 = EDGE_CURVE ( 'NONE', #125681, #54589, #100193, .T. ) ;
#120202 = AXIS2_PLACEMENT_3D ( 'NONE', #112239, #61203, #52664 ) ;
#120203 = AXIS2_PLACEMENT_3D ( 'NONE', #67246, #114444, #24790 ) ;
#120204 = VERTEX_POINT ( 'NONE', #88416 ) ;
#120205 = DIRECTION ( 'NONE',  ( -0.000000000000000000, -1.000000000000000000, -0.000000000000000000 ) ) ;
#120206 = DIRECTION ( 'NONE',  ( -0.000000000000000000, 1.000000000000000000, -0.000000000000000000 ) ) ;
#120207 = CARTESIAN_POINT ( 'NONE',  ( -2.100000000000033840, 2.500000000000000000, 3.737306695894644371 ) ) ;
#120208 = CARTESIAN_POINT ( 'NONE',  ( 3.349999999999941913, 12.50000000000000000, 6.560283801567334372 ) ) ;
#120209 = CARTESIAN_POINT ( 'NONE',  ( 2.099999999999948574, 2.500000000000000000, 3.737306695894644371 ) ) ;
#120210 = EDGE_LOOP ( 'NONE', ( #21269, #80527 ) ) ;
#120211 = CARTESIAN_POINT ( 'NONE',  ( -1.450000000000035039, 2.500000000000000000, -6.741600689897077281 ) ) ;
#120212 = CIRCLE ( 'NONE', #15727, 0.06509327318403745899 ) ;
#120213 = VECTOR ( 'NONE', #67945, 1000.000000000000000 ) ;
#120214 = DIRECTION ( 'NONE',  ( 0.000000000000000000, 1.000000000000000000, 0.000000000000000000 ) ) ;
#120216 = VERTEX_POINT ( 'NONE', #8560 ) ;
#120215 = DIRECTION ( 'NONE',  ( 0.000000000000000000, 0.000000000000000000, -1.000000000000000000 ) ) ;
#120217 = ADVANCED_FACE ( 'NONE', ( #39991 ), #2206, .T. ) ;
#120218 = VERTEX_POINT ( 'NONE', #60900 ) ;
#120219 = DIRECTION ( 'NONE',  ( 0.000000000000000000, 1.000000000000000000, 0.000000000000000000 ) ) ;
#120220 = AXIS2_PLACEMENT_3D ( 'NONE', #123312, #32392, #72297 ) ;
#120221 = VECTOR ( 'NONE', #123341, 1000.000000000000000 ) ;
#120222 = EDGE_LOOP ( 'NONE', ( #10413, #27169 ) ) ;
#120223 = ORIENTED_EDGE ( 'NONE', *, *, #113389, .F. ) ;
#120224 = DIRECTION ( 'NONE',  ( 0.000000000000000000, 1.000000000000000000, 0.000000000000000000 ) ) ;
#120225 = EDGE_CURVE ( 'NONE', #119487, #47194, #118528, .T. ) ;
#120226 = EDGE_CURVE ( 'NONE', #121748, #125596, #9232, .T. ) ;
#120227 = CARTESIAN_POINT ( 'NONE',  ( 18.37149739119586656, 2.540880845002003063, -2.596776292461022706 ) ) ;
#120229 = EDGE_CURVE ( 'NONE', #78481, #114814, #47921, .T. ) ;
#120228 = DIRECTION ( 'NONE',  ( -0.000000000000000000, 1.000000000000000000, -0.000000000000000000 ) ) ;
#120230 = FACE_OUTER_BOUND ( 'NONE', #35471, .T. ) ;
#120231 = ORIENTED_EDGE ( 'NONE', *, *, #121287, .F. ) ;
#120232 = ADVANCED_FACE ( 'NONE', ( #49817 ), #16583, .T. ) ;
#120233 = CARTESIAN_POINT ( 'NONE',  ( 184.7500000000000000, 9.429780353434619030E-16, -7.700000000000000178 ) ) ;
#120234 = EDGE_LOOP ( 'NONE', ( #126819, #16618, #63071, #123408 ) ) ;
#120235 = DIRECTION ( 'NONE',  ( 0.000000000000000000, 1.000000000000000000, 0.000000000000000000 ) ) ;
#120236 = ADVANCED_FACE ( 'NONE', ( #19029 ), #687, .T. ) ;
#120237 = DIRECTION ( 'NONE',  ( 0.000000000000000000, 1.000000000000000000, 0.000000000000000000 ) ) ;
#120238 = ADVANCED_FACE ( 'NONE', ( #89719 ), #89084, .T. ) ;
#120239 = DIRECTION ( 'NONE',  ( 0.000000000000000000, 0.000000000000000000, 1.000000000000000000 ) ) ;
#120240 = ADVANCED_FACE ( 'NONE', ( #47879 ), #29518, .T. ) ;
#120241 = ORIENTED_EDGE ( 'NONE', *, *, #67786, .F. ) ;
#120242 = ADVANCED_FACE ( 'NONE', ( #77961 ), #109356, .T. ) ;
#120243 = EDGE_CURVE ( 'NONE', #105724, #33641, #8182, .T. ) ;
#120244 = AXIS2_PLACEMENT_3D ( 'NONE', #23419, #93462, #92164 ) ;
#120245 = VERTEX_POINT ( 'NONE', #82495 ) ;
#120246 = VERTEX_POINT ( 'NONE', #71352 ) ;
#120247 = CONICAL_SURFACE ( 'NONE', #97249, 0.09999999999999982514, 0.003490658503988666988 ) ;
#120248 = ORIENTED_EDGE ( 'NONE', *, *, #60804, .T. ) ;
#120249 = ORIENTED_EDGE ( 'NONE', *, *, #97425, .F. ) ;
#120250 = CARTESIAN_POINT ( 'NONE',  ( -14.14999999999998614, 12.50000000000000000, 2.165063509461101265 ) ) ;
#120251 = CARTESIAN_POINT ( 'NONE',  ( 10.30524027349397898, 1.500000000000000222, 9.130939513664273477 ) ) ;
#120252 = AXIS2_PLACEMENT_3D ( 'NONE', #60285, #97597, #100186 ) ;
#120253 = DIRECTION ( 'NONE',  ( 0.000000000000000000, 0.000000000000000000, 1.000000000000000000 ) ) ;
#120254 = FACE_BOUND ( 'NONE', #20515, .T. ) ;
#120255 = LINE ( 'NONE', #60695, #124597 ) ;
#120256 = CARTESIAN_POINT ( 'NONE',  ( 186.3229166673494603, -4.445597072760122614, 7.699999999999998401 ) ) ;
#120257 = EDGE_CURVE ( 'NONE', #100851, #26800, #70901, .T. ) ;
#120258 = FACE_OUTER_BOUND ( 'NONE', #8183, .T. ) ;
#120259 = CARTESIAN_POINT ( 'NONE',  ( -7.950000000000012612, 2.500000000000000000, 2.165063509461097713 ) ) ;
#120260 = AXIS2_PLACEMENT_3D ( 'NONE', #62679, #12893, #122882 ) ;
#120261 = AXIS2_PLACEMENT_3D ( 'NONE', #31637, #21828, #82684 ) ;
#120262 = DIRECTION ( 'NONE',  ( -0.000000000000000000, -1.000000000000000000, -0.000000000000000000 ) ) ;
#120263 = AXIS2_PLACEMENT_3D ( 'NONE', #60023, #10868, #90745 ) ;
#120264 = FACE_OUTER_BOUND ( 'NONE', #16459, .T. ) ;
#120265 = LINE ( 'NONE', #10909, #19859 ) ;
#120266 = CIRCLE ( 'NONE', #84753, 0.06509327318403745899 ) ;
#120267 = VECTOR ( 'NONE', #21261, 1000.000000000000000 ) ;
#120268 = CARTESIAN_POINT ( 'NONE',  ( 5.799999999999931433, 2.500000000000000000, 4.430127018922196847 ) ) ;
#120269 = VERTEX_POINT ( 'NONE', #122415 ) ;
#120270 = ORIENTED_EDGE ( 'NONE', *, *, #10123, .T. ) ;
#120271 = ORIENTED_EDGE ( 'NONE', *, *, #57729, .T. ) ;
#120272 = ORIENTED_EDGE ( 'NONE', *, *, #106727, .F. ) ;
#120273 = AXIS2_PLACEMENT_3D ( 'NONE', #17792, #7327, #68181 ) ;
#120274 = DIRECTION ( 'NONE',  ( -4.274815082592931898E-19, -0.9999939076577903929, -0.003490651415223739937 ) ) ;
#120275 = DIRECTION ( 'NONE',  ( 0.000000000000000000, 0.000000000000000000, 1.000000000000000000 ) ) ;
#120276 = FACE_BOUND ( 'NONE', #30708, .T. ) ;
#120277 = CARTESIAN_POINT ( 'NONE',  ( 1.049999999999954969, 2.500000000000000000, -6.841600689897077814 ) ) ;
#120278 = VERTEX_POINT ( 'NONE', #52373 ) ;
#120279 = DIRECTION ( 'NONE',  ( -0.000000000000000000, -1.000000000000000000, -0.000000000000000000 ) ) ;
#120280 = DIRECTION ( 'NONE',  ( 0.000000000000000000, 0.000000000000000000, -1.000000000000000000 ) ) ;
#120281 = FACE_OUTER_BOUND ( 'NONE', #67099, .T. ) ;
#120282 = DIRECTION ( 'NONE',  ( 0.000000000000000000, 0.000000000000000000, 1.000000000000000000 ) ) ;
#120284 = VERTEX_POINT ( 'NONE', #2611 ) ;
#120283 = AXIS2_PLACEMENT_3D ( 'NONE', #126397, #85178, #15122 ) ;
#120285 = LINE ( 'NONE', #30627, #74329 ) ;
#120286 = ADVANCED_FACE ( 'NONE', ( #64122 ), #33356, .T. ) ;
#120287 = ORIENTED_EDGE ( 'NONE', *, *, #87733, .F. ) ;
#120288 = EDGE_LOOP ( 'NONE', ( #115080, #14316 ) ) ;
#120289 = DIRECTION ( 'NONE',  ( 0.000000000000000000, -0.000000000000000000, 1.000000000000000000 ) ) ;
#120290 = CARTESIAN_POINT ( 'NONE',  ( -7.950000000000016165, 2.500000000000000000, -6.595190528383296780 ) ) ;
#120291 = ORIENTED_EDGE ( 'NONE', *, *, #27510, .F. ) ;
#120292 = AXIS2_PLACEMENT_3D ( 'NONE', #25780, #105644, #86634 ) ;
#120293 = VECTOR ( 'NONE', #73085, 1000.000000000000000 ) ;
#120294 = CARTESIAN_POINT ( 'NONE',  ( 184.5000000000000000, -6.267304879582558996, 4.236192450104883100 ) ) ;
#120295 = FACE_OUTER_BOUND ( 'NONE', #106230, .T. ) ;
#120296 = CARTESIAN_POINT ( 'NONE',  ( 2.899999999999946620, 12.50000000000000000, -5.022947341949754119 ) ) ;
#120297 = VERTEX_POINT ( 'NONE', #103414 ) ;
#120298 = ADVANCED_FACE ( 'NONE', ( #32761 ), #92957, .T. ) ;
#120299 = DIRECTION ( 'NONE',  ( 0.000000000000000000, 0.000000000000000000, 1.000000000000000000 ) ) ;
#120300 = ORIENTED_EDGE ( 'NONE', *, *, #7628, .T. ) ;
#120301 = DIRECTION ( 'NONE',  ( 0.000000000000000000, 1.000000000000000000, 0.000000000000000000 ) ) ;
#120302 = VECTOR ( 'NONE', #59723, 1000.000000000000000 ) ;
#120303 = EDGE_LOOP ( 'NONE', ( #75005, #17045, #81465, #32009 ) ) ;
#120305 = CARTESIAN_POINT ( 'NONE',  ( 1.649999999999949729, 2.500000000000000000, 5.802370205355744659 ) ) ;
#120304 = CIRCLE ( 'NONE', #1165, 0.06509327318403745899 ) ;
#120306 = VERTEX_POINT ( 'NONE', #83140 ) ;
#120307 = CARTESIAN_POINT ( 'NONE',  ( 5.849999999999933920, 2.500000000000000000, -2.857883832488653741 ) ) ;
#120308 = CARTESIAN_POINT ( 'NONE',  ( -1.250000000000001110, 2.500000000000000000, -2.265063509461101798 ) ) ;
#120309 = CARTESIAN_POINT ( 'NONE',  ( 11.04999999999991012, 12.50000000000000000, 6.841600689897072485 ) ) ;
#120310 = CARTESIAN_POINT ( 'NONE',  ( -3.150000000000033218, 12.50000000000000000, -6.841600689897078702 ) ) ;
#120311 = DIRECTION ( 'NONE',  ( 0.000000000000000000, 1.000000000000000000, 0.000000000000000000 ) ) ;
#120312 = EDGE_LOOP ( 'NONE', ( #89772, #85784, #26550, #120995 ) ) ;
#120313 = ORIENTED_EDGE ( 'NONE', *, *, #78347, .T. ) ;
#120314 = ORIENTED_EDGE ( 'NONE', *, *, #39420, .T. ) ;
#120315 = DIRECTION ( 'NONE',  ( 0.000000000000000000, 1.000000000000000000, 0.000000000000000000 ) ) ;
#120316 = CIRCLE ( 'NONE', #3328, 0.1000000000000002554 ) ;
#120317 = VECTOR ( 'NONE', #127220, 1000.000000000000000 ) ;
#120318 = DIRECTION ( 'NONE',  ( 0.000000000000000000, 0.000000000000000000, -1.000000000000000000 ) ) ;
#120319 = DIRECTION ( 'NONE',  ( 0.000000000000000000, 0.000000000000000000, 1.000000000000000000 ) ) ;
#120321 = ORIENTED_EDGE ( 'NONE', *, *, #105605, .T. ) ;
#120320 = VERTEX_POINT ( 'NONE', #1332 ) ;
#120322 = ORIENTED_EDGE ( 'NONE', *, *, #33169, .F. ) ;
#120323 = DIRECTION ( 'NONE',  ( 0.000000000000000000, -0.9999939076577903929, 0.003490651415223739937 ) ) ;
#120324 = ORIENTED_EDGE ( 'NONE', *, *, #32557, .T. ) ;
#120325 = DIRECTION ( 'NONE',  ( 0.000000000000000000, 0.000000000000000000, -1.000000000000000000 ) ) ;
#120326 = EDGE_CURVE ( 'NONE', #93646, #1061, #68831, .T. ) ;
#120327 = CARTESIAN_POINT ( 'NONE',  ( -14.14999999999998614, 2.500000000000000000, 2.165063509461101265 ) ) ;
#120328 = CARTESIAN_POINT ( 'NONE',  ( -0.2000000000000408673, 2.500000000000000000, -4.083716857408426826 ) ) ;
#120329 = AXIS2_PLACEMENT_3D ( 'NONE', #44311, #94064, #73764 ) ;
#120330 = DIRECTION ( 'NONE',  ( 0.000000000000000000, 1.000000000000000000, 0.000000000000000000 ) ) ;
#120331 = CARTESIAN_POINT ( 'NONE',  ( 185.5833333333333144, -6.668395609140180369, 3.849999999999994760 ) ) ;
#120332 = CARTESIAN_POINT ( 'NONE',  ( 162.5000000000000000, 0.5000000000000000000, 7.499999999999994671 ) ) ;
#120333 = AXIS2_PLACEMENT_3D ( 'NONE', #11656, #51601, #30028 ) ;
#120334 = CARTESIAN_POINT ( 'NONE',  ( -11.05000000000000071, 2.500000000000000000, -2.411473670974874306 ) ) ;
#120335 = EDGE_CURVE ( 'NONE', #3627, #107815, #66764, .T. ) ;
#120336 = ORIENTED_EDGE ( 'NONE', *, *, #44107, .F. ) ;
#120337 = ORIENTED_EDGE ( 'NONE', *, *, #107806, .T. ) ;
#120338 = LINE ( 'NONE', #20203, #119732 ) ;
#120339 = AXIS2_PLACEMENT_3D ( 'NONE', #43510, #44134, #55252 ) ;
#120340 = AXIS2_PLACEMENT_3D ( 'NONE', #58398, #59699, #57749 ) ;
#120341 = FACE_OUTER_BOUND ( 'NONE', #125484, .T. ) ;
#120342 = EDGE_CURVE ( 'NONE', #66203, #35924, #75100, .T. ) ;
#120343 = ORIENTED_EDGE ( 'NONE', *, *, #67446, .F. ) ;
#120344 = ADVANCED_FACE ( 'NONE', ( #1973 ), #24208, .T. ) ;
#120345 = ORIENTED_EDGE ( 'NONE', *, *, #52462, .F. ) ;
#120346 = EDGE_CURVE ( 'NONE', #39511, #126455, #108544, .T. ) ;
#120347 = CARTESIAN_POINT ( 'NONE',  ( 187.1093750003414016, 9.264065473108010111E-16, -7.564683531250000925 ) ) ;
#120349 = EDGE_CURVE ( 'NONE', #98829, #74234, #41285, .T. ) ;
#120348 = CARTESIAN_POINT ( 'NONE',  ( 1.849999999999949685, 12.50000000000000000, 1.818653347947321475 ) ) ;
#120350 = EDGE_CURVE ( 'NONE', #51798, #81523, #31022, .T. ) ;
#120351 = DIRECTION ( 'NONE',  ( 0.000000000000000000, 0.000000000000000000, 1.000000000000000000 ) ) ;
#120352 = CIRCLE ( 'NONE', #21871, 0.09999999999999982514 ) ;
#120353 = CARTESIAN_POINT ( 'NONE',  ( -6.250000000000019540, 12.50000000000000000, -7.188010851410854052 ) ) ;
#120354 = DIRECTION ( 'NONE',  ( -0.000000000000000000, 1.000000000000000000, -0.000000000000000000 ) ) ;
#120355 = CARTESIAN_POINT ( 'NONE',  ( -2.950000000000029932, 2.500000000000000000, -2.065063509461102065 ) ) ;
#120356 = DIRECTION ( 'NONE',  ( 0.000000000000000000, 1.000000000000000000, 0.000000000000000000 ) ) ;
#120357 = ADVANCED_FACE ( 'NONE', ( #3913 ), #102094, .T. ) ;
#120359 = EDGE_CURVE ( 'NONE', #115626, #122432, #120866, .T. ) ;
#120358 = DIRECTION ( 'NONE',  ( 0.000000000000000000, 0.000000000000000000, 1.000000000000000000 ) ) ;
#120360 = VERTEX_POINT ( 'NONE', #111266 ) ;
#120361 = EDGE_CURVE ( 'NONE', #69008, #24259, #4077, .T. ) ;
#120362 = ORIENTED_EDGE ( 'NONE', *, *, #90949, .T. ) ;
#120363 = CONICAL_SURFACE ( 'NONE', #80651, 0.09999999999999982514, 0.003490658503988666988 ) ;
#120364 = VERTEX_POINT ( 'NONE', #11799 ) ;
#120365 = ORIENTED_EDGE ( 'NONE', *, *, #99399, .T. ) ;
#120366 = EDGE_LOOP ( 'NONE', ( #54288, #79519, #110792, #85524 ) ) ;
#120367 = DIRECTION ( 'NONE',  ( 0.000000000000000000, -0.9999939076577903929, 0.003490651415223739937 ) ) ;
#120368 = DIRECTION ( 'NONE',  ( 0.000000000000000000, 0.000000000000000000, 1.000000000000000000 ) ) ;
#120369 = ORIENTED_EDGE ( 'NONE', *, *, #87402, .T. ) ;
#120370 = DIRECTION ( 'NONE',  ( -0.000000000000000000, 1.000000000000000000, -0.000000000000000000 ) ) ;
#120371 = CARTESIAN_POINT ( 'NONE',  ( 1.649999999999950617, 2.500000000000000000, -2.165063509461101710 ) ) ;
#120372 = CARTESIAN_POINT ( 'NONE',  ( 12.09999999999990195, 2.500000000000000000, -0.7928203230275542301 ) ) ;
#120374 = EDGE_LOOP ( 'NONE', ( #85489, #53610, #81943, #33983 ) ) ;
#120373 = DIRECTION ( 'NONE',  ( 0.000000000000000000, 0.000000000000000000, 1.000000000000000000 ) ) ;
#120375 = CARTESIAN_POINT ( 'NONE',  ( 0.5999999999999551248, 2.500000000000000000, -4.676537180435978769 ) ) ;
#120376 = AXIS2_PLACEMENT_3D ( 'NONE', #107241, #45759, #115774 ) ;
#120377 = PLANE ( 'NONE',  #91717 ) ;
#120378 = VERTEX_POINT ( 'NONE', #51740 ) ;
#120379 = EDGE_LOOP ( 'NONE', ( #65341, #95235, #117968, #107978 ) ) ;
#120380 = ORIENTED_EDGE ( 'NONE', *, *, #40847, .T. ) ;
#120381 = VERTEX_POINT ( 'NONE', #91652 ) ;
#120382 = CARTESIAN_POINT ( 'NONE',  ( 162.5000000000000000, 0.5000000000000000000, 7.499999999999994671 ) ) ;
#120383 = AXIS2_PLACEMENT_3D ( 'NONE', #121089, #22268, #120448 ) ;
#120384 = AXIS2_PLACEMENT_3D ( 'NONE', #127200, #115394, #85948 ) ;
#120385 = DIRECTION ( 'NONE',  ( -0.000000000000000000, -1.000000000000000000, -0.000000000000000000 ) ) ;
#120386 = CARTESIAN_POINT ( 'NONE',  ( -3.750000000000026201, 12.50000000000000000, 5.802370205355744659 ) ) ;
#120387 = AXIS2_PLACEMENT_3D ( 'NONE', #54562, #56501, #96418 ) ;
#120388 = DIRECTION ( 'NONE',  ( 0.000000000000000000, -0.9999939076577903929, 0.003490651415223739937 ) ) ;
#120389 = ORIENTED_EDGE ( 'NONE', *, *, #95807, .T. ) ;
#120390 = DIRECTION ( 'NONE',  ( -4.274815082592931898E-19, -0.9999939076577903929, -0.003490651415223739937 ) ) ;
#120391 = CARTESIAN_POINT ( 'NONE',  ( -3.150000000000030109, 12.50000000000000000, 1.818653347947321475 ) ) ;
#120392 = CARTESIAN_POINT ( 'NONE',  ( -9.150000000000009237, 12.50000000000000000, 2.165063509461097713 ) ) ;
#120393 = DIRECTION ( 'NONE',  ( 0.000000000000000000, 0.000000000000000000, 1.000000000000000000 ) ) ;
#120394 = EDGE_CURVE ( 'NONE', #79468, #44082, #62214, .T. ) ;
#120395 = AXIS2_PLACEMENT_3D ( 'NONE', #89012, #20908, #58268 ) ;
#120396 = EDGE_CURVE ( 'NONE', #62169, #18680, #68640, .T. ) ;
#120397 = VERTEX_POINT ( 'NONE', #7122 ) ;
#120398 = DIRECTION ( 'NONE',  ( 0.000000000000000000, 0.000000000000000000, -1.000000000000000000 ) ) ;
#120401 = ADVANCED_FACE ( 'NONE', ( #64762 ), #62401, .T. ) ;
#120400 = VECTOR ( 'NONE', #20483, 1000.000000000000000 ) ;
#120399 = CIRCLE ( 'NONE', #66008, 0.06509327318403745899 ) ;
#120402 = ORIENTED_EDGE ( 'NONE', *, *, #77347, .F. ) ;
#120403 = ORIENTED_EDGE ( 'NONE', *, *, #24749, .F. ) ;
#120404 = CARTESIAN_POINT ( 'NONE',  ( 1.649999999999951061, 2.500000000000000000, -6.495190528383302464 ) ) ;
#120405 = CARTESIAN_POINT ( 'NONE',  ( 0.3999999999999619971, 12.50000000000000000, 0.06509327318403732021 ) ) ;
#120406 = FACE_BOUND ( 'NONE', #11410, .T. ) ;
#120407 = DIRECTION ( 'NONE',  ( 0.000000000000000000, 1.000000000000000000, 0.000000000000000000 ) ) ;
#120408 = DIRECTION ( 'NONE',  ( 0.000000000000000000, 0.000000000000000000, -1.000000000000000000 ) ) ;
#120409 = EDGE_CURVE ( 'NONE', #72896, #101165, #5920, .T. ) ;
#120410 = DIRECTION ( 'NONE',  ( 0.000000000000000000, 1.000000000000000000, 0.000000000000000000 ) ) ;
#120411 = VECTOR ( 'NONE', #11934, 1000.000000000000000 ) ;
#120412 = CARTESIAN_POINT ( 'NONE',  ( -5.850000000000021849, 12.50000000000000000, -1.472243186433550122 ) ) ;
#120413 = DIRECTION ( 'NONE',  ( 0.000000000000000000, -0.9999939076577903929, 0.003490651415223739937 ) ) ;
#120414 = FACE_OUTER_BOUND ( 'NONE', #19101, .T. ) ;
#120415 = ORIENTED_EDGE ( 'NONE', *, *, #100692, .T. ) ;
#120416 = CARTESIAN_POINT ( 'NONE',  ( -14.54999999999998472, 2.500000000000000000, 2.165063509461101265 ) ) ;
#120417 = DIRECTION ( 'NONE',  ( -4.274815082592931898E-19, -0.9999939076577903929, -0.003490651415223739937 ) ) ;
#120418 = VERTEX_POINT ( 'NONE', #37260 ) ;
#120419 = VERTEX_POINT ( 'NONE', #55596 ) ;
#120420 = CARTESIAN_POINT ( 'NONE',  ( 13.54999999999989591, 2.500000000000000000, -1.818653347947326138 ) ) ;
#120421 = DIRECTION ( 'NONE',  ( 0.000000000000000000, 0.000000000000000000, -1.000000000000000000 ) ) ;
#120422 = EDGE_CURVE ( 'NONE', #119869, #100266, #20811, .T. ) ;
#120423 = FACE_BOUND ( 'NONE', #61923, .T. ) ;
#120424 = CARTESIAN_POINT ( 'NONE',  ( 11.24999999999990763, 12.50000000000000000, 1.472243186433545459 ) ) ;
#120425 = CIRCLE ( 'NONE', #11753, 0.09999999999999982514 ) ;
#120426 = DIRECTION ( 'NONE',  ( -0.000000000000000000, -1.000000000000000000, -0.000000000000000000 ) ) ;
#120427 = AXIS2_PLACEMENT_3D ( 'NONE', #21029, #80609, #81868 ) ;
#120428 = ORIENTED_EDGE ( 'NONE', *, *, #105752, .T. ) ;
#120429 = CARTESIAN_POINT ( 'NONE',  ( 87.49999999944498086, 3.974992050012154277, 6.359987280019447020 ) ) ;
#120430 = CARTESIAN_POINT ( 'NONE',  ( 184.9583333333333144, 4.445597072760117285, 7.699999999999999289 ) ) ;
#120431 = ORIENTED_EDGE ( 'NONE', *, *, #83395, .F. ) ;
#120432 = PLANE ( 'NONE',  #21892 ) ;
#120433 = CARTESIAN_POINT ( 'NONE',  ( 186.6979166673494603, 6.668395609140176816, 3.850000000000000977 ) ) ;
#120435 = AXIS2_PLACEMENT_3D ( 'NONE', #50874, #71807, #9658 ) ;
#120434 = AXIS2_PLACEMENT_3D ( 'NONE', #68358, #128611, #67711 ) ;
#120436 = EDGE_CURVE ( 'NONE', #51752, #29463, #58486, .T. ) ;
#120437 = DIRECTION ( 'NONE',  ( 0.000000000000000000, 0.000000000000000000, 1.000000000000000000 ) ) ;
#120438 = DIRECTION ( 'NONE',  ( -0.000000000000000000, -1.000000000000000000, -0.000000000000000000 ) ) ;
#120439 = VECTOR ( 'NONE', #47927, 1000.000000000000000 ) ;
#120440 = VERTEX_POINT ( 'NONE', #77171 ) ;
#120441 = AXIS2_PLACEMENT_3D ( 'NONE', #96962, #28236, #68142 ) ;
#120442 = CARTESIAN_POINT ( 'NONE',  ( -7.100000000000013856, 12.50000000000000000, 3.572213422710607489 ) ) ;
#120443 = CARTESIAN_POINT ( 'NONE',  ( -10.20000000000000639, 2.500000000000000000, -4.083716857408422385 ) ) ;
#120444 = FACE_OUTER_BOUND ( 'NONE', #128934, .T. ) ;
#120445 = ORIENTED_EDGE ( 'NONE', *, *, #127592, .T. ) ;
#120446 = ORIENTED_EDGE ( 'NONE', *, *, #52106, .F. ) ;
#120447 = EDGE_CURVE ( 'NONE', #7522, #126712, #56860, .T. ) ;
#120448 = DIRECTION ( 'NONE',  ( 0.000000000000000000, 0.000000000000000000, -1.000000000000000000 ) ) ;
#120449 = EDGE_LOOP ( 'NONE', ( #84203, #111907 ) ) ;
#120450 = DIRECTION ( 'NONE',  ( 0.000000000000000000, -0.000000000000000000, 1.000000000000000000 ) ) ;
#120451 = CARTESIAN_POINT ( 'NONE',  ( 17.50000000000000000, -2.499999999999999556, 0.6666666666666717367 ) ) ;
#120452 = DIRECTION ( 'NONE',  ( 0.000000000000000000, 0.000000000000000000, 1.000000000000000000 ) ) ;
#120453 = ORIENTED_EDGE ( 'NONE', *, *, #111630, .T. ) ;
#120454 = CARTESIAN_POINT ( 'NONE',  ( 6.249999999999967137, 2.500000000000000000, -2.065063509461102065 ) ) ;
#120455 = DIRECTION ( 'NONE',  ( 0.000000000000000000, 0.000000000000000000, 1.000000000000000000 ) ) ;
#120456 = DIRECTION ( 'NONE',  ( -0.000000000000000000, 1.000000000000000000, -0.000000000000000000 ) ) ;
#120457 = CARTESIAN_POINT ( 'NONE',  ( -11.05000000000000071, 2.500000000000000000, -6.841600689897075149 ) ) ;
#120458 = DIRECTION ( 'NONE',  ( -1.000000000000000000, 0.000000000000000000, 0.000000000000000000 ) ) ;
#120459 = DIRECTION ( 'NONE',  ( 0.000000000000000000, -0.000000000000000000, 1.000000000000000000 ) ) ;
#120460 = VERTEX_POINT ( 'NONE', #94226 ) ;
#120461 = ORIENTED_EDGE ( 'NONE', *, *, #52211, .T. ) ;
#120462 = CARTESIAN_POINT ( 'NONE',  ( 11.64999999999990266, 2.500000000000000000, -6.495190528383302464 ) ) ;
#120463 = VERTEX_POINT ( 'NONE', #46408 ) ;
#120464 = CONICAL_SURFACE ( 'NONE', #1326, 0.09999999999999999167, 0.003490658503988666988 ) ;
#120465 = CARTESIAN_POINT ( 'NONE',  ( 104.2474658290071687, 6.952256801654628227, 3.319715706849921677 ) ) ;
#120467 = EDGE_LOOP ( 'NONE', ( #105341, #89618, #44779, #87930 ) ) ;
#120466 = ORIENTED_EDGE ( 'NONE', *, *, #57148, .T. ) ;
#120468 = AXIS2_PLACEMENT_3D ( 'NONE', #66030, #48331, #58169 ) ;
#120469 = ORIENTED_EDGE ( 'NONE', *, *, #122243, .T. ) ;
#120470 = DIRECTION ( 'NONE',  ( 0.000000000000000000, 0.000000000000000000, 1.000000000000000000 ) ) ;
#120471 = CIRCLE ( 'NONE', #30606, 0.06509327318403745899 ) ;
#120472 = AXIS2_PLACEMENT_3D ( 'NONE', #100311, #42032, #52481 ) ;
#120473 = CARTESIAN_POINT ( 'NONE',  ( -11.84999999999999609, 12.50000000000000000, 6.841600689897072485 ) ) ;
#120474 = DIRECTION ( 'NONE',  ( 0.000000000000000000, 0.000000000000000000, 1.000000000000000000 ) ) ;
#120475 = AXIS2_PLACEMENT_3D ( 'NONE', #43171, #14313, #24800 ) ;
#120476 = EDGE_CURVE ( 'NONE', #23253, #98415, #98160, .T. ) ;
#120477 = SURFACE_STYLE_FILL_AREA ( #91657 ) ;
#120478 = CARTESIAN_POINT ( 'NONE',  ( -6.650000000000018119, 12.50000000000000000, -2.922977105672691422 ) ) ;
#120479 = LINE ( 'NONE', #81829, #6199 ) ;
#120480 = CARTESIAN_POINT ( 'NONE',  ( -1.450000000000035039, 2.500000000000000000, -6.841600689897077814 ) ) ;
#120481 = DIRECTION ( 'NONE',  ( -0.000000000000000000, -1.000000000000000000, -0.000000000000000000 ) ) ;
#120482 = DIRECTION ( 'NONE',  ( -0.000000000000000000, -1.000000000000000000, -0.000000000000000000 ) ) ;
#120483 = PLANE ( 'NONE',  #95846 ) ;
#120484 = AXIS2_PLACEMENT_3D ( 'NONE', #19459, #128805, #39776 ) ;
#120485 = ADVANCED_FACE ( 'NONE', ( #104679 ), #104148, .T. ) ;
#120486 = ORIENTED_EDGE ( 'NONE', *, *, #54768, .F. ) ;
#120488 = CIRCLE ( 'NONE', #11813, 0.06509327318403745899 ) ;
#120487 = CIRCLE ( 'NONE', #53596, 0.1000000000000002554 ) ;
#120489 = CARTESIAN_POINT ( 'NONE',  ( 10.59999999999990905, 2.500000000000000000, -4.676537180435978769 ) ) ;
#120490 = ADVANCED_FACE ( 'NONE', ( #105985 ), #7990, .T. ) ;
#120491 = VERTEX_POINT ( 'NONE', #96157 ) ;
#120492 = EDGE_CURVE ( 'NONE', #58724, #34741, #76960, .T. ) ;
#120493 = VERTEX_POINT ( 'NONE', #26780 ) ;
#120494 = ADVANCED_FACE ( 'NONE', ( #26144 ), #110683, .T. ) ;
#120495 = CARTESIAN_POINT ( 'NONE',  ( 5.799999999999933209, 2.500000000000000000, 0.09999999999999761857 ) ) ;
#120496 = ADVANCED_FACE ( 'NONE', ( #4528 ), #70982, .T. ) ;
#120497 = DIRECTION ( 'NONE',  ( 0.000000000000000000, 0.000000000000000000, -1.000000000000000000 ) ) ;
#120498 = CARTESIAN_POINT ( 'NONE',  ( -12.49999999999999289, 2.500000000000000000, -5.022947341949751454 ) ) ;
#120499 = DIRECTION ( 'NONE',  ( 0.000000000000000000, 0.000000000000000000, 1.000000000000000000 ) ) ;
#120500 = DIRECTION ( 'NONE',  ( 0.000000000000000000, 1.000000000000000000, 0.000000000000000000 ) ) ;
#120501 = EDGE_CURVE ( 'NONE', #84780, #80574, #104430, .T. ) ;
#120502 = CARTESIAN_POINT ( 'NONE',  ( -10.00000000000000355, 2.500000000000000000, 3.537306695894645081 ) ) ;
#120503 = ORIENTED_EDGE ( 'NONE', *, *, #121181, .T. ) ;
#120504 = EDGE_CURVE ( 'NONE', #26800, #100851, #54262, .T. ) ;
#120505 = ADVANCED_FACE ( 'NONE', ( #66054 ), #31292, .T. ) ;
#120506 = EDGE_CURVE ( 'NONE', #85926, #4878, #48013, .T. ) ;
#120507 = ORIENTED_EDGE ( 'NONE', *, *, #10512, .F. ) ;
#120508 = CARTESIAN_POINT ( 'NONE',  ( 16.56576425165006228, 2.500000000000000444, -6.084390597445811011 ) ) ;
#120509 = EDGE_CURVE ( 'NONE', #42494, #65236, #125607, .T. ) ;
#120510 = ORIENTED_EDGE ( 'NONE', *, *, #35993, .T. ) ;
#120511 = CARTESIAN_POINT ( 'NONE',  ( 9.149999999999920419, 2.500000000000000000, 1.572243186433545548 ) ) ;
#120512 = ORIENTED_EDGE ( 'NONE', *, *, #117667, .F. ) ;
#120513 = ORIENTED_EDGE ( 'NONE', *, *, #74726, .T. ) ;
#120514 = EDGE_CURVE ( 'NONE', #86064, #72341, #93683, .T. ) ;
#120515 = PLANE ( 'NONE',  #4314 ) ;
#120516 = DIRECTION ( 'NONE',  ( 0.000000000000000000, 1.000000000000000000, 0.000000000000000000 ) ) ;
#120517 = CONICAL_SURFACE ( 'NONE', #24374, 0.1000000000000002554, 0.003490658503988666988 ) ;
#120518 = CARTESIAN_POINT ( 'NONE',  ( -7.100000000000014744, 12.50000000000000000, 4.265033745738159077 ) ) ;
#120520 = LINE ( 'NONE', #110685, #19631 ) ;
#120519 = CIRCLE ( 'NONE', #22331, 0.09999999999999982514 ) ;
#120521 = CARTESIAN_POINT ( 'NONE',  ( -9.600000000000008527, 2.500000000000000000, -4.922947341949749145 ) ) ;
#120522 = VERTEX_POINT ( 'NONE', #18243 ) ;
#120523 = SHAPE_REPRESENTATION ( 'Rechargeable Battery Pack Module', ( #108296 ), #47765 ) ;
#120524 = DIRECTION ( 'NONE',  ( 0.000000000000000000, 0.000000000000000000, -1.000000000000000000 ) ) ;
#120525 = DIRECTION ( 'NONE',  ( -0.000000000000000000, -1.000000000000000000, -0.000000000000000000 ) ) ;
#120526 = DIRECTION ( 'NONE',  ( 0.000000000000000000, 1.000000000000000000, 0.000000000000000000 ) ) ;
#120527 = DIRECTION ( 'NONE',  ( 0.000000000000000000, 1.000000000000000000, 0.000000000000000000 ) ) ;
#120529 = CIRCLE ( 'NONE', #103799, 0.1000000000000000472 ) ;
#120528 = AXIS2_PLACEMENT_3D ( 'NONE', #60349, #108771, #51810 ) ;
#120530 = DIRECTION ( 'NONE',  ( 0.000000000000000000, 0.000000000000000000, 1.000000000000000000 ) ) ;
#120531 = VERTEX_POINT ( 'NONE', #127561 ) ;
#120532 = VERTEX_POINT ( 'NONE', #129525 ) ;
#120533 = CARTESIAN_POINT ( 'NONE',  ( -5.600000000000020073, 12.50000000000000000, -0.3464101615137782364 ) ) ;
#120534 = ORIENTED_EDGE ( 'NONE', *, *, #35579, .F. ) ;
#120535 = AXIS2_PLACEMENT_3D ( 'NONE', #44586, #95619, #104765 ) ;
#120536 = DIRECTION ( 'NONE',  ( 0.000000000000000000, 0.000000000000000000, -1.000000000000000000 ) ) ;
#120537 = DIRECTION ( 'NONE',  ( 0.000000000000000000, 0.000000000000000000, 1.000000000000000000 ) ) ;
#120538 = CONICAL_SURFACE ( 'NONE', #47385, 0.09999999999999982514, 0.003490658503988666988 ) ;
#120539 = ORIENTED_EDGE ( 'NONE', *, *, #5526, .F. ) ;
#120540 = CARTESIAN_POINT ( 'NONE',  ( -8.350000000000013856, 2.500000000000000000, -5.902370205355745192 ) ) ;
#120541 = DIRECTION ( 'NONE',  ( 0.000000000000000000, 0.000000000000000000, -1.000000000000000000 ) ) ;
#120542 = DIRECTION ( 'NONE',  ( 0.000000000000000000, 0.000000000000000000, 1.000000000000000000 ) ) ;
#120543 = DIRECTION ( 'NONE',  ( 0.000000000000000000, 0.000000000000000000, 1.000000000000000000 ) ) ;
#120544 = EDGE_CURVE ( 'NONE', #23954, #87583, #85367, .T. ) ;
#120545 = CARTESIAN_POINT ( 'NONE',  ( -0.8000000000000381251, 12.50000000000000000, 4.265033745738159077 ) ) ;
#120546 = EDGE_CURVE ( 'NONE', #68963, #68394, #53978, .T. ) ;
#120547 = ORIENTED_EDGE ( 'NONE', *, *, #117075, .F. ) ;
#120548 = CARTESIAN_POINT ( 'NONE',  ( 76.45352548353409361, 3.568407488302709041, -6.085611496483662286 ) ) ;
#120549 = CIRCLE ( 'NONE', #126813, 0.06509327318403745899 ) ;
#120550 = DIRECTION ( 'NONE',  ( 0.000000000000000000, 0.000000000000000000, 1.000000000000000000 ) ) ;
#120551 = CARTESIAN_POINT ( 'NONE',  ( -2.900000000000029221, 12.50000000000000000, -0.7579135962115916003 ) ) ;
#120552 = AXIS2_PLACEMENT_3D ( 'NONE', #175, #98377, #108845 ) ;
#120553 = EDGE_CURVE ( 'NONE', #45205, #17761, #9070, .T. ) ;
#120554 = CARTESIAN_POINT ( 'NONE',  ( 11.64999999999990621, 2.500000000000000000, -2.265063509461101798 ) ) ;
#120555 = VERTEX_POINT ( 'NONE', #90189 ) ;
#120556 = CIRCLE ( 'NONE', #1415, 0.06509327318403745899 ) ;
#120557 = VERTEX_POINT ( 'NONE', #118376 ) ;
#120558 = CARTESIAN_POINT ( 'NONE',  ( 108.0000000000000142, 8.500000000000000000, 4.500000000000003553 ) ) ;
#120559 = DIRECTION ( 'NONE',  ( 0.000000000000000000, 0.000000000000000000, 1.000000000000000000 ) ) ;
#120560 = AXIS2_PLACEMENT_3D ( 'NONE', #27218, #107720, #68431 ) ;
#120561 = CARTESIAN_POINT ( 'NONE',  ( 7.699999999999925571, 2.500000000000000000, -4.576537180435978236 ) ) ;
#120562 = AXIS2_PLACEMENT_3D ( 'NONE', #34147, #35440, #77753 ) ;
#120563 = ORIENTED_EDGE ( 'NONE', *, *, #59932, .T. ) ;
#120564 = CARTESIAN_POINT ( 'NONE',  ( 8.949999999999915801, 2.500000000000000000, -1.918653347947326004 ) ) ;
#120565 = VECTOR ( 'NONE', #71417, 1000.000000000000000 ) ;
#120566 = CARTESIAN_POINT ( 'NONE',  ( 7.949999999999922018, 2.500000000000000000, -2.165063509461101710 ) ) ;
#120567 = ORIENTED_EDGE ( 'NONE', *, *, #37299, .T. ) ;
#120568 = CARTESIAN_POINT ( 'NONE',  ( 4.399999999999940847, 12.50000000000000000, -4.741630453620015118 ) ) ;
#120569 = AXIS2_PLACEMENT_3D ( 'NONE', #90335, #129027, #99548 ) ;
#120570 = VERTEX_POINT ( 'NONE', #87622 ) ;
#120571 = CARTESIAN_POINT ( 'NONE',  ( -6.050000000000018474, 2.500000000000000000, 6.741600689897071952 ) ) ;
#120573 = AXIS2_PLACEMENT_3D ( 'NONE', #55578, #6435, #116414 ) ;
#120572 = CIRCLE ( 'NONE', #51635, 0.1000000000000002554 ) ;
#120574 = EDGE_LOOP ( 'NONE', ( #33138, #102600, #98380, #3057 ) ) ;
#120575 = DIRECTION ( 'NONE',  ( -4.274815082592931898E-19, -0.9999939076577903929, -0.003490651415223739937 ) ) ;
#120576 = DIRECTION ( 'NONE',  ( -0.000000000000000000, -1.000000000000000000, -0.000000000000000000 ) ) ;
#120577 = ORIENTED_EDGE ( 'NONE', *, *, #64781, .T. ) ;
#120578 = ORIENTED_EDGE ( 'NONE', *, *, #21012, .T. ) ;
#120579 = DIRECTION ( 'NONE',  ( 0.000000000000000000, 0.000000000000000000, -1.000000000000000000 ) ) ;
#120580 = CARTESIAN_POINT ( 'NONE',  ( -6.700000000000016165, 12.50000000000000000, 4.330127018922196314 ) ) ;
#120581 = VERTEX_POINT ( 'NONE', #109193 ) ;
#120583 = ADVANCED_FACE ( 'NONE', ( #40493 ), #87407, .T. ) ;
#120582 = FACE_OUTER_BOUND ( 'NONE', #29909, .T. ) ;
#120584 = DIRECTION ( 'NONE',  ( 0.000000000000000000, 0.000000000000000000, -1.000000000000000000 ) ) ;
#120585 = DIRECTION ( 'NONE',  ( 0.000000000000000000, 0.000000000000000000, 1.000000000000000000 ) ) ;
#120586 = CARTESIAN_POINT ( 'NONE',  ( 103.2667367461191077, 8.548823231429411251, 1.644105246313542157 ) ) ;
#120587 = CARTESIAN_POINT ( 'NONE',  ( 15.59999999999988951, 2.500000000000000000, -0.3464101615137783474 ) ) ;
#120588 = DIRECTION ( 'NONE',  ( 0.000000000000000000, 1.000000000000000000, 0.000000000000000000 ) ) ;
#120589 = CARTESIAN_POINT ( 'NONE',  ( 14.34999999999989306, 12.50000000000000000, -2.511473670974877948 ) ) ;
#120590 = CIRCLE ( 'NONE', #91343, 0.06509327318403745899 ) ;
#120591 = EDGE_LOOP ( 'NONE', ( #48122, #76583, #76547, #39174 ) ) ;
#120592 = VERTEX_POINT ( 'NONE', #79120 ) ;
#120593 = CARTESIAN_POINT ( 'NONE',  ( -1.050000000000037348, 2.500000000000000000, -6.741600689897078169 ) ) ;
#120594 = ORIENTED_EDGE ( 'NONE', *, *, #76930, .F. ) ;
#120595 = DIRECTION ( 'NONE',  ( -4.274815082592931898E-19, -0.9999939076577903929, -0.003490651415223739937 ) ) ;
#120596 = DIRECTION ( 'NONE',  ( 0.000000000000000000, 0.000000000000000000, 1.000000000000000000 ) ) ;
#120597 = ADVANCED_FACE ( 'NONE', ( #88254 ), #58200, .T. ) ;
#120598 = PLANE ( 'NONE',  #95003 ) ;
#120600 = EDGE_LOOP ( 'NONE', ( #94614, #86150, #41466, #81746 ) ) ;
#120599 = ORIENTED_EDGE ( 'NONE', *, *, #34689, .F. ) ;
#120601 = FACE_BOUND ( 'NONE', #12855, .T. ) ;
#120602 = ORIENTED_EDGE ( 'NONE', *, *, #37642, .T. ) ;
#120603 = EDGE_CURVE ( 'NONE', #117308, #89205, #30019, .T. ) ;
#120604 = DIRECTION ( 'NONE',  ( 0.000000000000000000, 0.000000000000000000, -1.000000000000000000 ) ) ;
#120605 = CARTESIAN_POINT ( 'NONE',  ( 186.5000000000000000, 0.000000000000000000, 7.700000000000000178 ) ) ;
#120606 = CARTESIAN_POINT ( 'NONE',  ( -3.750000000000027978, 2.500000000000000000, 7.088010851410848190 ) ) ;
#120607 = CARTESIAN_POINT ( 'NONE',  ( 2.949999999999943334, 2.500000000000000000, 6.395190528383296602 ) ) ;
#120608 = AXIS2_PLACEMENT_3D ( 'NONE', #97436, #117062, #37877 ) ;
#120609 = FACE_OUTER_BOUND ( 'NONE', #102643, .T. ) ;
#120610 = CIRCLE ( 'NONE', #89304, 0.06509327318403745899 ) ;
#120611 = CARTESIAN_POINT ( 'NONE',  ( 10.84999999999990905, 2.500000000000000000, -5.802370205355749988 ) ) ;
#120612 = CARTESIAN_POINT ( 'NONE',  ( 0.1999999999999571565, 12.50000000000000000, 3.918623584224382839 ) ) ;
#120613 = DIRECTION ( 'NONE',  ( -4.274815082592931898E-19, -0.9999939076577903929, -0.003490651415223739937 ) ) ;
#120614 = EDGE_CURVE ( 'NONE', #56986, #47494, #38562, .T. ) ;
#120615 = FACE_OUTER_BOUND ( 'NONE', #125912, .T. ) ;
#120616 = CARTESIAN_POINT ( 'NONE',  ( -1.850000000000033840, 2.500000000000000000, 2.511473670974873507 ) ) ;
#120617 = AXIS2_PLACEMENT_3D ( 'NONE', #67371, #56292, #15721 ) ;
#120618 = EDGE_LOOP ( 'NONE', ( #32749, #81157, #116862, #57337 ) ) ;
#120619 = VERTEX_POINT ( 'NONE', #49664 ) ;
#120620 = ORIENTED_EDGE ( 'NONE', *, *, #11416, .F. ) ;
#120621 = ORIENTED_EDGE ( 'NONE', *, *, #61669, .F. ) ;
#120622 = CARTESIAN_POINT ( 'NONE',  ( -8.350000000000008527, 2.500000000000000000, 7.188010851410848723 ) ) ;
#120623 = CARTESIAN_POINT ( 'NONE',  ( 2.000000000000000000, 0.000000000000000000, 6.000000000000005329 ) ) ;
#120625 = ORIENTED_EDGE ( 'NONE', *, *, #94725, .T. ) ;
#120624 = ORIENTED_EDGE ( 'NONE', *, *, #39990, .T. ) ;
#120626 = ORIENTED_EDGE ( 'NONE', *, *, #86041, .T. ) ;
#120627 = CARTESIAN_POINT ( 'NONE',  ( -6.050000000000020250, 12.50000000000000000, -6.841600689897078702 ) ) ;
#120629 = AXIS2_PLACEMENT_3D ( 'NONE', #117813, #28168, #36710 ) ;
#120628 = AXIS2_PLACEMENT_3D ( 'NONE', #110999, #71752, #12800 ) ;
#120630 = VECTOR ( 'NONE', #93870, 1000.000000000000000 ) ;
#120631 = CARTESIAN_POINT ( 'NONE',  ( 6.649999999999930189, 12.50000000000000000, -1.472243186433550122 ) ) ;
#120632 = CARTESIAN_POINT ( 'NONE',  ( 12.69999999999990337, 12.50000000000000000, -4.676537180435978769 ) ) ;
#120633 = FACE_OUTER_BOUND ( 'NONE', #74380, .T. ) ;
#120634 = CYLINDRICAL_SURFACE ( 'NONE', #12151, 2.318304356886073059 ) ;
#120635 = DIRECTION ( 'NONE',  ( 0.000000000000000000, 0.000000000000000000, -1.000000000000000000 ) ) ;
#120636 = EDGE_LOOP ( 'NONE', ( #73437, #105957 ) ) ;
#120637 = LINE ( 'NONE', #70898, #122847 ) ;
#120638 = VERTEX_POINT ( 'NONE', #19533 ) ;
#120639 = ADVANCED_FACE ( 'NONE', ( #69265 ), #104245, .T. ) ;
#120640 = VERTEX_POINT ( 'NONE', #59499 ) ;
#120641 = VERTEX_POINT ( 'NONE', #107270 ) ;
#120642 = CARTESIAN_POINT ( 'NONE',  ( 3.949999999999938005, 2.500000000000000000, 6.741600689897071952 ) ) ;
#120643 = ORIENTED_EDGE ( 'NONE', *, *, #93037, .F. ) ;
#120644 = ADVANCED_FACE ( 'NONE', ( #17589 ), #49019, .T. ) ;
#120645 = EDGE_LOOP ( 'NONE', ( #19712, #128825, #61764, #44888 ) ) ;
#120646 = EDGE_LOOP ( 'NONE', ( #108341, #98124 ) ) ;
#120647 = CONICAL_SURFACE ( 'NONE', #99728, 0.1000000000000002554, 0.003490658503988666988 ) ;
#120648 = EDGE_CURVE ( 'NONE', #89168, #85675, #81261, .T. ) ;
#120649 = CARTESIAN_POINT ( 'NONE',  ( 13.09999999999989839, 2.500000000000000000, -0.3464101615137783474 ) ) ;
#120650 = FACE_OUTER_BOUND ( 'NONE', #35418, .T. ) ;
#120652 = CIRCLE ( 'NONE', #9830, 0.06509327318403745899 ) ;
#120651 = CARTESIAN_POINT ( 'NONE',  ( -8.150000000000009237, 12.50000000000000000, 6.148780366869520009 ) ) ;
#120653 = LINE ( 'NONE', #99735, #52607 ) ;
#120654 = CARTESIAN_POINT ( 'NONE',  ( -7.700000000000016165, 12.50000000000000000, 0.3464101615137735735 ) ) ;
#120655 = EDGE_CURVE ( 'NONE', #97694, #72972, #95838, .T. ) ;
#120656 = DIRECTION ( 'NONE',  ( -0.000000000000000000, -1.000000000000000000, -0.000000000000000000 ) ) ;
#120657 = ADVANCED_FACE ( 'NONE', ( #28075 ), #58823, .T. ) ;
#120658 = EDGE_CURVE ( 'NONE', #113211, #100972, #118906, .T. ) ;
#120659 = AXIS2_PLACEMENT_3D ( 'NONE', #40277, #120765, #61201 ) ;
#120660 = DIRECTION ( 'NONE',  ( -4.274815082592931898E-19, -0.9999939076577903929, -0.003490651415223739937 ) ) ;
#120661 = ORIENTED_EDGE ( 'NONE', *, *, #120026, .F. ) ;
#120662 = AXIS2_PLACEMENT_3D ( 'NONE', #63560, #55009, #53729 ) ;
#120663 = DIRECTION ( 'NONE',  ( 0.000000000000000000, 0.000000000000000000, 1.000000000000000000 ) ) ;
#120664 = EDGE_CURVE ( 'NONE', #84079, #125412, #125177, .T. ) ;
#120665 = ORIENTED_EDGE ( 'NONE', *, *, #114199, .T. ) ;
#120666 = CARTESIAN_POINT ( 'NONE',  ( 109.1593346011806887, 7.211655450534177447, 4.866583586154797025 ) ) ;
#120667 = LINE ( 'NONE', #91852, #71210 ) ;
#120668 = ORIENTED_EDGE ( 'NONE', *, *, #95094, .F. ) ;
#120669 = FACE_OUTER_BOUND ( 'NONE', #33547, .T. ) ;
#120670 = CIRCLE ( 'NONE', #74691, 0.09999999999999982514 ) ;
#120671 = EDGE_CURVE ( 'NONE', #125152, #97372, #111794, .T. ) ;
#120672 = CARTESIAN_POINT ( 'NONE',  ( 9.999999999999948486, 2.500000000000000000, 4.230127018922196669 ) ) ;
#120673 = VERTEX_POINT ( 'NONE', #61416 ) ;
#120674 = ADVANCED_FACE ( 'NONE', ( #62697 ), #82984, .T. ) ;
#120676 = CONICAL_SURFACE ( 'NONE', #37058, 0.1000000000000000472, 0.003490658503988666988 ) ;
#120675 = AXIS2_PLACEMENT_3D ( 'NONE', #47407, #120010, #69609 ) ;
#120677 = DIRECTION ( 'NONE',  ( -0.000000000000000000, -1.000000000000000000, -0.000000000000000000 ) ) ;
#120678 = ORIENTED_EDGE ( 'NONE', *, *, #56586, .F. ) ;
#120679 = ORIENTED_EDGE ( 'NONE', *, *, #50626, .F. ) ;
#120680 = LINE ( 'NONE', #112795, #70636 ) ;
#120681 = CARTESIAN_POINT ( 'NONE',  ( 2.499999999999983569, 2.500000000000000000, -0.1000000000000022815 ) ) ;
#120682 = CARTESIAN_POINT ( 'NONE',  ( 184.5885416670080872, -6.551208109652273848, -3.782341765625003571 ) ) ;
#120683 = DIRECTION ( 'NONE',  ( 0.000000000000000000, 0.000000000000000000, -1.000000000000000000 ) ) ;
#120684 = CARTESIAN_POINT ( 'NONE',  ( 106.0514428414850272, 8.500000000000000000, -1.125000000000000222 ) ) ;
#120685 = ORIENTED_EDGE ( 'NONE', *, *, #29487, .T. ) ;
#120686 = DIRECTION ( 'NONE',  ( -0.000000000000000000, -1.000000000000000000, -0.000000000000000000 ) ) ;
#120687 = VECTOR ( 'NONE', #54908, 1000.000000000000000 ) ;
#120688 = ORIENTED_EDGE ( 'NONE', *, *, #33172, .F. ) ;
#120689 = FACE_OUTER_BOUND ( 'NONE', #41956, .T. ) ;
#120690 = CARTESIAN_POINT ( 'NONE',  ( -13.94999999999998863, 2.500000000000000000, 2.411473670974877415 ) ) ;
#120691 = CARTESIAN_POINT ( 'NONE',  ( 186.8385416670080872, 6.551208109652274736, 3.782341765625001351 ) ) ;
#120692 = DIRECTION ( 'NONE',  ( -0.000000000000000000, -1.000000000000000000, -0.000000000000000000 ) ) ;
#120693 = DIRECTION ( 'NONE',  ( 0.000000000000000000, 1.000000000000000000, 0.000000000000000000 ) ) ;
#120694 = DIRECTION ( 'NONE',  ( -0.000000000000000000, 1.000000000000000000, -0.000000000000000000 ) ) ;
#120695 = CARTESIAN_POINT ( 'NONE',  ( 4.799999999999937650, 12.50000000000000000, -3.983716857408426293 ) ) ;
#120696 = ORIENTED_EDGE ( 'NONE', *, *, #106619, .F. ) ;
#120697 = CIRCLE ( 'NONE', #99870, 0.1000000000000002554 ) ;
#120699 = ADVANCED_FACE ( 'NONE', ( #92803 ), #32615, .T. ) ;
#120698 = CARTESIAN_POINT ( 'NONE',  ( -6.050000000000018474, 12.50000000000000000, 2.511473670974873507 ) ) ;
#120700 = CIRCLE ( 'NONE', #116480, 0.06509327318403745899 ) ;
#120701 = DIRECTION ( 'NONE',  ( -0.000000000000000000, -1.000000000000000000, -0.000000000000000000 ) ) ;
#120702 = DIRECTION ( 'NONE',  ( -0.000000000000000000, -1.000000000000000000, -0.000000000000000000 ) ) ;
#120703 = EDGE_LOOP ( 'NONE', ( #55081, #62532 ) ) ;
#120705 = CIRCLE ( 'NONE', #1565, 0.06509327318403745899 ) ;
#120704 = AXIS2_PLACEMENT_3D ( 'NONE', #99307, #120235, #29282 ) ;
#120706 = CARTESIAN_POINT ( 'NONE',  ( -3.350000000000028511, 2.500000000000000000, -2.757883832488654097 ) ) ;
#120707 = ADVANCED_FACE ( 'NONE', ( #31314 ), #11649, .T. ) ;
#120708 = AXIS2_PLACEMENT_3D ( 'NONE', #21139, #112112, #22458 ) ;
#120709 = ORIENTED_EDGE ( 'NONE', *, *, #26816, .T. ) ;
#120710 = ORIENTED_EDGE ( 'NONE', *, *, #61158, .T. ) ;
#120711 = DIRECTION ( 'NONE',  ( -4.274815082592931898E-19, -0.9999939076577903929, -0.003490651415223739937 ) ) ;
#120712 = ORIENTED_EDGE ( 'NONE', *, *, #98439, .T. ) ;
#120713 = CARTESIAN_POINT ( 'NONE',  ( 19.72570408286242127, -0.6078483229330700066, -4.299616118079172544 ) ) ;
#120714 = DIRECTION ( 'NONE',  ( 0.000000000000000000, 0.000000000000000000, 1.000000000000000000 ) ) ;
#120715 = CARTESIAN_POINT ( 'NONE',  ( 4.599999999999936584, 2.500000000000000000, 4.230127018922196669 ) ) ;
#120716 = CIRCLE ( 'NONE', #62152, 0.06509327318403745899 ) ;
#120717 = VERTEX_POINT ( 'NONE', #70568 ) ;
#120718 = CARTESIAN_POINT ( 'NONE',  ( -11.64999999999999858, 12.50000000000000000, -5.802370205355746435 ) ) ;
#120719 = FACE_OUTER_BOUND ( 'NONE', #82645, .T. ) ;
#120720 = CARTESIAN_POINT ( 'NONE',  ( -2.500000000000030642, 2.500000000000000000, -5.022947341949754119 ) ) ;
#120721 = ORIENTED_EDGE ( 'NONE', *, *, #82506, .F. ) ;
#120722 = AXIS2_PLACEMENT_3D ( 'NONE', #106279, #56524, #103714 ) ;
#120723 = ORIENTED_EDGE ( 'NONE', *, *, #90340, .T. ) ;
#120724 = ORIENTED_EDGE ( 'NONE', *, *, #68252, .F. ) ;
#120725 = CARTESIAN_POINT ( 'NONE',  ( -3.550000000000028688, 2.500000000000000000, 6.741600689897071952 ) ) ;
#120726 = DIRECTION ( 'NONE',  ( 0.000000000000000000, 0.000000000000000000, 1.000000000000000000 ) ) ;
#120727 = CARTESIAN_POINT ( 'NONE',  ( -5.650000000000019895, 2.500000000000000000, 2.411473670974873862 ) ) ;
#120728 = FACE_BOUND ( 'NONE', #68808, .T. ) ;
#120729 = ORIENTED_EDGE ( 'NONE', *, *, #94241, .F. ) ;
#120730 = AXIS2_PLACEMENT_3D ( 'NONE', #5173, #34675, #66673 ) ;
#120731 = DIRECTION ( 'NONE',  ( 0.000000000000000000, 1.000000000000000000, 0.000000000000000000 ) ) ;
#120732 = CARTESIAN_POINT ( 'NONE',  ( 11.24999999999990763, 2.500000000000000000, -7.088010851410853519 ) ) ;
#120733 = EDGE_LOOP ( 'NONE', ( #111423, #69163 ) ) ;
#120735 = EDGE_CURVE ( 'NONE', #18179, #30237, #26877, .T. ) ;
#120734 = FACE_OUTER_BOUND ( 'NONE', #37579, .T. ) ;
#120736 = DIRECTION ( 'NONE',  ( 0.000000000000000000, 0.000000000000000000, 1.000000000000000000 ) ) ;
#120737 = CIRCLE ( 'NONE', #22476, 0.06509327318403745899 ) ;
#120738 = FACE_OUTER_BOUND ( 'NONE', #110005, .T. ) ;
#120739 = CARTESIAN_POINT ( 'NONE',  ( -4.350000000000023626, 12.50000000000000000, 2.511473670974873507 ) ) ;
#120740 = DIRECTION ( 'NONE',  ( 0.000000000000000000, 0.000000000000000000, 1.000000000000000000 ) ) ;
#120741 = DIRECTION ( 'NONE',  ( -0.000000000000000000, 1.000000000000000000, -0.000000000000000000 ) ) ;
#120742 = AXIS2_PLACEMENT_3D ( 'NONE', #40121, #119968, #38864 ) ;
#120743 = CARTESIAN_POINT ( 'NONE',  ( 6.249999999999967137, 2.500000000000000000, -2.265063509461101798 ) ) ;
#120744 = CIRCLE ( 'NONE', #118686, 0.06509327318403745899 ) ;
#120745 = EDGE_CURVE ( 'NONE', #52849, #41301, #37355, .T. ) ;
#120746 = VECTOR ( 'NONE', #111190, 1000.000000000000000 ) ;
#120747 = ORIENTED_EDGE ( 'NONE', *, *, #120201, .F. ) ;
#120748 = ORIENTED_EDGE ( 'NONE', *, *, #11123, .T. ) ;
#120749 = VERTEX_POINT ( 'NONE', #3127 ) ;
#120750 = ORIENTED_EDGE ( 'NONE', *, *, #38028, .T. ) ;
#120751 = DIRECTION ( 'NONE',  ( 0.000000000000000000, 0.000000000000000000, 1.000000000000000000 ) ) ;
#120752 = EDGE_CURVE ( 'NONE', #123701, #119499, #45758, .T. ) ;
#120753 = CARTESIAN_POINT ( 'NONE',  ( -11.64999999999999680, 2.500000000000000000, -2.857883832488649745 ) ) ;
#120754 = AXIS2_PLACEMENT_3D ( 'NONE', #63970, #35796, #65237 ) ;
#120755 = ORIENTED_EDGE ( 'NONE', *, *, #112377, .T. ) ;
#120756 = FACE_BOUND ( 'NONE', #104869, .T. ) ;
#120757 = EDGE_CURVE ( 'NONE', #38170, #26678, #123027, .T. ) ;
#120758 = CARTESIAN_POINT ( 'NONE',  ( -2.900000000000029665, 12.50000000000000000, 3.637306695894644726 ) ) ;
#120759 = CYLINDRICAL_SURFACE ( 'NONE', #61688, 7.700000000000000178 ) ;
#120761 = VECTOR ( 'NONE', #38368, 1000.000000000000000 ) ;
#120760 = AXIS2_PLACEMENT_3D ( 'NONE', #31010, #93134, #122588 ) ;
#120762 = EDGE_CURVE ( 'NONE', #113663, #60541, #77054, .T. ) ;
#120763 = FACE_OUTER_BOUND ( 'NONE', #5959, .T. ) ;
#120764 = CARTESIAN_POINT ( 'NONE',  ( -8.750000000000010658, 12.50000000000000000, -1.472243186433550122 ) ) ;
#120765 = DIRECTION ( 'NONE',  ( 0.000000000000000000, 1.000000000000000000, 0.000000000000000000 ) ) ;
#120766 = CARTESIAN_POINT ( 'NONE',  ( 6.249999999999934275, 2.500000000000000000, -7.088010851410853519 ) ) ;
#120767 = DIRECTION ( 'NONE',  ( 0.000000000000000000, 0.000000000000000000, 1.000000000000000000 ) ) ;
#120768 = ADVANCED_FACE ( 'NONE', ( #12911 ), #73154, .T. ) ;
#120769 = DIRECTION ( 'NONE',  ( -0.000000000000000000, 1.000000000000000000, -0.000000000000000000 ) ) ;
#120770 = VERTEX_POINT ( 'NONE', #111111 ) ;
#120771 = ORIENTED_EDGE ( 'NONE', *, *, #78094, .T. ) ;
#120772 = ORIENTED_EDGE ( 'NONE', *, *, #19716, .F. ) ;
#120773 = ORIENTED_EDGE ( 'NONE', *, *, #118769, .F. ) ;
#120774 = ORIENTED_EDGE ( 'NONE', *, *, #28739, .T. ) ;
#120775 = ORIENTED_EDGE ( 'NONE', *, *, #58112, .F. ) ;
#120776 = LINE ( 'NONE', #51417, #50555 ) ;
#120777 = EDGE_LOOP ( 'NONE', ( #89124, #86881 ) ) ;
#120778 = DIRECTION ( 'NONE',  ( -0.000000000000000000, 1.000000000000000000, -0.000000000000000000 ) ) ;
#120779 = CARTESIAN_POINT ( 'NONE',  ( 16.31212829106973672, -2.500000000000129674, 6.358241997069454143 ) ) ;
#120780 = LINE ( 'NONE', #31138, #129461 ) ;
#120781 = DIRECTION ( 'NONE',  ( 0.000000000000000000, 0.000000000000000000, 1.000000000000000000 ) ) ;
#120782 = VERTEX_POINT ( 'NONE', #101330 ) ;
#120783 = CARTESIAN_POINT ( 'NONE',  ( -10.40000000000000213, 2.500000000000000000, 0.6928203230275494784 ) ) ;
#120784 = AXIS2_PLACEMENT_3D ( 'NONE', #121282, #60456, #100362 ) ;
#120785 = ORIENTED_EDGE ( 'NONE', *, *, #79974, .F. ) ;
#120786 = EDGE_CURVE ( 'NONE', #118189, #95937, #64519, .T. ) ;
#120787 = CIRCLE ( 'NONE', #49797, 0.06509327318403745899 ) ;
#120788 = ORIENTED_EDGE ( 'NONE', *, *, #49179, .T. ) ;
#120789 = CARTESIAN_POINT ( 'NONE',  ( 4.199999999999941558, 12.50000000000000000, -4.395220292106239768 ) ) ;
#120790 = LINE ( 'NONE', #70408, #57339 ) ;
#120791 = FACE_OUTER_BOUND ( 'NONE', #48246, .T. ) ;
#120792 = EDGE_CURVE ( 'NONE', #72819, #119417, #14333, .T. ) ;
#120793 = ORIENTED_EDGE ( 'NONE', *, *, #87357, .F. ) ;
#120796 = ADVANCED_FACE ( 'NONE', ( #63328, #93436 ), #121591, .F. ) ;
#120795 = EDGE_LOOP ( 'NONE', ( #109354, #4330, #83623, #35956 ) ) ;
#120794 = CIRCLE ( 'NONE', #104078, 0.06509327318403745899 ) ;
#120797 = DIRECTION ( 'NONE',  ( -0.000000000000000000, -1.000000000000000000, -0.000000000000000000 ) ) ;
#120798 = VECTOR ( 'NONE', #118534, 1000.000000000000000 ) ;
#120799 = AXIS2_PLACEMENT_3D ( 'NONE', #21793, #71513, #110160 ) ;
#120800 = CARTESIAN_POINT ( 'NONE',  ( 8.299999999999922551, 2.500000000000000000, -2.385244779468109755E-15 ) ) ;
#120801 = DIRECTION ( 'NONE',  ( 0.000000000000000000, 0.000000000000000000, -1.000000000000000000 ) ) ;
#120802 = DIRECTION ( 'NONE',  ( 0.000000000000000000, 1.000000000000000000, 0.000000000000000000 ) ) ;
#120803 = VERTEX_POINT ( 'NONE', #30670 ) ;
#120804 = ADVANCED_FACE ( 'NONE', ( #52229 ), #66574, .T. ) ;
#120805 = CARTESIAN_POINT ( 'NONE',  ( -6.850000000000017408, 2.500000000000000000, -6.741600689897077281 ) ) ;
#120806 = EDGE_CURVE ( 'NONE', #124753, #118132, #87496, .T. ) ;
#120807 = EDGE_CURVE ( 'NONE', #59372, #43527, #72518, .T. ) ;
#120808 = ORIENTED_EDGE ( 'NONE', *, *, #65474, .T. ) ;
#120809 = CARTESIAN_POINT ( 'NONE',  ( 10.06913504599025977, -2.500000000000000444, 8.158951466667735630 ) ) ;
#120810 = CIRCLE ( 'NONE', #125013, 0.06509327318403745899 ) ;
#120811 = ORIENTED_EDGE ( 'NONE', *, *, #98229, .F. ) ;
#120812 = CARTESIAN_POINT ( 'NONE',  ( -5.600000000000023626, 12.50000000000000000, -4.048810130592463530 ) ) ;
#120813 = EDGE_CURVE ( 'NONE', #93332, #26619, #10155, .T. ) ;
#120814 = DIRECTION ( 'NONE',  ( 0.000000000000000000, 1.000000000000000000, 0.000000000000000000 ) ) ;
#120815 = CARTESIAN_POINT ( 'NONE',  ( -3.350000000000031619, 12.50000000000000000, -5.802370205355749988 ) ) ;
#120816 = CONICAL_SURFACE ( 'NONE', #51867, 0.09999999999999982514, 0.003490658503988666988 ) ;
#120817 = CARTESIAN_POINT ( 'NONE',  ( -11.24999999999999822, 2.500000000000000000, 5.802370205355744659 ) ) ;
#120818 = EDGE_LOOP ( 'NONE', ( #50585, #89095, #29216, #22766 ) ) ;
#120819 = ADVANCED_FACE ( 'NONE', ( #125466 ), #41567, .T. ) ;
#120821 = AXIS2_PLACEMENT_3D ( 'NONE', #5756, #27332, #56785 ) ;
#120820 = DIRECTION ( 'NONE',  ( 0.000000000000000000, 0.000000000000000000, -1.000000000000000000 ) ) ;
#120822 = EDGE_CURVE ( 'NONE', #38829, #42322, #116750, .T. ) ;
#120823 = MECHANICAL_DESIGN_GEOMETRIC_PRESENTATION_REPRESENTATION (  '', ( #47672 ), #7945 ) ;
#120824 = CARTESIAN_POINT ( 'NONE',  ( 0.6499999999999561684, 2.500000000000000000, 1.818653347947321475 ) ) ;
#120825 = ORIENTED_EDGE ( 'NONE', *, *, #96267, .T. ) ;
#120826 = ORIENTED_EDGE ( 'NONE', *, *, #53008, .F. ) ;
#120827 = ORIENTED_EDGE ( 'NONE', *, *, #72040, .F. ) ;
#120828 = CARTESIAN_POINT ( 'NONE',  ( -10.60000000000000320, 12.50000000000000000, -4.676537180435973440 ) ) ;
#120829 = CARTESIAN_POINT ( 'NONE',  ( -1.050000000000037348, 2.500000000000000000, -2.411473670974877859 ) ) ;
#120830 = CARTESIAN_POINT ( 'NONE',  ( -1.250000000000036193, 2.500000000000000000, 1.572243186433545548 ) ) ;
#120831 = DIRECTION ( 'NONE',  ( 0.000000000000000000, -0.9999939076577903929, 0.003490651415223739937 ) ) ;
#120832 = VECTOR ( 'NONE', #126595, 1000.000000000000000 ) ;
#120834 = CIRCLE ( 'NONE', #35168, 0.06509327318403745899 ) ;
#120833 = CARTESIAN_POINT ( 'NONE',  ( -11.24999999999999822, 12.50000000000000000, 5.802370205355744659 ) ) ;
#120835 = DIRECTION ( 'NONE',  ( 0.000000000000000000, 0.000000000000000000, 1.000000000000000000 ) ) ;
#120836 = CIRCLE ( 'NONE', #33025, 0.1000000000000000472 ) ;
#120837 = DIRECTION ( 'NONE',  ( -0.000000000000000000, 1.000000000000000000, -0.000000000000000000 ) ) ;
#120838 = DIRECTION ( 'NONE',  ( 0.000000000000000000, -0.9999939076577903929, 0.003490651415223739937 ) ) ;
#120839 = LINE ( 'NONE', #97966, #102774 ) ;
#120840 = CONICAL_SURFACE ( 'NONE', #43210, 0.1000000000000000472, 0.003490658503988666988 ) ;
#120841 = ORIENTED_EDGE ( 'NONE', *, *, #121130, .F. ) ;
#120842 = CARTESIAN_POINT ( 'NONE',  ( 149.5981739382431783, 0.5000000000000000000, -1.703575533167231537 ) ) ;
#120843 = CIRCLE ( 'NONE', #74880, 0.06509327318403745899 ) ;
#120844 = FACE_OUTER_BOUND ( 'NONE', #9552, .T. ) ;
#120845 = DIRECTION ( 'NONE',  ( 0.000000000000000000, 0.000000000000000000, 1.000000000000000000 ) ) ;
#120846 = DIRECTION ( 'NONE',  ( -0.000000000000000000, 1.000000000000000000, -0.000000000000000000 ) ) ;
#120847 = ORIENTED_EDGE ( 'NONE', *, *, #126434, .F. ) ;
#120848 = CARTESIAN_POINT ( 'NONE',  ( -12.09999999999999609, 2.500000000000000000, -0.5928203230275500557 ) ) ;
#120850 = CIRCLE ( 'NONE', #114574, 0.06509327318403745899 ) ;
#120849 = AXIS2_PLACEMENT_3D ( 'NONE', #47900, #11004, #28249 ) ;
#120851 = EDGE_CURVE ( 'NONE', #98415, #23253, #60347, .T. ) ;
#120852 = CARTESIAN_POINT ( 'NONE',  ( 107.5000000000000142, 0.000000000000000000, 0.000000000000000000 ) ) ;
#120854 = EDGE_LOOP ( 'NONE', ( #28107, #12406, #94275, #129030 ) ) ;
#120853 = FACE_OUTER_BOUND ( 'NONE', #13090, .T. ) ;
#120855 = ORIENTED_EDGE ( 'NONE', *, *, #93055, .F. ) ;
#120856 = DIRECTION ( 'NONE',  ( 0.000000000000000000, -0.9999939076577903929, 0.003490651415223739937 ) ) ;
#120857 = EDGE_CURVE ( 'NONE', #79541, #2654, #110500, .T. ) ;
#120858 = EDGE_LOOP ( 'NONE', ( #65288, #27713 ) ) ;
#120859 = ORIENTED_EDGE ( 'NONE', *, *, #79877, .T. ) ;
#120860 = DIRECTION ( 'NONE',  ( -0.000000000000000000, -1.000000000000000000, -0.000000000000000000 ) ) ;
#120861 = DIRECTION ( 'NONE',  ( 0.000000000000000000, 0.000000000000000000, -1.000000000000000000 ) ) ;
#120862 = CARTESIAN_POINT ( 'NONE',  ( 8.749999999999923617, 2.500000000000000000, 1.372243186433545370 ) ) ;
#120863 = CARTESIAN_POINT ( 'NONE',  ( 9.399999999999915090, 2.500000000000000000, 3.983716857408420964 ) ) ;
#120864 = ORIENTED_EDGE ( 'NONE', *, *, #111186, .F. ) ;
#120865 = CIRCLE ( 'NONE', #106208, 0.1000000000000002554 ) ;
#120866 = CIRCLE ( 'NONE', #28948, 0.1000000000000002554 ) ;
#120867 = CARTESIAN_POINT ( 'NONE',  ( 184.5000000000000000, 0.000000000000000000, 7.700000000000000178 ) ) ;
#120868 = EDGE_LOOP ( 'NONE', ( #30925, #86728, #65604, #87259 ) ) ;
#120869 = VECTOR ( 'NONE', #101937, 1000.000000000000000 ) ;
#120870 = DIRECTION ( 'NONE',  ( 0.000000000000000000, 0.000000000000000000, -1.000000000000000000 ) ) ;
#120871 = CARTESIAN_POINT ( 'NONE',  ( -2.100000000000034284, 12.50000000000000000, -2.385244779468109755E-15 ) ) ;
#120872 = VERTEX_POINT ( 'NONE', #44324 ) ;
#120873 = AXIS2_PLACEMENT_3D ( 'NONE', #129041, #117230, #47243 ) ;
#120874 = CONICAL_SURFACE ( 'NONE', #58209, 0.09999999999999982514, 0.003490658503988666988 ) ;
#120875 = ORIENTED_EDGE ( 'NONE', *, *, #53036, .F. ) ;
#120876 = ORIENTED_EDGE ( 'NONE', *, *, #79429, .F. ) ;
#120877 = ORIENTED_EDGE ( 'NONE', *, *, #121081, .T. ) ;
#120878 = DIRECTION ( 'NONE',  ( -0.000000000000000000, 1.000000000000000000, -0.000000000000000000 ) ) ;
#120879 = CARTESIAN_POINT ( 'NONE',  ( 8.512291507278087366, 1.500000000000128120, 9.502944100741384403 ) ) ;
#120880 = DIRECTION ( 'NONE',  ( -0.000000000000000000, -1.000000000000000000, -0.000000000000000000 ) ) ;
#120881 = FACE_BOUND ( 'NONE', #124725, .T. ) ;
#120882 = CARTESIAN_POINT ( 'NONE',  ( -3.749999999999991118, 2.500000000000000000, 2.265063509461097357 ) ) ;
#120883 = CARTESIAN_POINT ( 'NONE',  ( 185.2395833340161175, 4.445597072760117285, 7.699999999999999289 ) ) ;
#120884 = VECTOR ( 'NONE', #24135, 1000.000000000000000 ) ;
#120885 = CARTESIAN_POINT ( 'NONE',  ( -0.6500000000000403233, 12.50000000000000000, 1.818653347947321475 ) ) ;
#120886 = DIRECTION ( 'NONE',  ( -0.000000000000000000, 1.000000000000000000, -0.000000000000000000 ) ) ;
#120887 = CARTESIAN_POINT ( 'NONE',  ( -0.4000000000000392131, 12.50000000000000000, -5.088040615133791356 ) ) ;
#120888 = CARTESIAN_POINT ( 'NONE',  ( 12.49999999999993605, 12.50000000000000000, 0.06509327318403515528 ) ) ;
#120889 = CARTESIAN_POINT ( 'NONE',  ( -8.750000000000010658, 2.500000000000000000, -7.088010851410848190 ) ) ;
#120891 = EDGE_CURVE ( 'NONE', #88147, #123047, #74444, .T. ) ;
#120890 = CIRCLE ( 'NONE', #116686, 0.09999999999999982514 ) ;
#120892 = DIRECTION ( 'NONE',  ( -0.000000000000000000, 1.000000000000000000, -0.000000000000000000 ) ) ;
#120893 = VERTEX_POINT ( 'NONE', #115636 ) ;
#120894 = ORIENTED_EDGE ( 'NONE', *, *, #29899, .T. ) ;
#120895 = ORIENTED_EDGE ( 'NONE', *, *, #113676, .T. ) ;
#120896 = ORIENTED_EDGE ( 'NONE', *, *, #86348, .F. ) ;
#120897 = VERTEX_POINT ( 'NONE', #56702 ) ;
#120898 = AXIS2_PLACEMENT_3D ( 'NONE', #123879, #74803, #95733 ) ;
#120899 = DIRECTION ( 'NONE',  ( 0.000000000000000000, 0.000000000000000000, -1.000000000000000000 ) ) ;
#120900 = EDGE_CURVE ( 'NONE', #79354, #63146, #65242, .T. ) ;
#120901 = DIRECTION ( 'NONE',  ( -4.274815082592931898E-19, -0.9999939076577903929, -0.003490651415223739937 ) ) ;
#120902 = VERTEX_POINT ( 'NONE', #25993 ) ;
#120903 = FACE_BOUND ( 'NONE', #92839, .T. ) ;
#120904 = ADVANCED_FACE ( 'NONE', ( #16133 ), #124184, .T. ) ;
#120905 = LINE ( 'NONE', #81622, #127211 ) ;
#120906 = VECTOR ( 'NONE', #50979, 1000.000000000000000 ) ;
#120907 = COLOUR_RGB ( '', 0.08235294, 0.09019608, 0.10196078) ;
#120908 = EDGE_CURVE ( 'NONE', #81253, #46586, #5037, .T. ) ;
#120909 = EDGE_CURVE ( 'NONE', #64039, #31018, #74997, .T. ) ;
#120910 = VERTEX_POINT ( 'NONE', #24056 ) ;
#120911 = CARTESIAN_POINT ( 'NONE',  ( 6.899999999999926636, 2.500000000000000000, 0.3464101615137736845 ) ) ;
#120912 = DIRECTION ( 'NONE',  ( 0.000000000000000000, -0.000000000000000000, 1.000000000000000000 ) ) ;
#120913 = DIRECTION ( 'NONE',  ( 0.000000000000000000, 0.000000000000000000, -1.000000000000000000 ) ) ;
#120914 = EDGE_CURVE ( 'NONE', #97281, #113533, #91719, .T. ) ;
#120915 = CARTESIAN_POINT ( 'NONE',  ( -8.350000000000013856, 12.50000000000000000, -2.099970236277064473 ) ) ;
#120916 = VERTEX_POINT ( 'NONE', #94080 ) ;
#120917 = CIRCLE ( 'NONE', #125129, 0.06509327318403745899 ) ;
#120918 = DIRECTION ( 'NONE',  ( -4.274815082592931898E-19, -0.9999939076577903929, -0.003490651415223739937 ) ) ;
#120919 = CONICAL_SURFACE ( 'NONE', #5882, 0.1000000000000002554, 0.003490658503988666988 ) ;
#120920 = ORIENTED_EDGE ( 'NONE', *, *, #105832, .F. ) ;
#120921 = ORIENTED_EDGE ( 'NONE', *, *, #19271, .F. ) ;
#120922 = DIRECTION ( 'NONE',  ( 0.000000000000000000, 1.000000000000000000, 0.000000000000000000 ) ) ;
#120923 = DIRECTION ( 'NONE',  ( 0.000000000000000000, 0.000000000000000000, 1.000000000000000000 ) ) ;
#120924 = EDGE_LOOP ( 'NONE', ( #108608, #90714 ) ) ;
#120925 = CARTESIAN_POINT ( 'NONE',  ( -3.100000000000028955, 12.50000000000000000, 3.983716857408420964 ) ) ;
#120926 = FACE_OUTER_BOUND ( 'NONE', #85761, .T. ) ;
#120927 = CARTESIAN_POINT ( 'NONE',  ( -1.250000000000001554, 2.500000000000000000, 6.595190528383296780 ) ) ;
#120928 = DIRECTION ( 'NONE',  ( 1.000000000000000000, 0.000000000000000000, 0.000000000000000000 ) ) ;
#120929 = FACE_OUTER_BOUND ( 'NONE', #92811, .T. ) ;
#120930 = EDGE_LOOP ( 'NONE', ( #62748, #46997 ) ) ;
#120931 = DIRECTION ( 'NONE',  ( 0.000000000000000000, 0.000000000000000000, 1.000000000000000000 ) ) ;
#120932 = EDGE_LOOP ( 'NONE', ( #91072, #111134, #72822, #97203 ) ) ;
#120933 = DIRECTION ( 'NONE',  ( 0.000000000000000000, 0.000000000000000000, 1.000000000000000000 ) ) ;
#120935 = VECTOR ( 'NONE', #75775, 1000.000000000000000 ) ;
#120934 = AXIS2_PLACEMENT_3D ( 'NONE', #115650, #86843, #76394 ) ;
#120936 = ORIENTED_EDGE ( 'NONE', *, *, #70280, .F. ) ;
#120937 = DIRECTION ( 'NONE',  ( 0.000000000000000000, 0.000000000000000000, -1.000000000000000000 ) ) ;
#120938 = ORIENTED_EDGE ( 'NONE', *, *, #50560, .F. ) ;
#120939 = CARTESIAN_POINT ( 'NONE',  ( 12.89999999999990088, 2.500000000000000000, 4.230127018922196669 ) ) ;
#120940 = DIRECTION ( 'NONE',  ( -0.000000000000000000, 1.000000000000000000, -0.000000000000000000 ) ) ;
#120941 = DIRECTION ( 'NONE',  ( 0.000000000000000000, 0.000000000000000000, 1.000000000000000000 ) ) ;
#120942 = CARTESIAN_POINT ( 'NONE',  ( 0.7999999999999553024, 2.500000000000000000, -4.330127018922201643 ) ) ;
#120943 = CARTESIAN_POINT ( 'NONE',  ( 10.44999999999991047, 2.500000000000000000, -6.495190528383302464 ) ) ;
#120944 = ORIENTED_EDGE ( 'NONE', *, *, #84271, .T. ) ;
#120945 = ORIENTED_EDGE ( 'NONE', *, *, #54609, .T. ) ;
#120946 = ORIENTED_EDGE ( 'NONE', *, *, #18417, .F. ) ;
#120947 = CARTESIAN_POINT ( 'NONE',  ( -10.40000000000000391, 2.500000000000000000, -3.737306695894645259 ) ) ;
#120948 = DIRECTION ( 'NONE',  ( 0.000000000000000000, -0.9999939076577903929, 0.003490651415223739937 ) ) ;
#120950 = EDGE_CURVE ( 'NONE', #7073, #78283, #34536, .T. ) ;
#120949 = CARTESIAN_POINT ( 'NONE',  ( 5.649999999999934630, 12.50000000000000000, 6.213873640053559022 ) ) ;
#120953 = EDGE_LOOP ( 'NONE', ( #58902, #22194, #57688, #102283 ) ) ;
#120952 = ORIENTED_EDGE ( 'NONE', *, *, #46214, .F. ) ;
#120951 = CONICAL_SURFACE ( 'NONE', #22681, 0.1000000000000000472, 0.003490658503988666988 ) ;
#120954 = VERTEX_POINT ( 'NONE', #14840 ) ;
#120955 = EDGE_CURVE ( 'NONE', #41978, #115959, #39427, .T. ) ;
#120956 = DIRECTION ( 'NONE',  ( 0.000000000000000000, 1.000000000000000000, 0.000000000000000000 ) ) ;
#120957 = EDGE_CURVE ( 'NONE', #115043, #104608, #96012, .T. ) ;
#120958 = ORIENTED_EDGE ( 'NONE', *, *, #53424, .F. ) ;
#120959 = CARTESIAN_POINT ( 'NONE',  ( -4.293440603042597559E-14, 2.500000000000000000, 5.022947341949748790 ) ) ;
#120960 = CARTESIAN_POINT ( 'NONE',  ( 11.64999999999990798, 2.500000000000000000, -2.757883832488654097 ) ) ;
#120961 = CONTEXT_DEPENDENT_SHAPE_REPRESENTATION ( #117470, #105795 ) ;
#120963 = CARTESIAN_POINT ( 'NONE',  ( -6.900000000000019007, 12.50000000000000000, -0.3464101615137783474 ) ) ;
#120962 = CONICAL_SURFACE ( 'NONE', #79212, 0.1000000000000002554, 0.003490658503988666988 ) ;
#120964 = DIRECTION ( 'NONE',  ( -0.000000000000000000, 1.000000000000000000, -0.000000000000000000 ) ) ;
#120965 = AXIS2_PLACEMENT_3D ( 'NONE', #117713, #98094, #67313 ) ;
#120967 = EDGE_CURVE ( 'NONE', #41467, #69086, #114988, .T. ) ;
#120966 = FACE_OUTER_BOUND ( 'NONE', #79420, .T. ) ;
#120968 = DIRECTION ( 'NONE',  ( 0.000000000000000000, 1.000000000000000000, 0.000000000000000000 ) ) ;
#120969 = FACE_OUTER_BOUND ( 'NONE', #33377, .T. ) ;
#120970 = EDGE_CURVE ( 'NONE', #43475, #62131, #121298, .T. ) ;
#120971 = CARTESIAN_POINT ( 'NONE',  ( -6.650000000000014566, 12.50000000000000000, 1.472243186433545459 ) ) ;
#120972 = CONICAL_SURFACE ( 'NONE', #95845, 0.1000000000000002554, 0.003490658503988666988 ) ;
#120973 = EDGE_LOOP ( 'NONE', ( #117466, #31170, #4935, #66635 ) ) ;
#120975 = EDGE_CURVE ( 'NONE', #124470, #8336, #106472, .T. ) ;
#120974 = AXIS2_PLACEMENT_3D ( 'NONE', #126288, #77182, #97465 ) ;
#120976 = CARTESIAN_POINT ( 'NONE',  ( 9.349999999999916156, 12.50000000000000000, 6.148780366869520009 ) ) ;
#120977 = ADVANCED_FACE ( 'NONE', ( #35804 ), #69773, .T. ) ;
#120978 = CIRCLE ( 'NONE', #64530, 0.06509327318403745899 ) ;
#120979 = FACE_OUTER_BOUND ( 'NONE', #36178, .T. ) ;
#120980 = ORIENTED_EDGE ( 'NONE', *, *, #87571, .F. ) ;
#120981 = ORIENTED_EDGE ( 'NONE', *, *, #65311, .T. ) ;
#120982 = CARTESIAN_POINT ( 'NONE',  ( 187.2135416670080588, 4.367472073101518859, -7.564683531249999149 ) ) ;
#120983 = DIRECTION ( 'NONE',  ( -0.000000000000000000, 1.000000000000000000, -0.000000000000000000 ) ) ;
#120984 = DIRECTION ( 'NONE',  ( -0.000000000000000000, -1.000000000000000000, -0.000000000000000000 ) ) ;
#120985 = ADVANCED_FACE ( 'NONE', ( #78966 ), #88092, .T. ) ;
#120986 = AXIS2_PLACEMENT_3D ( 'NONE', #128647, #78892, #46847 ) ;
#120987 = CARTESIAN_POINT ( 'NONE',  ( -9.550000000000002487, 2.500000000000000000, 6.495190528383297135 ) ) ;
#120988 = CARTESIAN_POINT ( 'NONE',  ( -8.350000000000012079, 12.50000000000000000, -1.537336459617587581 ) ) ;
#120989 = AXIS2_PLACEMENT_3D ( 'NONE', #3951, #110682, #60941 ) ;
#120990 = FACE_OUTER_BOUND ( 'NONE', #111088, .T. ) ;
#120991 = CARTESIAN_POINT ( 'NONE',  ( 9.599999999999914380, 2.500000000000000000, 3.537306695894645081 ) ) ;
#120992 = CARTESIAN_POINT ( 'NONE',  ( 0.6499999999999543920, 12.50000000000000000, 6.906693963081109722 ) ) ;
#120993 = CARTESIAN_POINT ( 'NONE',  ( 12.29999999999990656, 2.500000000000000000, 4.083716857408421497 ) ) ;
#120994 = AXIS2_PLACEMENT_3D ( 'NONE', #109158, #10334, #20803 ) ;
#120995 = ORIENTED_EDGE ( 'NONE', *, *, #2856, .T. ) ;
#120996 = EDGE_LOOP ( 'NONE', ( #14526, #14355 ) ) ;
#120997 = VERTEX_POINT ( 'NONE', #118873 ) ;
#120998 = AXIS2_PLACEMENT_3D ( 'NONE', #125503, #94758, #46963 ) ;
#120999 = ORIENTED_EDGE ( 'NONE', *, *, #122607, .F. ) ;
#121000 = EDGE_LOOP ( 'NONE', ( #90532, #30304 ) ) ;
#121001 = CARTESIAN_POINT ( 'NONE',  ( -3.950000000000026379, 12.50000000000000000, 6.841600689897072485 ) ) ;
#121002 = DIRECTION ( 'NONE',  ( 0.000000000000000000, 1.000000000000000000, 0.000000000000000000 ) ) ;
#121003 = VERTEX_POINT ( 'NONE', #128727 ) ;
#121004 = FACE_OUTER_BOUND ( 'NONE', #119086, .T. ) ;
#121005 = DIRECTION ( 'NONE',  ( 0.000000000000000000, 0.000000000000000000, -1.000000000000000000 ) ) ;
#121006 = CIRCLE ( 'NONE', #8126, 0.06509327318403745899 ) ;
#121007 = DIRECTION ( 'NONE',  ( 0.000000000000000000, 0.000000000000000000, -1.000000000000000000 ) ) ;
#121009 = VERTEX_POINT ( 'NONE', #38403 ) ;
#121008 = CARTESIAN_POINT ( 'NONE',  ( 6.849999999999930367, 2.500000000000000000, -6.248780366869526759 ) ) ;
#121010 = PLANE ( 'NONE',  #43265 ) ;
#121011 = CIRCLE ( 'NONE', #58336, 0.09999999999999982514 ) ;
#121012 = LINE ( 'NONE', #22834, #125172 ) ;
#121013 = ORIENTED_EDGE ( 'NONE', *, *, #30229, .F. ) ;
#121014 = CIRCLE ( 'NONE', #108488, 0.06509327318403745899 ) ;
#121015 = ADVANCED_FACE ( 'NONE', ( #97299 ), #92041, .T. ) ;
#121016 = ORIENTED_EDGE ( 'NONE', *, *, #75700, .T. ) ;
#121017 = EDGE_LOOP ( 'NONE', ( #47908, #76026, #35767, #72120 ) ) ;
#121018 = VERTEX_POINT ( 'NONE', #49509 ) ;
#121019 = CARTESIAN_POINT ( 'NONE',  ( 3.349999999999945466, 2.500000000000000000, -7.188010851410854052 ) ) ;
#121020 = AXIS2_PLACEMENT_3D ( 'NONE', #73604, #115448, #113538 ) ;
#121021 = CARTESIAN_POINT ( 'NONE',  ( 9.149999999999916866, 2.500000000000000000, 5.702370205355745014 ) ) ;
#121022 = CARTESIAN_POINT ( 'NONE',  ( -8.350000000000013856, 2.500000000000000000, 2.265063509461097357 ) ) ;
#121023 = ORIENTED_EDGE ( 'NONE', *, *, #35993, .F. ) ;
#121025 = AXIS2_PLACEMENT_3D ( 'NONE', #122350, #22868, #64060 ) ;
#121024 = CONICAL_SURFACE ( 'NONE', #89634, 0.09999999999999982514, 0.003490658503988666988 ) ;
#121026 = DIRECTION ( 'NONE',  ( -0.000000000000000000, 1.000000000000000000, -0.000000000000000000 ) ) ;
#121027 = VERTEX_POINT ( 'NONE', #107762 ) ;
#121028 = LINE ( 'NONE', #40561, #99698 ) ;
#121030 = CIRCLE ( 'NONE', #29109, 0.06509327318403745899 ) ;
#121029 = CARTESIAN_POINT ( 'NONE',  ( 19.09982477502543219, -0.5559300837585612332, -4.454172625795868257 ) ) ;
#121031 = DIRECTION ( 'NONE',  ( -0.000000000000000000, -1.000000000000000000, -0.000000000000000000 ) ) ;
#121032 = CARTESIAN_POINT ( 'NONE',  ( -2.499999999999996003, 2.500000000000000000, -2.276824562219559311E-15 ) ) ;
#121033 = ORIENTED_EDGE ( 'NONE', *, *, #110001, .T. ) ;
#121035 = CIRCLE ( 'NONE', #75067, 0.1000000000000000472 ) ;
#121034 = CONICAL_SURFACE ( 'NONE', #64594, 0.1000000000000002554, 0.003490658503988666988 ) ;
#121036 = EDGE_LOOP ( 'NONE', ( #107760, #91894, #82491, #52550 ) ) ;
#121037 = VERTEX_POINT ( 'NONE', #29852 ) ;
#121038 = DIRECTION ( 'NONE',  ( -4.274815082592931898E-19, -0.9999939076577903929, -0.003490651415223739937 ) ) ;
#121039 = CARTESIAN_POINT ( 'NONE',  ( 9.799999999999913669, 12.50000000000000000, 4.676537180435972552 ) ) ;
#121040 = FACE_BOUND ( 'NONE', #37431, .T. ) ;
#121041 = CARTESIAN_POINT ( 'NONE',  ( -13.74999999999998934, 2.500000000000000000, 2.757883832488653209 ) ) ;
#121042 = CARTESIAN_POINT ( 'NONE',  ( -7.500000000000015099, 12.50000000000000000, -0.6928203230275541413 ) ) ;
#121043 = CARTESIAN_POINT ( 'NONE',  ( -9.150000000000009237, 2.500000000000000000, -2.857883832488653741 ) ) ;
#121044 = CIRCLE ( 'NONE', #18549, 0.09999999999999982514 ) ;
#121045 = PLANE ( 'NONE',  #40097 ) ;
#121046 = CARTESIAN_POINT ( 'NONE',  ( 184.0416666666666572, -4.445597072760122614, 7.699999999999997513 ) ) ;
#121047 = CARTESIAN_POINT ( 'NONE',  ( -10.40000000000000213, 12.50000000000000000, 5.088040615133786027 ) ) ;
#121048 = ORIENTED_EDGE ( 'NONE', *, *, #71695, .F. ) ;
#121049 = DIRECTION ( 'NONE',  ( 0.000000000000000000, 1.000000000000000000, 0.000000000000000000 ) ) ;
#121050 = AXIS2_PLACEMENT_3D ( 'NONE', #51973, #1559, #119393 ) ;
#121051 = EDGE_CURVE ( 'NONE', #43024, #32323, #58672, .T. ) ;
#121052 = CONICAL_SURFACE ( 'NONE', #18641, 0.1000000000000000472, 0.003490658503988666988 ) ;
#121053 = DIRECTION ( 'NONE',  ( 0.000000000000000000, 0.000000000000000000, -1.000000000000000000 ) ) ;
#121054 = ORIENTED_EDGE ( 'NONE', *, *, #98973, .F. ) ;
#121055 = EDGE_LOOP ( 'NONE', ( #90561, #55276, #13054, #107249 ) ) ;
#121056 = DIRECTION ( 'NONE',  ( 0.000000000000000000, 1.000000000000000000, 0.000000000000000000 ) ) ;
#121057 = EDGE_CURVE ( 'NONE', #62008, #120204, #78325, .T. ) ;
#121058 = CARTESIAN_POINT ( 'NONE',  ( 5.849999999999933031, 2.500000000000000000, 7.088010851410848190 ) ) ;
#121059 = FACE_BOUND ( 'NONE', #128040, .T. ) ;
#121060 = EDGE_CURVE ( 'NONE', #86814, #73847, #77013, .T. ) ;
#121061 = DIRECTION ( 'NONE',  ( 0.000000000000000000, 0.000000000000000000, 1.000000000000000000 ) ) ;
#121062 = CIRCLE ( 'NONE', #75097, 0.06509327318403745899 ) ;
#121063 = AXIS2_PLACEMENT_3D ( 'NONE', #54793, #34549, #83637 ) ;
#121064 = CIRCLE ( 'NONE', #56300, 0.1000000000000002554 ) ;
#121065 = CARTESIAN_POINT ( 'NONE',  ( 97.50000000000000000, 0.000000000000000000, 0.000000000000000000 ) ) ;
#121066 = EDGE_CURVE ( 'NONE', #23803, #86766, #27288, .T. ) ;
#121067 = EDGE_CURVE ( 'NONE', #87887, #11509, #20038, .T. ) ;
#121068 = VERTEX_POINT ( 'NONE', #109031 ) ;
#121069 = DIRECTION ( 'NONE',  ( 0.000000000000000000, 0.000000000000000000, 1.000000000000000000 ) ) ;
#121070 = ADVANCED_FACE ( 'NONE', ( #87463 ), #18879, .T. ) ;
#121071 = EDGE_CURVE ( 'NONE', #84610, #269, #69053, .T. ) ;
#121072 = DIRECTION ( 'NONE',  ( 0.000000000000000000, 0.000000000000000000, -1.000000000000000000 ) ) ;
#121073 = EDGE_CURVE ( 'NONE', #111655, #51736, #81578, .T. ) ;
#121074 = CIRCLE ( 'NONE', #89680, 0.06509327318403741736 ) ;
#121075 = VERTEX_POINT ( 'NONE', #27915 ) ;
#121076 = DIRECTION ( 'NONE',  ( -4.274815082592931898E-19, -0.9999939076577903929, -0.003490651415223739937 ) ) ;
#121077 = DIRECTION ( 'NONE',  ( 0.000000000000000000, 0.000000000000000000, -1.000000000000000000 ) ) ;
#121078 = CIRCLE ( 'NONE', #98086, 0.06509327318403745899 ) ;
#121079 = DIRECTION ( 'NONE',  ( 0.000000000000000000, 0.000000000000000000, 1.000000000000000000 ) ) ;
#121081 = EDGE_CURVE ( 'NONE', #51026, #56576, #41888, .T. ) ;
#121080 = DIRECTION ( 'NONE',  ( -0.000000000000000000, -1.000000000000000000, -0.000000000000000000 ) ) ;
#121082 = EDGE_LOOP ( 'NONE', ( #662, #122687 ) ) ;
#121083 = CARTESIAN_POINT ( 'NONE',  ( 5.649999999999934630, 2.500000000000000000, -1.818653347947325916 ) ) ;
#121084 = CARTESIAN_POINT ( 'NONE',  ( -6.250000000000021316, 2.500000000000000000, -5.802370205355749988 ) ) ;
#121085 = DIRECTION ( 'NONE',  ( -1.000000000000000000, -0.000000000000000000, -0.000000000000000000 ) ) ;
#121086 = CIRCLE ( 'NONE', #93911, 0.06509327318403745899 ) ;
#121087 = EDGE_LOOP ( 'NONE', ( #18125, #31495 ) ) ;
#121088 = EDGE_LOOP ( 'NONE', ( #66178, #39232 ) ) ;
#121089 = CARTESIAN_POINT ( 'NONE',  ( 14.59999999999989484, 2.500000000000000000, -0.6928203230275541413 ) ) ;
#121090 = ORIENTED_EDGE ( 'NONE', *, *, #121541, .T. ) ;
#121091 = DIRECTION ( 'NONE',  ( -0.000000000000000000, -1.000000000000000000, -0.000000000000000000 ) ) ;
#121092 = CARTESIAN_POINT ( 'NONE',  ( -5.400000000000019895, 12.50000000000000000, 3.702399969078682407 ) ) ;
#121093 = DIRECTION ( 'NONE',  ( 0.000000000000000000, 0.000000000000000000, 1.000000000000000000 ) ) ;
#121094 = EDGE_LOOP ( 'NONE', ( #71508, #44573, #114565, #5642 ) ) ;
#121095 = DIRECTION ( 'NONE',  ( 0.000000000000000000, 0.000000000000000000, 1.000000000000000000 ) ) ;
#121096 = CARTESIAN_POINT ( 'NONE',  ( -7.900000000000011013, 2.500000000000000000, 4.430127018922196847 ) ) ;
#121097 = LINE ( 'NONE', #33385, #96690 ) ;
#121098 = CARTESIAN_POINT ( 'NONE',  ( -12.89999999999999147, 12.50000000000000000, -4.330127018922198978 ) ) ;
#121099 = DIRECTION ( 'NONE',  ( 0.000000000000000000, 0.000000000000000000, 1.000000000000000000 ) ) ;
#121100 = AXIS2_PLACEMENT_3D ( 'NONE', #35504, #47901, #75402 ) ;
#121101 = DIRECTION ( 'NONE',  ( 0.000000000000000000, 0.000000000000000000, 1.000000000000000000 ) ) ;
#121102 = ORIENTED_EDGE ( 'NONE', *, *, #75888, .T. ) ;
#121103 = EDGE_LOOP ( 'NONE', ( #51482, #71279, #127883, #3177 ) ) ;
#121104 = CARTESIAN_POINT ( 'NONE',  ( -2.500000000000032419, 12.50000000000000000, -3.637306695894650055 ) ) ;
#121105 = VERTEX_POINT ( 'NONE', #8901 ) ;
#121106 = CARTESIAN_POINT ( 'NONE',  ( 9.799999999999918998, 2.500000000000000000, -0.2464101615137782308 ) ) ;
#121108 = ORIENTED_EDGE ( 'NONE', *, *, #54537, .F. ) ;
#121107 = ORIENTED_EDGE ( 'NONE', *, *, #77988, .F. ) ;
#121109 = VERTEX_POINT ( 'NONE', #99889 ) ;
#121110 = ADVANCED_FACE ( 'NONE', ( #8262 ), #44035, .T. ) ;
#121111 = DIRECTION ( 'NONE',  ( -0.000000000000000000, 1.000000000000000000, -0.000000000000000000 ) ) ;
#121112 = ADVANCED_FACE ( 'NONE', ( #89415 ), #86826, .T. ) ;
#121113 = DIRECTION ( 'NONE',  ( 0.000000000000000000, 1.000000000000000000, 0.000000000000000000 ) ) ;
#121114 = DIRECTION ( 'NONE',  ( 0.000000000000000000, -0.000000000000000000, 1.000000000000000000 ) ) ;
#121115 = EDGE_CURVE ( 'NONE', #109940, #87133, #39843, .T. ) ;
#121117 = CONICAL_SURFACE ( 'NONE', #66728, 0.09999999999999982514, 0.003490658503988666988 ) ;
#121116 = CONICAL_SURFACE ( 'NONE', #106444, 0.1000000000000000472, 0.003490658503988666988 ) ;
#121118 = CARTESIAN_POINT ( 'NONE',  ( 5.599999999999933031, 2.500000000000000000, 0.2464101615137735679 ) ) ;
#121119 = DIRECTION ( 'NONE',  ( 0.000000000000000000, 1.000000000000000000, 0.000000000000000000 ) ) ;
#121120 = CARTESIAN_POINT ( 'NONE',  ( 11.84999999999990372, 12.50000000000000000, 2.576566944158910744 ) ) ;
#121121 = DIRECTION ( 'NONE',  ( 0.000000000000000000, 0.000000000000000000, -1.000000000000000000 ) ) ;
#121122 = DIRECTION ( 'NONE',  ( 0.000000000000000000, 0.000000000000000000, 1.000000000000000000 ) ) ;
#121123 = AXIS2_PLACEMENT_3D ( 'NONE', #5475, #36898, #97735 ) ;
#121124 = EDGE_CURVE ( 'NONE', #14247, #78443, #10211, .T. ) ;
#121125 = FACE_OUTER_BOUND ( 'NONE', #85831, .T. ) ;
#121126 = EDGE_CURVE ( 'NONE', #74881, #66521, #125495, .T. ) ;
#121127 = CIRCLE ( 'NONE', #8247, 9.000000000000001776 ) ;
#121129 = ORIENTED_EDGE ( 'NONE', *, *, #93580, .F. ) ;
#121128 = ADVANCED_FACE ( 'NONE', ( #90041 ), #104569, .T. ) ;
#121130 = EDGE_CURVE ( 'NONE', #94015, #74258, #2159, .T. ) ;
#121131 = DIRECTION ( 'NONE',  ( 0.000000000000000000, 0.000000000000000000, 1.000000000000000000 ) ) ;
#121132 = ORIENTED_EDGE ( 'NONE', *, *, #73542, .F. ) ;
#121133 = ORIENTED_EDGE ( 'NONE', *, *, #97026, .T. ) ;
#121134 = CARTESIAN_POINT ( 'NONE',  ( 10.59999999999991260, 2.500000000000000000, -0.2464101615137783419 ) ) ;
#121135 = CARTESIAN_POINT ( 'NONE',  ( -5.400000000000024336, 2.500000000000000000, -3.637306695894650055 ) ) ;
#121136 = EDGE_CURVE ( 'NONE', #54303, #3400, #89978, .T. ) ;
#121137 = DIRECTION ( 'NONE',  ( 0.000000000000000000, 0.000000000000000000, 1.000000000000000000 ) ) ;
#121138 = CARTESIAN_POINT ( 'NONE',  ( -6.450000000000014388, 2.500000000000000000, 6.148780366869520897 ) ) ;
#121139 = LINE ( 'NONE', #91681, #5117 ) ;
#121141 = CONICAL_SURFACE ( 'NONE', #68818, 0.1000000000000002554, 0.003490658503988666988 ) ;
#121140 = CARTESIAN_POINT ( 'NONE',  ( -7.950000000000009059, 12.50000000000000000, 6.430097255199259010 ) ) ;
#121142 = ORIENTED_EDGE ( 'NONE', *, *, #75131, .T. ) ;
#121143 = ORIENTED_EDGE ( 'NONE', *, *, #72304, .T. ) ;
#121144 = VECTOR ( 'NONE', #71360, 1000.000000000000000 ) ;
#121146 = EDGE_LOOP ( 'NONE', ( #62538, #120772, #4976, #19896 ) ) ;
#121145 = AXIS2_PLACEMENT_3D ( 'NONE', #56104, #113100, #84930 ) ;
#121147 = FACE_OUTER_BOUND ( 'NONE', #66885, .T. ) ;
#121148 = VERTEX_POINT ( 'NONE', #103095 ) ;
#121149 = EDGE_CURVE ( 'NONE', #108367, #28877, #33574, .T. ) ;
#121150 = ORIENTED_EDGE ( 'NONE', *, *, #46756, .F. ) ;
#121152 = VECTOR ( 'NONE', #36822, 1000.000000000000000 ) ;
#121151 = DIRECTION ( 'NONE',  ( 0.000000000000000000, 0.000000000000000000, 1.000000000000000000 ) ) ;
#121153 = FACE_OUTER_BOUND ( 'NONE', #54117, .T. ) ;
#121155 = AXIS2_PLACEMENT_3D ( 'NONE', #105510, #51, #109364 ) ;
#121154 = CIRCLE ( 'NONE', #18747, 0.1000000000000000056 ) ;
#121156 = AXIS2_PLACEMENT_3D ( 'NONE', #76532, #116435, #106621 ) ;
#121157 = CARTESIAN_POINT ( 'NONE',  ( -6.650000000000014566, 2.500000000000000000, 2.165063509461097713 ) ) ;
#121158 = CARTESIAN_POINT ( 'NONE',  ( -9.400000000000007461, 2.500000000000000000, 0.3464101615137735735 ) ) ;
#121159 = DIRECTION ( 'NONE',  ( 0.000000000000000000, 1.000000000000000000, 0.000000000000000000 ) ) ;
#121160 = EDGE_LOOP ( 'NONE', ( #3884, #5172 ) ) ;
#121161 = FACE_OUTER_BOUND ( 'NONE', #84354, .T. ) ;
#121162 = DIRECTION ( 'NONE',  ( -0.000000000000000000, 1.000000000000000000, -0.000000000000000000 ) ) ;
#121163 = FACE_OUTER_BOUND ( 'NONE', #6234, .T. ) ;
#121164 = PLANE ( 'NONE',  #26346 ) ;
#121165 = CIRCLE ( 'NONE', #37555, 0.06509327318403745899 ) ;
#121166 = CARTESIAN_POINT ( 'NONE',  ( -9.999999999999969802, 2.500000000000000000, 0.09999999999999772959 ) ) ;
#121167 = VERTEX_POINT ( 'NONE', #33095 ) ;
#121168 = AXIS2_PLACEMENT_3D ( 'NONE', #88505, #117295, #67570 ) ;
#121169 = EDGE_CURVE ( 'NONE', #89740, #92388, #54382, .T. ) ;
#121170 = ORIENTED_EDGE ( 'NONE', *, *, #46806, .F. ) ;
#121171 = ORIENTED_EDGE ( 'NONE', *, *, #22094, .F. ) ;
#121172 = DIRECTION ( 'NONE',  ( 0.000000000000000000, 0.000000000000000000, 1.000000000000000000 ) ) ;
#121173 = ORIENTED_EDGE ( 'NONE', *, *, #39634, .F. ) ;
#121174 = CIRCLE ( 'NONE', #119122, 0.06509327318403745899 ) ;
#121175 = FACE_OUTER_BOUND ( 'NONE', #71410, .T. ) ;
#121176 = CARTESIAN_POINT ( 'NONE',  ( 2.049999999999950084, 2.500000000000000000, -2.065063509461102065 ) ) ;
#121177 = CIRCLE ( 'NONE', #60567, 0.09999999999999999167 ) ;
#121178 = ORIENTED_EDGE ( 'NONE', *, *, #120757, .F. ) ;
#121179 = DIRECTION ( 'NONE',  ( 0.000000000000000000, 0.000000000000000000, 1.000000000000000000 ) ) ;
#121180 = CARTESIAN_POINT ( 'NONE',  ( -5.400000000000019895, 2.500000000000000000, 4.330127018922196314 ) ) ;
#121181 = EDGE_CURVE ( 'NONE', #80836, #119345, #92633, .T. ) ;
#121182 = DIRECTION ( 'NONE',  ( -4.274815082592931898E-19, -0.9999939076577903929, -0.003490651415223739937 ) ) ;
#121183 = DIRECTION ( 'NONE',  ( -0.000000000000000000, -1.000000000000000000, -0.000000000000000000 ) ) ;
#121184 = DIRECTION ( 'NONE',  ( 0.000000000000000000, 0.000000000000000000, 1.000000000000000000 ) ) ;
#121185 = ORIENTED_EDGE ( 'NONE', *, *, #117516, .T. ) ;
#121186 = ORIENTED_EDGE ( 'NONE', *, *, #125477, .F. ) ;
#121187 = CARTESIAN_POINT ( 'NONE',  ( 26.75236858844773380, 2.962322775928817986, -2.722363799301888765 ) ) ;
#121188 = LINE ( 'NONE', #128459, #51913 ) ;
#121189 = DIRECTION ( 'NONE',  ( 0.000000000000000000, 0.000000000000000000, -1.000000000000000000 ) ) ;
#121190 = DIRECTION ( 'NONE',  ( -0.000000000000000000, -1.000000000000000000, -0.000000000000000000 ) ) ;
#121191 = VERTEX_POINT ( 'NONE', #61902 ) ;
#121192 = VERTEX_POINT ( 'NONE', #22627 ) ;
#121194 = AXIS2_PLACEMENT_3D ( 'NONE', #121587, #50945, #21468 ) ;
#121193 = FACE_OUTER_BOUND ( 'NONE', #43022, .T. ) ;
#121195 = CARTESIAN_POINT ( 'NONE',  ( 9.799999999999917222, 12.50000000000000000, 0.3464101615137735735 ) ) ;
#121196 = DIRECTION ( 'NONE',  ( 0.000000000000000000, 1.000000000000000000, 0.000000000000000000 ) ) ;
#121197 = DIRECTION ( 'NONE',  ( 0.000000000000000000, 1.000000000000000000, 0.000000000000000000 ) ) ;
#121198 = VERTEX_POINT ( 'NONE', #11498 ) ;
#121199 = DIRECTION ( 'NONE',  ( -4.274815082592931898E-19, -0.9999939076577903929, -0.003490651415223739937 ) ) ;
#121200 = EDGE_CURVE ( 'NONE', #31897, #128741, #60669, .T. ) ;
#121202 = CIRCLE ( 'NONE', #81509, 0.1000000000000000472 ) ;
#121201 = CIRCLE ( 'NONE', #20863, 0.06509327318403745899 ) ;
#121203 = LINE ( 'NONE', #71449, #97453 ) ;
#121204 = ORIENTED_EDGE ( 'NONE', *, *, #90935, .F. ) ;
#121205 = CARTESIAN_POINT ( 'NONE',  ( 15.19999999999989093, 12.50000000000000000, 0.2813168883297361700 ) ) ;
#121206 = ORIENTED_EDGE ( 'NONE', *, *, #57557, .F. ) ;
#121207 = CARTESIAN_POINT ( 'NONE',  ( -7.100000000000017408, 2.500000000000000000, -5.122947341949753763 ) ) ;
#121209 = CIRCLE ( 'NONE', #110741, 0.1000000000000002554 ) ;
#121208 = CONICAL_SURFACE ( 'NONE', #62742, 0.09999999999999982514, 0.003490658503988666988 ) ;
#121210 = ORIENTED_EDGE ( 'NONE', *, *, #41468, .F. ) ;
#121211 = ORIENTED_EDGE ( 'NONE', *, *, #81738, .F. ) ;
#121212 = CARTESIAN_POINT ( 'NONE',  ( -9.350000000000008527, 2.500000000000000000, -6.941600689897073018 ) ) ;
#121213 = CARTESIAN_POINT ( 'NONE',  ( 11.74779829714319135, 2.499999999999999556, -7.682567038344338073 ) ) ;
#121214 = EDGE_CURVE ( 'NONE', #72985, #17629, #10822, .T. ) ;
#121215 = ORIENTED_EDGE ( 'NONE', *, *, #59483, .T. ) ;
#121216 = EDGE_CURVE ( 'NONE', #121192, #35232, #82172, .T. ) ;
#121217 = ORIENTED_EDGE ( 'NONE', *, *, #16164, .T. ) ;
#121218 = ADVANCED_FACE ( 'NONE', ( #91342 ), #71114, .T. ) ;
#121219 = EDGE_CURVE ( 'NONE', #108239, #46118, #50780, .T. ) ;
#121220 = FACE_OUTER_BOUND ( 'NONE', #105121, .T. ) ;
#121221 = CARTESIAN_POINT ( 'NONE',  ( -10.60000000000000142, 12.50000000000000000, -0.3464101615137782364 ) ) ;
#121222 = ORIENTED_EDGE ( 'NONE', *, *, #87530, .T. ) ;
#121223 = CARTESIAN_POINT ( 'NONE',  ( 187.2135416670080303, 4.367472073101518859, -7.564683531249999149 ) ) ;
#121224 = CARTESIAN_POINT ( 'NONE',  ( 184.4010416670081156, -4.367472073101520635, 7.564683531249999149 ) ) ;
#121225 = EDGE_CURVE ( 'NONE', #65002, #99984, #62808, .T. ) ;
#121226 = DIRECTION ( 'NONE',  ( 0.000000000000000000, 0.000000000000000000, -1.000000000000000000 ) ) ;
#121227 = DIRECTION ( 'NONE',  ( 0.000000000000000000, 0.000000000000000000, -1.000000000000000000 ) ) ;
#121228 = DIRECTION ( 'NONE',  ( 0.000000000000000000, 0.000000000000000000, 1.000000000000000000 ) ) ;
#121229 = DIRECTION ( 'NONE',  ( 0.000000000000000000, -0.000000000000000000, 1.000000000000000000 ) ) ;
#121230 = CARTESIAN_POINT ( 'NONE',  ( -12.94999999999999218, 2.500000000000000000, 2.165063509461101265 ) ) ;
#121231 = ADVANCED_FACE ( 'NONE', ( #12763 ), #111635, .T. ) ;
#121232 = EDGE_CURVE ( 'NONE', #54565, #9756, #100, .T. ) ;
#121233 = VECTOR ( 'NONE', #110024, 1000.000000000000000 ) ;
#121234 = EDGE_CURVE ( 'NONE', #60541, #20895, #122105, .T. ) ;
#121235 = CIRCLE ( 'NONE', #25092, 0.09999999999999982514 ) ;
#121236 = ORIENTED_EDGE ( 'NONE', *, *, #30447, .T. ) ;
#121237 = EDGE_LOOP ( 'NONE', ( #54668, #125071, #122683, #117209 ) ) ;
#121238 = DIRECTION ( 'NONE',  ( 0.000000000000000000, 1.000000000000000000, 0.000000000000000000 ) ) ;
#121239 = ORIENTED_EDGE ( 'NONE', *, *, #8764, .T. ) ;
#121240 = DIRECTION ( 'NONE',  ( -4.274815082592931898E-19, -0.9999939076577903929, -0.003490651415223739937 ) ) ;
#121241 = DIRECTION ( 'NONE',  ( 0.000000000000000000, -0.000000000000000000, 1.000000000000000000 ) ) ;
#121242 = DIRECTION ( 'NONE',  ( 0.000000000000000000, 1.000000000000000000, 0.000000000000000000 ) ) ;
#121244 = ORIENTED_EDGE ( 'NONE', *, *, #124648, .F. ) ;
#121243 = ORIENTED_EDGE ( 'NONE', *, *, #17420, .F. ) ;
#121245 = PRODUCT_RELATED_PRODUCT_CATEGORY ( 'part', '', ( #52397 ) ) ;
#121246 = FACE_BOUND ( 'NONE', #55573, .T. ) ;
#121247 = EDGE_LOOP ( 'NONE', ( #53118, #108105, #70558, #117803 ) ) ;
#121248 = ADVANCED_FACE ( 'NONE', ( #63172 ), #101817, .T. ) ;
#121249 = DIRECTION ( 'NONE',  ( -0.000000000000000000, -1.000000000000000000, -0.000000000000000000 ) ) ;
#121250 = DIRECTION ( 'NONE',  ( 0.000000000000000000, 1.000000000000000000, 0.000000000000000000 ) ) ;
#121251 = VECTOR ( 'NONE', #115357, 1000.000000000000000 ) ;
#121252 = CARTESIAN_POINT ( 'NONE',  ( 0.6499999999999561684, 12.50000000000000000, 1.753560074763284016 ) ) ;
#121253 = CARTESIAN_POINT ( 'NONE',  ( 9.999999999999948486, 12.50000000000000000, 4.265033745738159077 ) ) ;
#121254 = CARTESIAN_POINT ( 'NONE',  ( 3.349999999999941913, 12.50000000000000000, 5.737276932171707422 ) ) ;
#121255 = DIRECTION ( 'NONE',  ( 0.000000000000000000, -0.000000000000000000, 1.000000000000000000 ) ) ;
#121256 = FACE_OUTER_BOUND ( 'NONE', #124029, .T. ) ;
#121257 = CARTESIAN_POINT ( 'NONE',  ( -1.250000000000001110, 2.500000000000000000, -6.595190528383302109 ) ) ;
#121258 = FACE_OUTER_BOUND ( 'NONE', #47949, .T. ) ;
#121259 = CARTESIAN_POINT ( 'NONE',  ( 4.999999999999935163, 2.500000000000000000, 3.737306695894644371 ) ) ;
#121260 = AXIS2_PLACEMENT_3D ( 'NONE', #30614, #101914, #72459 ) ;
#121261 = CARTESIAN_POINT ( 'NONE',  ( 10.19999999999991225, 2.500000000000000000, -4.676537180435978769 ) ) ;
#121262 = AXIS2_PLACEMENT_3D ( 'NONE', #25702, #57760, #125828 ) ;
#121263 = ORIENTED_EDGE ( 'NONE', *, *, #3955, .F. ) ;
#121264 = EDGE_LOOP ( 'NONE', ( #123502, #112744, #75210, #61951 ) ) ;
#121265 = ORIENTED_EDGE ( 'NONE', *, *, #60418, .T. ) ;
#121266 = ORIENTED_EDGE ( 'NONE', *, *, #18339, .T. ) ;
#121267 = DIRECTION ( 'NONE',  ( 0.000000000000000000, 0.000000000000000000, -1.000000000000000000 ) ) ;
#121268 = CARTESIAN_POINT ( 'NONE',  ( 8.549999999999922551, 12.50000000000000000, 2.446380397790835826 ) ) ;
#121270 = ORIENTED_EDGE ( 'NONE', *, *, #84749, .F. ) ;
#121269 = ORIENTED_EDGE ( 'NONE', *, *, #78188, .T. ) ;
#121271 = EDGE_LOOP ( 'NONE', ( #84807, #120112 ) ) ;
#121272 = DIRECTION ( 'NONE',  ( 0.000000000000000000, 1.846105847067148022E-16, -1.000000000000000000 ) ) ;
#121273 = CIRCLE ( 'NONE', #4172, 0.5000000000000000000 ) ;
#121274 = CARTESIAN_POINT ( 'NONE',  ( 2.299999999999949640, 2.500000000000000000, -4.676537180435977881 ) ) ;
#121275 = CARTESIAN_POINT ( 'NONE',  ( -1.450000000000036371, 12.50000000000000000, 6.841600689897072485 ) ) ;
#121276 = DIRECTION ( 'NONE',  ( 0.000000000000000000, -0.000000000000000000, 1.000000000000000000 ) ) ;
#121277 = DIRECTION ( 'NONE',  ( 0.000000000000000000, 0.000000000000000000, -1.000000000000000000 ) ) ;
#121278 = CIRCLE ( 'NONE', #6319, 0.1000000000000002554 ) ;
#121279 = CARTESIAN_POINT ( 'NONE',  ( 8.349999999999923261, 12.50000000000000000, -6.430097255199264339 ) ) ;
#121280 = DIRECTION ( 'NONE',  ( -0.000000000000000000, 1.000000000000000000, -0.000000000000000000 ) ) ;
#121281 = VERTEX_POINT ( 'NONE', #93925 ) ;
#121282 = CARTESIAN_POINT ( 'NONE',  ( 3.149999999999946176, 2.500000000000000000, -6.841600689897077814 ) ) ;
#121283 = ORIENTED_EDGE ( 'NONE', *, *, #127164, .F. ) ;
#121284 = EDGE_CURVE ( 'NONE', #72341, #86064, #37679, .T. ) ;
#121285 = ORIENTED_EDGE ( 'NONE', *, *, #45549, .T. ) ;
#121286 = ORIENTED_EDGE ( 'NONE', *, *, #42776, .T. ) ;
#121287 = EDGE_CURVE ( 'NONE', #83886, #89736, #87827, .T. ) ;
#121288 = DIRECTION ( 'NONE',  ( 0.000000000000000000, 0.000000000000000000, 1.000000000000000000 ) ) ;
#121289 =( BOUNDED_CURVE ( )  B_SPLINE_CURVE ( 2, ( #17032, #39950, #119786, #106732, #7236, #47191, #123018 ),
 .UNSPECIFIED., .F., .F. ) 
 B_SPLINE_CURVE_WITH_KNOTS ( ( 3, 2, 2, 3 ),
 ( 0.4285714285714289362, 0.4523809523809527722, 0.4761904761904766081, 0.5000000000000004441 ),
 .UNSPECIFIED. ) 
 CURVE ( )  GEOMETRIC_REPRESENTATION_ITEM ( )  RATIONAL_B_SPLINE_CURVE ( ( 0.9999999999999977796, 0.8660254037844409281, 1.000000000000000000, 0.8660254037844387076, 1.000000000000000000, 0.8660254037844361541, 1.000000000000002442 ) ) 
 REPRESENTATION_ITEM ( '' )  );
#121290 = EDGE_LOOP ( 'NONE', ( #46623, #3313, #10960, #52694 ) ) ;
#121291 = ORIENTED_EDGE ( 'NONE', *, *, #52438, .T. ) ;
#121292 = ORIENTED_EDGE ( 'NONE', *, *, #67109, .F. ) ;
#121293 = DIRECTION ( 'NONE',  ( -1.000000000000000000, -0.000000000000000000, -0.000000000000000000 ) ) ;
#121294 = EDGE_CURVE ( 'NONE', #95328, #97364, #36310, .T. ) ;
#121295 = FACE_OUTER_BOUND ( 'NONE', #87082, .T. ) ;
#121296 = FACE_OUTER_BOUND ( 'NONE', #53861, .T. ) ;
#121297 = DIRECTION ( 'NONE',  ( 0.000000000000000000, 1.000000000000000000, 0.000000000000000000 ) ) ;
#121298 = CIRCLE ( 'NONE', #25143, 0.06509327318403745899 ) ;
#121299 = DIRECTION ( 'NONE',  ( -0.000000000000000000, 1.000000000000000000, -0.000000000000000000 ) ) ;
#121300 = AXIS2_PLACEMENT_3D ( 'NONE', #16773, #5034, #105177 ) ;
#121301 = CARTESIAN_POINT ( 'NONE',  ( 187.0312500006828031, 9.429780353434619030E-16, -7.700000000000000178 ) ) ;
#121302 = VERTEX_POINT ( 'NONE', #113562 ) ;
#121303 = DIRECTION ( 'NONE',  ( 0.000000000000000000, 1.000000000000000000, 0.000000000000000000 ) ) ;
#121305 = VECTOR ( 'NONE', #79528, 1000.000000000000000 ) ;
#121304 = AXIS2_PLACEMENT_3D ( 'NONE', #32345, #50665, #9457 ) ;
#121306 = ORIENTED_EDGE ( 'NONE', *, *, #60052, .F. ) ;
#121307 = CARTESIAN_POINT ( 'NONE',  ( 6.249999999999965361, 2.500000000000000000, 2.165063509461097713 ) ) ;
#121308 = ORIENTED_EDGE ( 'NONE', *, *, #29001, .T. ) ;
#121309 = DIRECTION ( 'NONE',  ( 0.000000000000000000, 0.000000000000000000, 1.000000000000000000 ) ) ;
#121310 = EDGE_LOOP ( 'NONE', ( #57510, #32407 ) ) ;
#121311 = DIRECTION ( 'NONE',  ( -0.000000000000000000, -1.000000000000000000, -0.000000000000000000 ) ) ;
#121312 = DIRECTION ( 'NONE',  ( 0.000000000000000000, 0.000000000000000000, 1.000000000000000000 ) ) ;
#121313 = ORIENTED_EDGE ( 'NONE', *, *, #102573, .F. ) ;
#121314 = ORIENTED_EDGE ( 'NONE', *, *, #47287, .T. ) ;
#121315 = CARTESIAN_POINT ( 'NONE',  ( -1.322875655532295136, -1.500000000000000222, -5.000000000000004441 ) ) ;
#121316 = DIRECTION ( 'NONE',  ( -0.000000000000000000, -1.000000000000000000, -0.000000000000000000 ) ) ;
#121317 = CARTESIAN_POINT ( 'NONE',  ( 184.0885416670080872, -6.551208109652273848, -3.782341765625003571 ) ) ;
#121318 = DIRECTION ( 'NONE',  ( 0.000000000000000000, 0.000000000000000000, 1.000000000000000000 ) ) ;
#121319 = DIRECTION ( 'NONE',  ( 0.000000000000000000, 0.000000000000000000, -1.000000000000000000 ) ) ;
#121320 = ORIENTED_EDGE ( 'NONE', *, *, #43037, .F. ) ;
#121321 = LINE ( 'NONE', #905, #23652 ) ;
#121322 = ORIENTED_EDGE ( 'NONE', *, *, #100279, .T. ) ;
#121323 = DIRECTION ( 'NONE',  ( -0.000000000000000000, -1.000000000000000000, -0.000000000000000000 ) ) ;
#121324 = AXIS2_PLACEMENT_3D ( 'NONE', #3283, #83146, #33406 ) ;
#121325 = DIRECTION ( 'NONE',  ( -4.274815082592931898E-19, -0.9999939076577903929, -0.003490651415223739937 ) ) ;
#121326 = VECTOR ( 'NONE', #62064, 1000.000000000000000 ) ;
#121327 = EDGE_CURVE ( 'NONE', #58914, #8254, #24538, .T. ) ;
#121328 = CARTESIAN_POINT ( 'NONE',  ( 11.44999999999990514, 2.500000000000000000, 2.511473670974873507 ) ) ;
#121329 = DIRECTION ( 'NONE',  ( 0.000000000000000000, 1.000000000000000000, 0.000000000000000000 ) ) ;
#121330 = DIRECTION ( 'NONE',  ( 0.000000000000000000, 0.000000000000000000, 1.000000000000000000 ) ) ;
#121331 = EDGE_CURVE ( 'NONE', #49253, #37140, #102593, .T. ) ;
#121332 = DIRECTION ( 'NONE',  ( 0.000000000000000000, 0.000000000000000000, 1.000000000000000000 ) ) ;
#121333 = CARTESIAN_POINT ( 'NONE',  ( 10.39999999999991154, 2.500000000000000000, 3.637306695894644726 ) ) ;
#121334 = ORIENTED_EDGE ( 'NONE', *, *, #109256, .T. ) ;
#121335 = VECTOR ( 'NONE', #73690, 1000.000000000000000 ) ;
#121336 = CARTESIAN_POINT ( 'NONE',  ( -12.69999999999999041, 12.50000000000000000, 3.983716857408420964 ) ) ;
#121337 = DIRECTION ( 'NONE',  ( 0.000000000000000000, 1.000000000000000000, 0.000000000000000000 ) ) ;
#121338 = FACE_OUTER_BOUND ( 'NONE', #110915, .T. ) ;
#121339 = EDGE_CURVE ( 'NONE', #29412, #115297, #43552, .T. ) ;
#121340 = ORIENTED_EDGE ( 'NONE', *, *, #66828, .T. ) ;
#121341 = DIRECTION ( 'NONE',  ( 0.000000000000000000, -0.9999939076577903929, 0.003490651415223739937 ) ) ;
#121342 = AXIS2_PLACEMENT_3D ( 'NONE', #9934, #11212, #88482 ) ;
#121343 = CIRCLE ( 'NONE', #123400, 0.09999999999999982514 ) ;
#121344 = EDGE_LOOP ( 'NONE', ( #26464, #89232, #56227, #42009 ) ) ;
#121345 = ORIENTED_EDGE ( 'NONE', *, *, #81076, .F. ) ;
#121346 = DIRECTION ( 'NONE',  ( -0.000000000000000000, -1.000000000000000000, -0.000000000000000000 ) ) ;
#121347 = ORIENTED_EDGE ( 'NONE', *, *, #82711, .F. ) ;
#121348 = CARTESIAN_POINT ( 'NONE',  ( 16.86689433361074819, -2.548103353434854057, -5.776876940651522574 ) ) ;
#121349 = DIRECTION ( 'NONE',  ( -0.000000000000000000, 1.000000000000000000, -0.000000000000000000 ) ) ;
#121350 = AXIS2_PLACEMENT_3D ( 'NONE', #15734, #5903, #45863 ) ;
#121351 = ORIENTED_EDGE ( 'NONE', *, *, #124185, .T. ) ;
#121352 = DIRECTION ( 'NONE',  ( -0.000000000000000000, -1.000000000000000000, -0.000000000000000000 ) ) ;
#121353 = EDGE_CURVE ( 'NONE', #64176, #52063, #23906, .T. ) ;
#121354 = CARTESIAN_POINT ( 'NONE',  ( 4.199999999999941558, 12.50000000000000000, -4.330127018922201643 ) ) ;
#121355 = AXIS2_PLACEMENT_3D ( 'NONE', #29789, #18675, #28506 ) ;
#121356 = VERTEX_POINT ( 'NONE', #123377 ) ;
#121357 = EDGE_CURVE ( 'NONE', #66637, #69877, #23172, .T. ) ;
#121358 = ORIENTED_EDGE ( 'NONE', *, *, #59790, .T. ) ;
#121359 = VERTEX_POINT ( 'NONE', #55925 ) ;
#121360 = CARTESIAN_POINT ( 'NONE',  ( -1.050000000000037792, 12.50000000000000000, 6.083687093685482772 ) ) ;
#121361 = CARTESIAN_POINT ( 'NONE',  ( -2.499999999999996447, 2.500000000000000000, 4.230127018922196669 ) ) ;
#121362 = DIRECTION ( 'NONE',  ( 0.000000000000000000, 0.000000000000000000, -1.000000000000000000 ) ) ;
#121363 = ADVANCED_FACE ( 'NONE', ( #84748 ), #94556, .T. ) ;
#121364 = ADVANCED_FACE ( 'NONE', ( #95860 ), #37765, .T. ) ;
#121365 = FACE_BOUND ( 'NONE', #9994, .T. ) ;
#121366 = ORIENTED_EDGE ( 'NONE', *, *, #54007, .T. ) ;
#121367 = EDGE_CURVE ( 'NONE', #113231, #118968, #14050, .T. ) ;
#121368 = EDGE_CURVE ( 'NONE', #128991, #38337, #45485, .T. ) ;
#121369 = CARTESIAN_POINT ( 'NONE',  ( -0.4000000000000401013, 2.500000000000000000, -3.737306695894649700 ) ) ;
#121370 = DIRECTION ( 'NONE',  ( 0.000000000000000000, -0.9999939076577903929, 0.003490651415223739937 ) ) ;
#121371 = ORIENTED_EDGE ( 'NONE', *, *, #51526, .F. ) ;
#121372 = DIRECTION ( 'NONE',  ( -0.000000000000000000, 1.000000000000000000, -0.000000000000000000 ) ) ;
#121373 = DIRECTION ( 'NONE',  ( 0.000000000000000000, 0.000000000000000000, 1.000000000000000000 ) ) ;
#121374 = EDGE_CURVE ( 'NONE', #65870, #10740, #183, .T. ) ;
#121376 = CARTESIAN_POINT ( 'NONE',  ( -12.69999999999999218, 12.50000000000000000, -0.3464101615137741286 ) ) ;
#121375 = AXIS2_PLACEMENT_3D ( 'NONE', #73624, #64454, #103748 ) ;
#121377 = CARTESIAN_POINT ( 'NONE',  ( -9.200000000000006395, 12.50000000000000000, 0.06509327318403504425 ) ) ;
#121378 = CARTESIAN_POINT ( 'NONE',  ( -9.150000000000009237, 2.500000000000000000, 2.065063509461097624 ) ) ;
#121379 = AXIS2_PLACEMENT_3D ( 'NONE', #1522, #40838, #111479 ) ;
#121380 = EDGE_CURVE ( 'NONE', #91731, #118811, #67063, .T. ) ;
#121381 = DIRECTION ( 'NONE',  ( 0.000000000000000000, 1.000000000000000000, 0.000000000000000000 ) ) ;
#121382 = DIRECTION ( 'NONE',  ( -0.000000000000000000, 1.000000000000000000, -0.000000000000000000 ) ) ;
#121383 = EDGE_CURVE ( 'NONE', #127901, #91908, #39923, .T. ) ;
#121385 = EDGE_CURVE ( 'NONE', #59408, #125792, #106795, .T. ) ;
#121384 = CIRCLE ( 'NONE', #8502, 0.06509327318403745899 ) ;
#121386 = EDGE_LOOP ( 'NONE', ( #19212, #32568 ) ) ;
#121387 = ORIENTED_EDGE ( 'NONE', *, *, #80130, .F. ) ;
#121388 = ORIENTED_EDGE ( 'NONE', *, *, #45686, .T. ) ;
#121389 = ORIENTED_EDGE ( 'NONE', *, *, #105596, .F. ) ;
#121390 = CARTESIAN_POINT ( 'NONE',  ( -0.6500000000000398792, 12.50000000000000000, -2.576566944158915184 ) ) ;
#121391 = AXIS2_PLACEMENT_3D ( 'NONE', #20671, #60608, #21972 ) ;
#121392 = CARTESIAN_POINT ( 'NONE',  ( -1.900000000000034994, 12.50000000000000000, -4.611443907251940644 ) ) ;
#121393 = VERTEX_POINT ( 'NONE', #25828 ) ;
#121394 = ADVANCED_FACE ( 'NONE', ( #6167 ), #15338, .T. ) ;
#121395 = FACE_BOUND ( 'NONE', #114015, .T. ) ;
#121396 = ADVANCED_FACE ( 'NONE', ( #35651 ), #75558, .T. ) ;
#121397 = CARTESIAN_POINT ( 'NONE',  ( 13.74999999999993072, 2.500000000000000000, -2.065063509461102065 ) ) ;
#121398 = DIRECTION ( 'NONE',  ( 0.000000000000000000, 0.000000000000000000, 1.000000000000000000 ) ) ;
#121399 = CARTESIAN_POINT ( 'NONE',  ( 4.999999999999935163, 12.50000000000000000, 3.637306695894644726 ) ) ;
#121400 = LINE ( 'NONE', #42212, #113959 ) ;
#121401 = DIRECTION ( 'NONE',  ( 0.000000000000000000, 1.000000000000000000, 0.000000000000000000 ) ) ;
#121402 = DIRECTION ( 'NONE',  ( 0.000000000000000000, 0.000000000000000000, 1.000000000000000000 ) ) ;
#121403 = DIRECTION ( 'NONE',  ( 0.000000000000000000, 0.000000000000000000, -1.000000000000000000 ) ) ;
#121404 = DIRECTION ( 'NONE',  ( -4.274815082592931898E-19, -0.9999939076577903929, -0.003490651415223739937 ) ) ;
#121405 = CARTESIAN_POINT ( 'NONE',  ( -5.000000000000026645, 12.50000000000000000, -3.637306695894650055 ) ) ;
#121406 = ORIENTED_EDGE ( 'NONE', *, *, #76448, .T. ) ;
#121407 = ORIENTED_EDGE ( 'NONE', *, *, #90834, .T. ) ;
#121408 = VERTEX_POINT ( 'NONE', #80577 ) ;
#121409 = ORIENTED_EDGE ( 'NONE', *, *, #39213, .F. ) ;
#121410 = ORIENTED_EDGE ( 'NONE', *, *, #24004, .F. ) ;
#121411 = EDGE_LOOP ( 'NONE', ( #123722, #104802, #99937, #88787 ) ) ;
#121412 = DIRECTION ( 'NONE',  ( -0.000000000000000000, -1.000000000000000000, -0.000000000000000000 ) ) ;
#121413 = EDGE_LOOP ( 'NONE', ( #34793, #69212, #76669, #27593, #47937, #100075, #109586, #73548, #49194, #75825, #106386, #22270, #29491, #10414, #119553, #33284, #11594 ) ) ;
#121414 = CONICAL_SURFACE ( 'NONE', #48259, 0.1000000000000002554, 0.003490658503988666988 ) ;
#121415 = AXIS2_PLACEMENT_3D ( 'NONE', #36477, #107769, #85549 ) ;
#121416 = LINE ( 'NONE', #10792, #72859 ) ;
#121417 = CARTESIAN_POINT ( 'NONE',  ( 15.50668944026786278, -2.500000000000065281, 6.997696164093700766 ) ) ;
#121418 = CARTESIAN_POINT ( 'NONE',  ( -7.500000000000001776, 2.500000000000000000, 1.734723475976807094E-15 ) ) ;
#121419 = DIRECTION ( 'NONE',  ( -0.000000000000000000, 1.000000000000000000, -0.000000000000000000 ) ) ;
#121420 = ORIENTED_EDGE ( 'NONE', *, *, #56452, .F. ) ;
#121421 = DIRECTION ( 'NONE',  ( 0.000000000000000000, 1.000000000000000000, 0.000000000000000000 ) ) ;
#121422 = VECTOR ( 'NONE', #24917, 1000.000000000000000 ) ;
#121423 = ORIENTED_EDGE ( 'NONE', *, *, #17549, .T. ) ;
#121424 = EDGE_CURVE ( 'NONE', #15508, #23590, #4371, .T. ) ;
#121425 = EDGE_LOOP ( 'NONE', ( #52923, #86577 ) ) ;
#121426 = FACE_OUTER_BOUND ( 'NONE', #48078, .T. ) ;
#121427 = EDGE_CURVE ( 'NONE', #125357, #23344, #38740, .T. ) ;
#121428 = LINE ( 'NONE', #1018, #40646 ) ;
#121429 = DIRECTION ( 'NONE',  ( 0.000000000000000000, 1.000000000000000000, 0.000000000000000000 ) ) ;
#121430 = EDGE_LOOP ( 'NONE', ( #126290, #47206, #52682, #107585 ) ) ;
#121431 = ORIENTED_EDGE ( 'NONE', *, *, #10919, .T. ) ;
#121432 = CIRCLE ( 'NONE', #81721, 0.06509327318403745899 ) ;
#121433 = DIRECTION ( 'NONE',  ( 0.000000000000000000, 0.000000000000000000, -1.000000000000000000 ) ) ;
#121434 = CONICAL_SURFACE ( 'NONE', #8552, 0.1000000000000002554, 0.003490658503988666988 ) ;
#121435 = DIRECTION ( 'NONE',  ( 0.000000000000000000, 0.000000000000000000, -1.000000000000000000 ) ) ;
#121436 = CARTESIAN_POINT ( 'NONE',  ( 10.39999999999991154, 2.500000000000000000, -3.637306695894650055 ) ) ;
#121437 = CARTESIAN_POINT ( 'NONE',  ( -9.999999999999969802, 2.500000000000000000, -2.276824562219559311E-15 ) ) ;
#121438 = VERTEX_POINT ( 'NONE', #40011 ) ;
#121439 = CARTESIAN_POINT ( 'NONE',  ( -10.45000000000000107, 12.50000000000000000, 2.165063509461097713 ) ) ;
#121440 = AXIS2_PLACEMENT_3D ( 'NONE', #19457, #30593, #78404 ) ;
#121441 = ORIENTED_EDGE ( 'NONE', *, *, #101552, .F. ) ;
#121442 = CARTESIAN_POINT ( 'NONE',  ( 13.39053294304968134, -2.500000000000001332, 7.037281287790809081 ) ) ;
#121443 = EDGE_LOOP ( 'NONE', ( #89081, #108368, #96998, #8223 ) ) ;
#121444 = CARTESIAN_POINT ( 'NONE',  ( 17.50000000000000000, 2.499999999999999556, 2.333333333333335702 ) ) ;
#121445 = CARTESIAN_POINT ( 'NONE',  ( 26.74601956401501468, -2.978655701349517848, 2.722801865438416069 ) ) ;
#121446 = CONICAL_SURFACE ( 'NONE', #119385, 0.1000000000000000472, 0.003490658503988666988 ) ;
#121447 = LINE ( 'NONE', #52085, #107536 ) ;
#121448 = CARTESIAN_POINT ( 'NONE',  ( 0.5999999999999551248, 2.500000000000000000, -4.676537180435978769 ) ) ;
#121449 = CARTESIAN_POINT ( 'NONE',  ( -13.34999999999999076, 12.50000000000000000, -2.165063509461099489 ) ) ;
#121450 = EDGE_LOOP ( 'NONE', ( #53571, #2792 ) ) ;
#121451 = LINE ( 'NONE', #11510, #30058 ) ;
#121452 = DIRECTION ( 'NONE',  ( 0.000000000000000000, 1.000000000000000000, 0.000000000000000000 ) ) ;
#121453 = VERTEX_POINT ( 'NONE', #79921 ) ;
#121454 = ORIENTED_EDGE ( 'NONE', *, *, #115411, .T. ) ;
#121455 = EDGE_LOOP ( 'NONE', ( #39024, #32887 ) ) ;
#121456 = CARTESIAN_POINT ( 'NONE',  ( 2.500000000000002220, 2.750000000000000000, 10.00000000000000178 ) ) ;
#121457 = FACE_OUTER_BOUND ( 'NONE', #74745, .T. ) ;
#121458 = CARTESIAN_POINT ( 'NONE',  ( 187.2343750003414016, 8.734944146203032389, 5.348610694689227483E-16 ) ) ;
#121459 = DIRECTION ( 'NONE',  ( 0.000000000000000000, 0.000000000000000000, 1.000000000000000000 ) ) ;
#121460 = DIRECTION ( 'NONE',  ( 0.000000000000000000, 1.000000000000000000, 0.000000000000000000 ) ) ;
#121461 = ADVANCED_FACE ( 'NONE', ( #9252 ), #21034, .T. ) ;
#121462 = DIRECTION ( 'NONE',  ( 0.000000000000000000, 0.000000000000000000, 1.000000000000000000 ) ) ;
#121463 = CARTESIAN_POINT ( 'NONE',  ( 11.64999999999990266, 12.50000000000000000, -6.495190528383302464 ) ) ;
#121464 = CARTESIAN_POINT ( 'NONE',  ( 187.5000000000000000, 0.000000000000000000, 0.000000000000000000 ) ) ;
#121465 = CIRCLE ( 'NONE', #12792, 0.1000000000000000472 ) ;
#121466 = AXIS2_PLACEMENT_3D ( 'NONE', #6025, #45981, #106185 ) ;
#121467 = AXIS2_PLACEMENT_3D ( 'NONE', #84744, #105012, #124679 ) ;
#121468 = VECTOR ( 'NONE', #55658, 1000.000000000000000 ) ;
#121469 = EDGE_LOOP ( 'NONE', ( #53312, #48464 ) ) ;
#121470 = DIRECTION ( 'NONE',  ( -0.000000000000000000, -1.000000000000000000, -0.000000000000000000 ) ) ;
#121472 = EDGE_CURVE ( 'NONE', #103811, #124333, #4278, .T. ) ;
#121471 = AXIS2_PLACEMENT_3D ( 'NONE', #127882, #78153, #48686 ) ;
#121474 = EDGE_CURVE ( 'NONE', #81857, #124173, #59000, .T. ) ;
#121473 = DIRECTION ( 'NONE',  ( -0.000000000000000000, 1.000000000000000000, -0.000000000000000000 ) ) ;
#121475 = DIRECTION ( 'NONE',  ( -0.000000000000000000, -1.000000000000000000, -0.000000000000000000 ) ) ;
#121476 = CARTESIAN_POINT ( 'NONE',  ( 17.50000000000000000, -2.500000000000000000, 0.000000000000000000 ) ) ;
#121477 = VERTEX_POINT ( 'NONE', #60307 ) ;
#121478 = DIRECTION ( 'NONE',  ( -0.000000000000000000, 1.000000000000000000, -0.000000000000000000 ) ) ;
#121479 = DIRECTION ( 'NONE',  ( 0.000000000000000000, 1.000000000000000000, 0.000000000000000000 ) ) ;
#121481 = VERTEX_POINT ( 'NONE', #28900 ) ;
#121480 = CARTESIAN_POINT ( 'NONE',  ( 6.899999999999928413, 2.500000000000000000, 4.576537180435972019 ) ) ;
#121482 = EDGE_CURVE ( 'NONE', #64399, #33567, #100831, .T. ) ;
#121483 = ORIENTED_EDGE ( 'NONE', *, *, #816, .T. ) ;
#121484 = DIRECTION ( 'NONE',  ( 0.000000000000000000, -0.9999939076577903929, 0.003490651415223739937 ) ) ;
#121485 = ORIENTED_EDGE ( 'NONE', *, *, #104526, .F. ) ;
#121486 = VERTEX_POINT ( 'NONE', #18423 ) ;
#121487 = DIRECTION ( 'NONE',  ( 0.000000000000000000, 0.000000000000000000, 1.000000000000000000 ) ) ;
#121488 = DIRECTION ( 'NONE',  ( -0.000000000000000000, 1.000000000000000000, -0.000000000000000000 ) ) ;
#121489 = LINE ( 'NONE', #22684, #69384 ) ;
#121490 = CARTESIAN_POINT ( 'NONE',  ( -7.900000000000014566, 2.500000000000000000, -0.5928203230275541635 ) ) ;
#121491 = CIRCLE ( 'NONE', #113101, 0.06509327318403745899 ) ;
#121492 = EDGE_LOOP ( 'NONE', ( #24993, #28667 ) ) ;
#121493 = AXIS2_PLACEMENT_3D ( 'NONE', #50009, #109556, #108886 ) ;
#121494 = DIRECTION ( 'NONE',  ( 0.000000000000000000, 0.000000000000000000, -1.000000000000000000 ) ) ;
#121495 = ORIENTED_EDGE ( 'NONE', *, *, #49351, .T. ) ;
#121496 = DIRECTION ( 'NONE',  ( -4.274815082592931898E-19, -0.9999939076577903929, -0.003490651415223739937 ) ) ;
#121497 = CARTESIAN_POINT ( 'NONE',  ( 2.499999999999947153, 2.500000000000000000, -3.637306695894650055 ) ) ;
#121498 = AXIS2_PLACEMENT_3D ( 'NONE', #32307, #1513, #72213 ) ;
#121499 = VERTEX_POINT ( 'NONE', #89103 ) ;
#121500 = VECTOR ( 'NONE', #39871, 1000.000000000000000 ) ;
#121501 = EDGE_CURVE ( 'NONE', #6155, #127958, #71205, .T. ) ;
#121502 = VERTEX_POINT ( 'NONE', #120495 ) ;
#121503 = ORIENTED_EDGE ( 'NONE', *, *, #126123, .F. ) ;
#121504 = ORIENTED_EDGE ( 'NONE', *, *, #116498, .F. ) ;
#121505 = LINE ( 'NONE', #12204, #21087 ) ;
#121506 = CARTESIAN_POINT ( 'NONE',  ( -8.750000000000010658, 2.500000000000000000, -7.288010851410849256 ) ) ;
#121507 = CARTESIAN_POINT ( 'NONE',  ( -6.900000000000015454, 2.500000000000000000, 3.883716857408420431 ) ) ;
#121508 = EDGE_CURVE ( 'NONE', #115621, #20962, #50454, .T. ) ;
#121509 = FACE_BOUND ( 'NONE', #89174, .T. ) ;
#121510 = EDGE_LOOP ( 'NONE', ( #97495, #126048, #971, #86924 ) ) ;
#121511 = CARTESIAN_POINT ( 'NONE',  ( -0.6000000000000383915, 2.500000000000000000, -3.983716857408426293 ) ) ;
#121512 = CARTESIAN_POINT ( 'NONE',  ( 184.9062500006828031, -8.891194145520236347, -1.633285867636356693E-15 ) ) ;
#121513 = EDGE_CURVE ( 'NONE', #49354, #102850, #64936, .T. ) ;
#121514 = DIRECTION ( 'NONE',  ( 0.000000000000000000, -0.000000000000000000, 1.000000000000000000 ) ) ;
#121515 = DIRECTION ( 'NONE',  ( 0.000000000000000000, -0.000000000000000000, 1.000000000000000000 ) ) ;
#121516 = AXIS2_PLACEMENT_3D ( 'NONE', #4433, #105892, #74500 ) ;
#121517 = AXIS2_PLACEMENT_3D ( 'NONE', #77565, #26552, #58596 ) ;
#121518 = CIRCLE ( 'NONE', #83965, 0.1000000000000002554 ) ;
#121519 = ADVANCED_FACE ( 'NONE', ( #90368 ), #14741, .T. ) ;
#121520 = FACE_OUTER_BOUND ( 'NONE', #22902, .T. ) ;
#121521 = EDGE_CURVE ( 'NONE', #90643, #34472, #40669, .T. ) ;
#121522 = DIRECTION ( 'NONE',  ( -0.000000000000000000, -1.000000000000000000, -0.000000000000000000 ) ) ;
#121523 = UNCERTAINTY_MEASURE_WITH_UNIT (LENGTH_MEASURE( 1.000000000000000082E-05 ), #115286, 'distance_accuracy_value', 'NONE');
#121524 = EDGE_CURVE ( 'NONE', #56692, #49433, #77470, .T. ) ;
#121525 = DIRECTION ( 'NONE',  ( 0.000000000000000000, 1.000000000000000000, 0.000000000000000000 ) ) ;
#121527 = EDGE_CURVE ( 'NONE', #120101, #40494, #20995, .T. ) ;
#121526 = CIRCLE ( 'NONE', #69204, 0.1000000000000000472 ) ;
#121528 = LINE ( 'NONE', #111051, #78687 ) ;
#121529 = EDGE_CURVE ( 'NONE', #69367, #4802, #123519, .T. ) ;
#121530 = ORIENTED_EDGE ( 'NONE', *, *, #125665, .T. ) ;
#121531 = CIRCLE ( 'NONE', #92295, 0.06509327318403745899 ) ;
#121532 = CIRCLE ( 'NONE', #67137, 0.06509327318403745899 ) ;
#121533 = VERTEX_POINT ( 'NONE', #99579 ) ;
#121534 = ORIENTED_EDGE ( 'NONE', *, *, #3192, .T. ) ;
#121535 = VERTEX_POINT ( 'NONE', #8579 ) ;
#121536 = VERTEX_POINT ( 'NONE', #31472 ) ;
#121537 = CARTESIAN_POINT ( 'NONE',  ( -2.500000000000032419, 12.50000000000000000, 0.7579135962115869374 ) ) ;
#121538 = DIRECTION ( 'NONE',  ( 0.000000000000000000, 0.000000000000000000, 1.000000000000000000 ) ) ;
#121539 = VERTEX_POINT ( 'NONE', #51125 ) ;
#121540 = FACE_BOUND ( 'NONE', #59162, .T. ) ;
#121541 = EDGE_CURVE ( 'NONE', #120204, #102205, #9893, .T. ) ;
#121542 = CARTESIAN_POINT ( 'NONE',  ( 195.5000000000000000, 0.000000000000000000, 0.000000000000000000 ) ) ;
#121543 = VERTEX_POINT ( 'NONE', #106320 ) ;
#121544 = CARTESIAN_POINT ( 'NONE',  ( 4.599999999999938360, 2.500000000000000000, -2.276824562219559311E-15 ) ) ;
#121545 = DIRECTION ( 'NONE',  ( -0.000000000000000000, 1.000000000000000000, -0.000000000000000000 ) ) ;
#121546 = CARTESIAN_POINT ( 'NONE',  ( -8.100000000000010303, 12.50000000000000000, 4.676537180435972552 ) ) ;
#121547 = DIRECTION ( 'NONE',  ( 0.000000000000000000, 0.000000000000000000, -1.000000000000000000 ) ) ;
#121548 = ORIENTED_EDGE ( 'NONE', *, *, #55463, .T. ) ;
#121549 = DIRECTION ( 'NONE',  ( 0.000000000000000000, -0.000000000000000000, 1.000000000000000000 ) ) ;
#121550 = ORIENTED_EDGE ( 'NONE', *, *, #4064, .T. ) ;
#121551 = EDGE_LOOP ( 'NONE', ( #14851, #74677, #64928, #107184 ) ) ;
#121552 = CIRCLE ( 'NONE', #111074, 0.1000000000000000472 ) ;
#121553 = ORIENTED_EDGE ( 'NONE', *, *, #119189, .T. ) ;
#121554 = AXIS2_PLACEMENT_3D ( 'NONE', #129399, #40363, #128086 ) ;
#121555 = CARTESIAN_POINT ( 'NONE',  ( 8.749999999999921840, 2.500000000000000000, -5.802370205355749988 ) ) ;
#121556 = AXIS2_PLACEMENT_3D ( 'NONE', #114685, #45972, #14545 ) ;
#121557 = CARTESIAN_POINT ( 'NONE',  ( 5.649999999999934630, 12.50000000000000000, -1.818653347947325916 ) ) ;
#121558 = EDGE_LOOP ( 'NONE', ( #105762, #34136, #25696, #87168 ) ) ;
#121559 = CARTESIAN_POINT ( 'NONE',  ( 9.799999999999913669, 2.500000000000000000, -3.983716857408426293 ) ) ;
#121560 = CARTESIAN_POINT ( 'NONE',  ( 15.83209681635555022, 1.499999999999999556, -5.404881881984138658 ) ) ;
#121561 = VECTOR ( 'NONE', #68700, 1000.000000000000000 ) ;
#121563 = CONICAL_SURFACE ( 'NONE', #16976, 0.1000000000000002554, 0.003490658503988666988 ) ;
#121562 = CARTESIAN_POINT ( 'NONE',  ( -13.14999999999999147, 2.500000000000000000, 1.818653347947325472 ) ) ;
#121564 = DIRECTION ( 'NONE',  ( 0.000000000000000000, 0.000000000000000000, -1.000000000000000000 ) ) ;
#121565 = CARTESIAN_POINT ( 'NONE',  ( 186.4479166673494603, -6.668395609140176816, -3.850000000000003642 ) ) ;
#121566 = VERTEX_POINT ( 'NONE', #48534 ) ;
#121567 = AXIS2_PLACEMENT_3D ( 'NONE', #116251, #26597, #124144 ) ;
#121568 = CARTESIAN_POINT ( 'NONE',  ( -12.49999999999995914, 2.500000000000000000, -4.430127018922199511 ) ) ;
#121569 = ORIENTED_EDGE ( 'NONE', *, *, #45020, .T. ) ;
#121570 = CARTESIAN_POINT ( 'NONE',  ( 3.749999999999975131, 12.50000000000000000, 6.430097255199259010 ) ) ;
#121571 = CIRCLE ( 'NONE', #109042, 0.1000000000000000472 ) ;
#121572 = EDGE_LOOP ( 'NONE', ( #63230, #25821 ) ) ;
#121573 = EDGE_CURVE ( 'NONE', #129420, #65503, #18961, .T. ) ;
#121574 = DIRECTION ( 'NONE',  ( 0.000000000000000000, -0.000000000000000000, 1.000000000000000000 ) ) ;
#121575 = VERTEX_POINT ( 'NONE', #4543 ) ;
#121576 = FACE_OUTER_BOUND ( 'NONE', #38804, .T. ) ;
#121577 = CARTESIAN_POINT ( 'NONE',  ( 13.34999999999990017, 12.50000000000000000, 2.857883832488649301 ) ) ;
#121578 = CARTESIAN_POINT ( 'NONE',  ( -5.600000000000020073, 2.500000000000000000, 0.4464101615137736623 ) ) ;
#121579 = CARTESIAN_POINT ( 'NONE',  ( 6.899999999999928413, 12.50000000000000000, 4.676537180435972552 ) ) ;
#121580 = CARTESIAN_POINT ( 'NONE',  ( -7.900000000000011013, 12.50000000000000000, 3.702399969078682407 ) ) ;
#121581 = ORIENTED_EDGE ( 'NONE', *, *, #53385, .T. ) ;
#121582 = ORIENTED_EDGE ( 'NONE', *, *, #109636, .T. ) ;
#121583 = EDGE_CURVE ( 'NONE', #68393, #45961, #13091, .T. ) ;
#121584 = ORIENTED_EDGE ( 'NONE', *, *, #25165, .F. ) ;
#121585 = CARTESIAN_POINT ( 'NONE',  ( -3.150000000000030109, 2.500000000000000000, 1.818653347947321475 ) ) ;
#121586 = DIRECTION ( 'NONE',  ( 0.000000000000000000, 1.000000000000000000, 0.000000000000000000 ) ) ;
#121587 = CARTESIAN_POINT ( 'NONE',  ( -6.700000000000019718, 12.50000000000000000, -2.385244779468109755E-15 ) ) ;
#121589 = ORIENTED_EDGE ( 'NONE', *, *, #58558, .T. ) ;
#121588 = ORIENTED_EDGE ( 'NONE', *, *, #73218, .T. ) ;
#121590 = ORIENTED_EDGE ( 'NONE', *, *, #86630, .T. ) ;
#121591 = PLANE ( 'NONE',  #6026 ) ;
#121593 = ORIENTED_EDGE ( 'NONE', *, *, #61057, .F. ) ;
#121592 = CIRCLE ( 'NONE', #46287, 0.06509327318403745899 ) ;
#121594 = DIRECTION ( 'NONE',  ( -0.000000000000000000, 1.000000000000000000, -0.000000000000000000 ) ) ;
#121595 = LINE ( 'NONE', #83629, #56119 ) ;
#121596 = AXIS2_PLACEMENT_3D ( 'NONE', #63029, #62397, #1519 ) ;
#121597 = LINE ( 'NONE', #101336, #111747 ) ;
#121598 = CARTESIAN_POINT ( 'NONE',  ( 8.549999999999924327, 2.500000000000000000, -6.841600689897077814 ) ) ;
#121599 = CARTESIAN_POINT ( 'NONE',  ( 12.49999999999990408, 2.500000000000000000, 5.122947341949749323 ) ) ;
#121600 = DIRECTION ( 'NONE',  ( -0.000000000000000000, -1.000000000000000000, -0.000000000000000000 ) ) ;
#121601 = DIRECTION ( 'NONE',  ( 0.000000000000000000, 0.000000000000000000, 1.000000000000000000 ) ) ;
#121603 = AXIS2_PLACEMENT_3D ( 'NONE', #70640, #28145, #30096 ) ;
#121602 = DIRECTION ( 'NONE',  ( 0.000000000000000000, 1.000000000000000000, 0.000000000000000000 ) ) ;
#121604 = ORIENTED_EDGE ( 'NONE', *, *, #30070, .T. ) ;
#121605 = CIRCLE ( 'NONE', #25445, 0.1000000000000000472 ) ;
#121606 = AXIS2_PLACEMENT_3D ( 'NONE', #54868, #76462, #124914 ) ;
#121607 = LINE ( 'NONE', #72534, #2649 ) ;
#121608 = CONICAL_SURFACE ( 'NONE', #56744, 0.1000000000000002554, 0.003490658503988666988 ) ;
#121609 = CARTESIAN_POINT ( 'NONE',  ( -4.800000000000022915, 2.500000000000000000, -0.2464101615137783419 ) ) ;
#121610 = ORIENTED_EDGE ( 'NONE', *, *, #76568, .T. ) ;
#121611 = EDGE_LOOP ( 'NONE', ( #67142, #76017 ) ) ;
#121612 = CARTESIAN_POINT ( 'NONE',  ( 183.8593750003413732, 0.000000000000000000, 7.564683531250000925 ) ) ;
#121613 = CARTESIAN_POINT ( 'NONE',  ( -8.550000000000013145, 2.500000000000000000, -6.941600689897073906 ) ) ;
#121614 = DIRECTION ( 'NONE',  ( -0.000000000000000000, 1.000000000000000000, -0.000000000000000000 ) ) ;
#121615 = VECTOR ( 'NONE', #125379, 1000.000000000000000 ) ;
#121616 = LINE ( 'NONE', #62725, #55220 ) ;
#121617 = CARTESIAN_POINT ( 'NONE',  ( 3.349999999999945466, 12.50000000000000000, -7.253104124594891289 ) ) ;
#121618 = AXIS2_PLACEMENT_3D ( 'NONE', #61823, #32382, #22547 ) ;
#121619 = ADVANCED_FACE ( 'NONE', ( #91675 ), #110903, .T. ) ;
#121620 = CARTESIAN_POINT ( 'NONE',  ( -6.700000000000019718, 12.50000000000000000, -2.385244779468109755E-15 ) ) ;
#121621 = CIRCLE ( 'NONE', #6669, 0.1000000000000000056 ) ;
#121622 = DIRECTION ( 'NONE',  ( 0.000000000000000000, -0.9999939076577903929, 0.003490651415223739937 ) ) ;
#121623 = VECTOR ( 'NONE', #21813, 1000.000000000000000 ) ;
#121624 = DIRECTION ( 'NONE',  ( 0.000000000000000000, 0.000000000000000000, 1.000000000000000000 ) ) ;
#121625 = AXIS2_PLACEMENT_3D ( 'NONE', #38362, #86128, #17392 ) ;
#121626 = AXIS2_PLACEMENT_3D ( 'NONE', #122026, #289, #61827 ) ;
#121627 = LINE ( 'NONE', #90223, #85546 ) ;
#121628 = EDGE_CURVE ( 'NONE', #84054, #111888, #29450, .T. ) ;
#121629 = ORIENTED_EDGE ( 'NONE', *, *, #21028, .F. ) ;
#121630 = ORIENTED_EDGE ( 'NONE', *, *, #103821, .F. ) ;
#121631 = AXIS2_PLACEMENT_3D ( 'NONE', #96262, #54415, #74709 ) ;
#121632 = ORIENTED_EDGE ( 'NONE', *, *, #16067, .T. ) ;
#121633 = EDGE_CURVE ( 'NONE', #50907, #14841, #83815, .T. ) ;
#121634 = VERTEX_POINT ( 'NONE', #33418 ) ;
#121635 = EDGE_CURVE ( 'NONE', #92388, #89740, #60840, .T. ) ;
#121636 = CARTESIAN_POINT ( 'NONE',  ( -1.250000000000037970, 12.50000000000000000, 7.188010851410848723 ) ) ;
#121637 = CARTESIAN_POINT ( 'NONE',  ( 5.199999999999933564, 12.50000000000000000, 3.983716857408420076 ) ) ;
#121638 = ORIENTED_EDGE ( 'NONE', *, *, #75222, .T. ) ;
#121639 = CARTESIAN_POINT ( 'NONE',  ( -2.900000000000029221, 2.500000000000000000, -4.330127018922201643 ) ) ;
#121640 = DIRECTION ( 'NONE',  ( 0.000000000000000000, 0.000000000000000000, -1.000000000000000000 ) ) ;
#121641 = EDGE_CURVE ( 'NONE', #46605, #125318, #69144, .T. ) ;
#121642 = DIRECTION ( 'NONE',  ( 0.000000000000000000, 0.000000000000000000, 1.000000000000000000 ) ) ;
#121644 = VERTEX_POINT ( 'NONE', #121767 ) ;
#121643 = DIRECTION ( 'NONE',  ( 0.000000000000000000, 0.000000000000000000, 1.000000000000000000 ) ) ;
#121645 = ADVANCED_FACE ( 'NONE', ( #11817 ), #14834, .T. ) ;
#121646 = CARTESIAN_POINT ( 'NONE',  ( -4.550000000000026468, 2.500000000000000000, -6.395190528383301931 ) ) ;
#121647 = DIRECTION ( 'NONE',  ( 0.000000000000000000, -0.000000000000000000, 1.000000000000000000 ) ) ;
#121648 = VERTEX_POINT ( 'NONE', #73310 ) ;
#121649 = ORIENTED_EDGE ( 'NONE', *, *, #80724, .T. ) ;
#121650 = ORIENTED_EDGE ( 'NONE', *, *, #109737, .F. ) ;
#121651 = AXIS2_PLACEMENT_3D ( 'NONE', #99974, #59426, #99331 ) ;
#121652 = ORIENTED_EDGE ( 'NONE', *, *, #109832, .F. ) ;
#121653 = CARTESIAN_POINT ( 'NONE',  ( -10.20000000000000462, 2.500000000000000000, 0.2464101615137735679 ) ) ;
#121654 = CONICAL_SURFACE ( 'NONE', #88279, 0.1000000000000000472, 0.003490658503988666988 ) ;
#121655 = VECTOR ( 'NONE', #18429, 1000.000000000000000 ) ;
#121656 = DIRECTION ( 'NONE',  ( -0.000000000000000000, -1.000000000000000000, -0.000000000000000000 ) ) ;
#121657 = CARTESIAN_POINT ( 'NONE',  ( -11.44999999999999751, 12.50000000000000000, -6.841600689897074261 ) ) ;
#121659 = EDGE_LOOP ( 'NONE', ( #69175, #47331, #60244, #46203 ) ) ;
#121658 = AXIS2_PLACEMENT_3D ( 'NONE', #13323, #53280, #83996 ) ;
#121660 = AXIS2_PLACEMENT_3D ( 'NONE', #102167, #52412, #92331 ) ;
#121661 = AXIS2_PLACEMENT_3D ( 'NONE', #33697, #4217, #16449 ) ;
#121662 = CARTESIAN_POINT ( 'NONE',  ( 3.349999999999945466, 12.50000000000000000, -6.495190528383302464 ) ) ;
#121663 = VERTEX_POINT ( 'NONE', #103433 ) ;
#121664 = FACE_OUTER_BOUND ( 'NONE', #49060, .T. ) ;
#121665 = CARTESIAN_POINT ( 'NONE',  ( 16.70850060796060887, -0.4765610498145435026, -5.930927070179899729 ) ) ;
#121666 = AXIS2_PLACEMENT_3D ( 'NONE', #82055, #61796, #32352 ) ;
#121667 = DIRECTION ( 'NONE',  ( 0.000000000000000000, 0.000000000000000000, 1.000000000000000000 ) ) ;
#121668 = DIRECTION ( 'NONE',  ( -0.000000000000000000, 1.000000000000000000, -0.000000000000000000 ) ) ;
#121669 = CIRCLE ( 'NONE', #61135, 0.06509327318403745899 ) ;
#121670 = VERTEX_POINT ( 'NONE', #51758 ) ;
#121671 = VERTEX_POINT ( 'NONE', #102145 ) ;
#121672 = ORIENTED_EDGE ( 'NONE', *, *, #11133, .T. ) ;
#121673 = CARTESIAN_POINT ( 'NONE',  ( -2.050000000000033129, 12.50000000000000000, 2.165063509461097713 ) ) ;
#121674 = DIRECTION ( 'NONE',  ( 0.000000000000000000, 0.000000000000000000, -1.000000000000000000 ) ) ;
#121675 = DIRECTION ( 'NONE',  ( -4.274815082592931898E-19, -0.9999939076577903929, -0.003490651415223739937 ) ) ;
#121676 = FACE_BOUND ( 'NONE', #80215, .T. ) ;
#121677 = DIRECTION ( 'NONE',  ( -4.274815082592931898E-19, -0.9999939076577903929, -0.003490651415223739937 ) ) ;
#121678 = FACE_OUTER_BOUND ( 'NONE', #97780, .T. ) ;
#121679 = EDGE_CURVE ( 'NONE', #75247, #104608, #6417, .T. ) ;
#121680 = DIRECTION ( 'NONE',  ( 0.000000000000000000, 1.000000000000000000, 0.000000000000000000 ) ) ;
#121681 = ADVANCED_FACE ( 'NONE', ( #23574 ), #98467, .T. ) ;
#121682 = ADVANCED_FACE ( 'NONE', ( #72686 ), #94277, .T. ) ;
#121683 = DIRECTION ( 'NONE',  ( 0.000000000000000000, 1.000000000000000000, 0.000000000000000000 ) ) ;
#121684 = DIRECTION ( 'NONE',  ( -0.000000000000000000, 1.000000000000000000, -0.000000000000000000 ) ) ;
#121685 = ADVANCED_FACE ( 'NONE', ( #41944 ), #104731, .T. ) ;
#121686 = DIRECTION ( 'NONE',  ( 0.000000000000000000, 0.000000000000000000, 1.000000000000000000 ) ) ;
#121687 = EDGE_LOOP ( 'NONE', ( #30122, #129229 ) ) ;
#121688 = EDGE_CURVE ( 'NONE', #73789, #83814, #121465, .T. ) ;
#121689 = CARTESIAN_POINT ( 'NONE',  ( -1.850000000000033396, 12.50000000000000000, -2.446380397790840266 ) ) ;
#121690 = CARTESIAN_POINT ( 'NONE',  ( -8.750000000000007105, 2.500000000000000000, 7.088010851410848190 ) ) ;
#121691 = ADVANCED_FACE ( 'NONE', ( #73968 ), #21212, .T. ) ;
#121692 = EDGE_LOOP ( 'NONE', ( #37473, #124734, #8099, #80983 ) ) ;
#121693 = EDGE_LOOP ( 'NONE', ( #76999, #100752 ) ) ;
#121694 = DIRECTION ( 'NONE',  ( 0.000000000000000000, 0.000000000000000000, -1.000000000000000000 ) ) ;
#121695 = DIRECTION ( 'NONE',  ( 0.000000000000000000, 1.000000000000000000, 0.000000000000000000 ) ) ;
#121696 = FACE_BOUND ( 'NONE', #116148, .T. ) ;
#121697 = AXIS2_PLACEMENT_3D ( 'NONE', #88164, #27319, #109101 ) ;
#121698 = CARTESIAN_POINT ( 'NONE',  ( 7.049999999999930544, 2.500000000000000000, -6.495190528383302464 ) ) ;
#121699 = CIRCLE ( 'NONE', #65254, 0.06509327318403745899 ) ;
#121700 = EDGE_CURVE ( 'NONE', #68510, #68006, #65012, .T. ) ;
#121701 = AXIS2_PLACEMENT_3D ( 'NONE', #109396, #120516, #89118 ) ;
#121702 = EDGE_CURVE ( 'NONE', #6433, #73886, #113155, .T. ) ;
#121703 = ORIENTED_EDGE ( 'NONE', *, *, #96260, .F. ) ;
#121704 = CARTESIAN_POINT ( 'NONE',  ( 10.64999999999991331, 2.500000000000000000, 6.941600689897073018 ) ) ;
#121705 = CARTESIAN_POINT ( 'NONE',  ( 11.44999999999990870, 2.500000000000000000, -1.818653347947326138 ) ) ;
#121706 = VERTEX_POINT ( 'NONE', #102766 ) ;
#121708 = PLANE ( 'NONE',  #38621 ) ;
#121707 = CIRCLE ( 'NONE', #102932, 0.1000000000000000472 ) ;
#121709 = DIRECTION ( 'NONE',  ( 0.000000000000000000, -0.000000000000000000, 1.000000000000000000 ) ) ;
#121710 = VECTOR ( 'NONE', #120575, 1000.000000000000000 ) ;
#121711 = AXIS2_PLACEMENT_3D ( 'NONE', #91022, #58986, #81208 ) ;
#121712 = CONICAL_SURFACE ( 'NONE', #102940, 0.1000000000000002554, 0.003490658503988666988 ) ;
#121713 = CIRCLE ( 'NONE', #104978, 0.06509327318403745899 ) ;
#121714 = VERTEX_POINT ( 'NONE', #53046 ) ;
#121715 = DIRECTION ( 'NONE',  ( -0.000000000000000000, -1.000000000000000000, -0.000000000000000000 ) ) ;
#121716 = CARTESIAN_POINT ( 'NONE',  ( -2.700000000000030820, 2.500000000000000000, -3.883716857408426648 ) ) ;
#121717 = AXIS2_PLACEMENT_3D ( 'NONE', #34638, #121695, #84358 ) ;
#121718 = ORIENTED_EDGE ( 'NONE', *, *, #120361, .F. ) ;
#121719 = DIRECTION ( 'NONE',  ( -0.000000000000000000, -1.000000000000000000, -0.000000000000000000 ) ) ;
#121720 = AXIS2_PLACEMENT_3D ( 'NONE', #29481, #109321, #118489 ) ;
#121721 = DIRECTION ( 'NONE',  ( -0.000000000000000000, -1.000000000000000000, -0.000000000000000000 ) ) ;
#121722 = CARTESIAN_POINT ( 'NONE',  ( -5.000000000000023093, 12.50000000000000000, 0.6277270498435120194 ) ) ;
#121723 = VERTEX_POINT ( 'NONE', #92975 ) ;
#121724 = ORIENTED_EDGE ( 'NONE', *, *, #101862, .F. ) ;
#121725 = CARTESIAN_POINT ( 'NONE',  ( -9.400000000000007461, 12.50000000000000000, 0.3464101615137735735 ) ) ;
#121726 = EDGE_LOOP ( 'NONE', ( #75609, #84724, #112586, #15640 ) ) ;
#121727 = FACE_OUTER_BOUND ( 'NONE', #63529, .T. ) ;
#121728 = CARTESIAN_POINT ( 'NONE',  ( 15.19999999999989271, 2.500000000000000000, -0.4464101615137783252 ) ) ;
#121729 = CARTESIAN_POINT ( 'NONE',  ( -13.54999999999999005, 2.500000000000000000, 2.511473670974877503 ) ) ;
#121730 = EDGE_LOOP ( 'NONE', ( #10748, #75751, #4489, #59091 ) ) ;
#121731 = FACE_OUTER_BOUND ( 'NONE', #78820, .T. ) ;
#121732 = DIRECTION ( 'NONE',  ( -0.000000000000000000, 1.000000000000000000, -0.000000000000000000 ) ) ;
#121733 = DIRECTION ( 'NONE',  ( 0.000000000000000000, 0.000000000000000000, 1.000000000000000000 ) ) ;
#121734 = DIRECTION ( 'NONE',  ( 0.000000000000000000, -0.9999939076577903929, 0.003490651415223739937 ) ) ;
#121735 = FACE_OUTER_BOUND ( 'NONE', #15733, .T. ) ;
#121736 = DIRECTION ( 'NONE',  ( -0.000000000000000000, 1.000000000000000000, -0.000000000000000000 ) ) ;
#121737 = ORIENTED_EDGE ( 'NONE', *, *, #57893, .T. ) ;
#121738 = ADVANCED_FACE ( 'NONE', ( #3297 ), #74612, .T. ) ;
#121739 = ORIENTED_EDGE ( 'NONE', *, *, #51210, .T. ) ;
#121740 = DIRECTION ( 'NONE',  ( -0.000000000000000000, 1.000000000000000000, -0.000000000000000000 ) ) ;
#121741 = ORIENTED_EDGE ( 'NONE', *, *, #126281, .F. ) ;
#121742 = AXIS2_PLACEMENT_3D ( 'NONE', #60558, #9502, #38995 ) ;
#121743 = CARTESIAN_POINT ( 'NONE',  ( 11.69999999999990514, 12.50000000000000000, -2.276824562219559311E-15 ) ) ;
#121744 = AXIS2_PLACEMENT_3D ( 'NONE', #52355, #62829, #92270 ) ;
#121745 = CIRCLE ( 'NONE', #6794, 0.06509327318403745899 ) ;
#121747 = ORIENTED_EDGE ( 'NONE', *, *, #118278, .T. ) ;
#121746 = ORIENTED_EDGE ( 'NONE', *, *, #115979, .T. ) ;
#121748 = VERTEX_POINT ( 'NONE', #55615 ) ;
#121749 = DIRECTION ( 'NONE',  ( 0.000000000000000000, 0.000000000000000000, -1.000000000000000000 ) ) ;
#121750 = LINE ( 'NONE', #72031, #4650 ) ;
#121751 = AXIS2_PLACEMENT_3D ( 'NONE', #115147, #35979, #64784 ) ;
#121753 = FACE_OUTER_BOUND ( 'NONE', #85183, .T. ) ;
#121752 = AXIS2_PLACEMENT_3D ( 'NONE', #118420, #30062, #58864 ) ;
#121754 = AXIS2_PLACEMENT_3D ( 'NONE', #101485, #41925, #83141 ) ;
#121755 = LINE ( 'NONE', #14999, #32728 ) ;
#121756 = DIRECTION ( 'NONE',  ( -0.000000000000000000, 1.000000000000000000, -0.000000000000000000 ) ) ;
#121757 = LINE ( 'NONE', #72035, #119657 ) ;
#121758 = AXIS2_PLACEMENT_3D ( 'NONE', #6442, #46393, #86314 ) ;
#121759 = CARTESIAN_POINT ( 'NONE',  ( 1.649999999999948841, 2.500000000000000000, 6.595190528383296780 ) ) ;
#121760 = CARTESIAN_POINT ( 'NONE',  ( 6.449999999999930012, 12.50000000000000000, 6.906693963081109722 ) ) ;
#121761 = CARTESIAN_POINT ( 'NONE',  ( 0.3999999999999555023, 2.500000000000000000, 4.330127018922196314 ) ) ;
#121762 = CIRCLE ( 'NONE', #111373, 0.1000000000000000056 ) ;
#121763 = ORIENTED_EDGE ( 'NONE', *, *, #22406, .F. ) ;
#121764 = CARTESIAN_POINT ( 'NONE',  ( 14.79999999999989235, 12.50000000000000000, 0.3464101615137735735 ) ) ;
#121765 = ORIENTED_EDGE ( 'NONE', *, *, #29572, .F. ) ;
#121766 = ORIENTED_EDGE ( 'NONE', *, *, #57166, .F. ) ;
#121767 = CARTESIAN_POINT ( 'NONE',  ( 12.89999999999990266, 12.50000000000000000, -5.088040615133791356 ) ) ;
#121768 = LINE ( 'NONE', #51759, #20452 ) ;
#121769 = CARTESIAN_POINT ( 'NONE',  ( 11.44999999999990870, 12.50000000000000000, 6.841600689897072485 ) ) ;
#121770 = CARTESIAN_POINT ( 'NONE',  ( -11.64999999999999680, 2.500000000000000000, 2.165063509461097713 ) ) ;
#121771 = DIRECTION ( 'NONE',  ( 0.000000000000000000, 0.000000000000000000, 1.000000000000000000 ) ) ;
#121772 = DIRECTION ( 'NONE',  ( -0.000000000000000000, 1.000000000000000000, -0.000000000000000000 ) ) ;
#121773 = CARTESIAN_POINT ( 'NONE',  ( 5.649999999999936406, 12.50000000000000000, -6.083687093685488989 ) ) ;
#121774 = EDGE_LOOP ( 'NONE', ( #47223, #124503, #46843, #87196 ) ) ;
#121775 = EDGE_LOOP ( 'NONE', ( #37182, #63716, #84334, #35801 ) ) ;
#121776 = ADVANCED_FACE ( 'NONE', ( #114520 ), #110992, .T. ) ;
#121777 = VECTOR ( 'NONE', #86455, 1000.000000000000000 ) ;
#121778 = ORIENTED_EDGE ( 'NONE', *, *, #110865, .F. ) ;
#121779 = ORIENTED_EDGE ( 'NONE', *, *, #21327, .T. ) ;
#121780 = ADVANCED_FACE ( 'NONE', ( #116457 ), #42068, .T. ) ;
#121781 = ORIENTED_EDGE ( 'NONE', *, *, #32172, .T. ) ;
#121782 = CIRCLE ( 'NONE', #90382, 0.1000000000000002554 ) ;
#121783 = EDGE_CURVE ( 'NONE', #92818, #56590, #54556, .T. ) ;
#121784 = CYLINDRICAL_SURFACE ( 'NONE', #117177, 7.700000000000000178 ) ;
#121785 = DIRECTION ( 'NONE',  ( -0.000000000000000000, -1.000000000000000000, -0.000000000000000000 ) ) ;
#121786 = AXIS2_PLACEMENT_3D ( 'NONE', #31964, #81062, #112458 ) ;
#121787 = AXIS2_PLACEMENT_3D ( 'NONE', #102266, #73429, #103559 ) ;
#121788 = CARTESIAN_POINT ( 'NONE',  ( 12.49999999999993960, 12.50000000000000000, 4.330127018922196314 ) ) ;
#121789 = AXIS2_PLACEMENT_3D ( 'NONE', #40867, #110849, #61120 ) ;
#121790 = DIRECTION ( 'NONE',  ( 0.000000000000000000, 1.000000000000000000, 0.000000000000000000 ) ) ;
#121791 = ADVANCED_FACE ( 'NONE', ( #115820 ), #85710, .T. ) ;
#121792 = DIRECTION ( 'NONE',  ( 0.000000000000000000, 0.000000000000000000, 1.000000000000000000 ) ) ;
#121794 = ORIENTED_EDGE ( 'NONE', *, *, #71246, .T. ) ;
#121793 = EDGE_CURVE ( 'NONE', #56841, #35476, #25312, .T. ) ;
#121795 = CARTESIAN_POINT ( 'NONE',  ( 0.3999999999999628852, 2.500000000000000000, -0.7928203230275520097 ) ) ;
#121796 = CARTESIAN_POINT ( 'NONE',  ( -10.45000000000000462, 2.500000000000000000, -2.165063509461097713 ) ) ;
#121797 = EDGE_CURVE ( 'NONE', #110118, #22205, #37845, .T. ) ;
#121798 = FACE_OUTER_BOUND ( 'NONE', #53785, .T. ) ;
#121799 = EDGE_CURVE ( 'NONE', #108367, #106850, #26802, .T. ) ;
#121800 = LINE ( 'NONE', #3325, #32632 ) ;
#121801 = AXIS2_PLACEMENT_3D ( 'NONE', #128300, #118455, #50367 ) ;
#121802 = AXIS2_PLACEMENT_3D ( 'NONE', #65512, #17694, #88359 ) ;
#121803 = DIRECTION ( 'NONE',  ( -0.000000000000000000, 1.000000000000000000, -0.000000000000000000 ) ) ;
#121804 = ORIENTED_EDGE ( 'NONE', *, *, #108817, .F. ) ;
#121805 = AXIS2_PLACEMENT_3D ( 'NONE', #49673, #100045, #58201 ) ;
#121806 = AXIS2_PLACEMENT_3D ( 'NONE', #32780, #45802, #13736 ) ;
#121807 = EDGE_LOOP ( 'NONE', ( #6018, #20355 ) ) ;
#121808 = ORIENTED_EDGE ( 'NONE', *, *, #74940, .T. ) ;
#121809 = FACE_OUTER_BOUND ( 'NONE', #120288, .T. ) ;
#121810 = EDGE_CURVE ( 'NONE', #75902, #84566, #127735, .T. ) ;
#121811 = CIRCLE ( 'NONE', #82109, 0.09999999999999999167 ) ;
#121812 = VERTEX_POINT ( 'NONE', #37279 ) ;
#121813 = FACE_OUTER_BOUND ( 'NONE', #6691, .T. ) ;
#121814 = FACE_OUTER_BOUND ( 'NONE', #75867, .T. ) ;
#121815 = CIRCLE ( 'NONE', #117587, 0.1000000000000002554 ) ;
#121816 = EDGE_LOOP ( 'NONE', ( #47891, #101651 ) ) ;
#121817 = CARTESIAN_POINT ( 'NONE',  ( -8.750000000000005329, 2.500000000000000000, 5.702370205355745014 ) ) ;
#121818 = CARTESIAN_POINT ( 'NONE',  ( -12.49999999999999289, 12.50000000000000000, 3.702399969078682407 ) ) ;
#121819 = CARTESIAN_POINT ( 'NONE',  ( -14.54999999999998472, 2.500000000000000000, -2.065063509461099844 ) ) ;
#121820 = CARTESIAN_POINT ( 'NONE',  ( 4.349999999999941025, 2.500000000000000000, -6.148780366869526226 ) ) ;
#121821 = CARTESIAN_POINT ( 'NONE',  ( 7.699999999999923794, 12.50000000000000000, -0.3464101615137783474 ) ) ;
#121822 = ORIENTED_EDGE ( 'NONE', *, *, #117835, .T. ) ;
#121823 = AXIS2_PLACEMENT_3D ( 'NONE', #70099, #58990, #98900 ) ;
#121824 = ORIENTED_EDGE ( 'NONE', *, *, #95250, .T. ) ;
#121826 = EDGE_CURVE ( 'NONE', #93625, #97708, #71288, .T. ) ;
#121825 = CONICAL_SURFACE ( 'NONE', #52888, 0.09999999999999999167, 0.003490658503988666988 ) ;
#121827 = CARTESIAN_POINT ( 'NONE',  ( 7.899999999999924860, 2.500000000000000000, -3.537306695894649966 ) ) ;
#121828 = DIRECTION ( 'NONE',  ( 0.000000000000000000, -0.9999939076577903929, 0.003490651415223739937 ) ) ;
#121829 = DIRECTION ( 'NONE',  ( 0.000000000000000000, 0.000000000000000000, 1.000000000000000000 ) ) ;
#121830 = LINE ( 'NONE', #12519, #41730 ) ;
#121831 = VERTEX_POINT ( 'NONE', #86349 ) ;
#121832 = CONICAL_SURFACE ( 'NONE', #109318, 0.1000000000000002554, 0.003490658503988666988 ) ;
#121833 = AXIS2_PLACEMENT_3D ( 'NONE', #28431, #19904, #59849 ) ;
#121834 = VERTEX_POINT ( 'NONE', #97472 ) ;
#121835 = EDGE_CURVE ( 'NONE', #24133, #99929, #92216, .T. ) ;
#121836 = DIRECTION ( 'NONE',  ( -4.274815082592931898E-19, -0.9999939076577903929, -0.003490651415223739937 ) ) ;
#121837 = DIRECTION ( 'NONE',  ( -0.000000000000000000, -1.000000000000000000, -0.000000000000000000 ) ) ;
#121838 = DIRECTION ( 'NONE',  ( -0.000000000000000000, -1.000000000000000000, -0.000000000000000000 ) ) ;
#121839 = ADVANCED_FACE ( 'NONE', ( #126295 ), #47739, .T. ) ;
#121840 = CARTESIAN_POINT ( 'NONE',  ( -7.300000000000016698, 12.50000000000000000, -4.611443907251940644 ) ) ;
#121841 = ORIENTED_EDGE ( 'NONE', *, *, #73987, .T. ) ;
#121843 = CARTESIAN_POINT ( 'NONE',  ( 8.749999999999923617, 12.50000000000000000, 1.407149913249508000 ) ) ;
#121842 = CIRCLE ( 'NONE', #4754, 0.09999999999999982514 ) ;
#121844 = CIRCLE ( 'NONE', #126041, 0.06509327318403745899 ) ;
#121845 = EDGE_CURVE ( 'NONE', #79920, #8444, #35798, .T. ) ;
#121846 = DIRECTION ( 'NONE',  ( 0.000000000000000000, 0.000000000000000000, 1.000000000000000000 ) ) ;
#121847 = CIRCLE ( 'NONE', #11025, 0.09999999999999982514 ) ;
#121848 = VERTEX_POINT ( 'NONE', #47101 ) ;
#121849 = CIRCLE ( 'NONE', #52910, 0.1000000000000002554 ) ;
#121850 = DIRECTION ( 'NONE',  ( 0.000000000000000000, 1.000000000000000000, 0.000000000000000000 ) ) ;
#121851 = EDGE_CURVE ( 'NONE', #7001, #55449, #52521, .T. ) ;
#121852 = ORIENTED_EDGE ( 'NONE', *, *, #41722, .T. ) ;
#121853 = CIRCLE ( 'NONE', #88388, 0.1000000000000002554 ) ;
#121854 = CARTESIAN_POINT ( 'NONE',  ( 1.049999999999954081, 12.50000000000000000, -6.213873640053564351 ) ) ;
#121855 = EDGE_CURVE ( 'NONE', #35899, #30305, #85947, .T. ) ;
#121856 = ADVANCED_FACE ( 'NONE', ( #124999 ), #123608, .T. ) ;
#121857 = ADVANCED_FACE ( 'NONE', ( #117092 ), #29541, .T. ) ;
#121858 = EDGE_LOOP ( 'NONE', ( #63137, #84935 ) ) ;
#121859 = DIRECTION ( 'NONE',  ( 0.000000000000000000, 0.000000000000000000, 1.000000000000000000 ) ) ;
#121860 = CARTESIAN_POINT ( 'NONE',  ( 12.30568799055497564, 2.500000000000001776, -7.490555763477717122 ) ) ;
#121861 = VERTEX_POINT ( 'NONE', #49686 ) ;
#121862 = ORIENTED_EDGE ( 'NONE', *, *, #25800, .T. ) ;
#121863 = CARTESIAN_POINT ( 'NONE',  ( -7.300000000000013145, 2.500000000000000000, 4.083716857408420609 ) ) ;
#121864 = CARTESIAN_POINT ( 'NONE',  ( -3.750000000000031086, 2.500000000000000000, -5.902370205355750521 ) ) ;
#121865 = EDGE_CURVE ( 'NONE', #68456, #45964, #6510, .T. ) ;
#121866 = AXIS2_PLACEMENT_3D ( 'NONE', #121195, #31535, #119913 ) ;
#121867 = LINE ( 'NONE', #1444, #80280 ) ;
#121868 = CARTESIAN_POINT ( 'NONE',  ( 185.6510416670080303, 4.367472073101518859, -7.564683531249999149 ) ) ;
#121869 = DIRECTION ( 'NONE',  ( 0.000000000000000000, -0.9999939076577903929, 0.003490651415223739937 ) ) ;
#121870 = CARTESIAN_POINT ( 'NONE',  ( -14.79999999999998472, 2.500000000000000000, 0.3464101615137758494 ) ) ;
#121871 = CARTESIAN_POINT ( 'NONE',  ( -3.750000000000031086, 2.500000000000000000, -5.702370205355749455 ) ) ;
#121872 = DIRECTION ( 'NONE',  ( 0.000000000000000000, 0.000000000000000000, 1.000000000000000000 ) ) ;
#121873 = CARTESIAN_POINT ( 'NONE',  ( 1.649999999999951505, 2.500000000000000000, -2.857883832488653741 ) ) ;
#121874 = CIRCLE ( 'NONE', #27778, 0.06509327318403745899 ) ;
#121875 = CIRCLE ( 'NONE', #80119, 0.1000000000000000472 ) ;
#121876 = CIRCLE ( 'NONE', #86368, 0.09999999999999982514 ) ;
#121877 = VERTEX_POINT ( 'NONE', #39868 ) ;
#121878 = ORIENTED_EDGE ( 'NONE', *, *, #62147, .F. ) ;
#121879 = DIRECTION ( 'NONE',  ( 0.000000000000000000, 0.000000000000000000, 1.000000000000000000 ) ) ;
#121880 = EDGE_LOOP ( 'NONE', ( #36752, #40044, #72942, #38879 ) ) ;
#121881 = CARTESIAN_POINT ( 'NONE',  ( 12.69999999999989981, 12.50000000000000000, -0.4115034346978157509 ) ) ;
#121882 = CARTESIAN_POINT ( 'NONE',  ( -2.900000000000030109, 12.50000000000000000, -3.637306695894650055 ) ) ;
#121883 = DIRECTION ( 'NONE',  ( 0.000000000000000000, 0.000000000000000000, 1.000000000000000000 ) ) ;
#121885 = EDGE_LOOP ( 'NONE', ( #68610, #66011 ) ) ;
#121884 = EDGE_LOOP ( 'NONE', ( #41651, #30416, #60862, #67098 ) ) ;
#121886 = FACE_BOUND ( 'NONE', #24674, .T. ) ;
#121887 = ORIENTED_EDGE ( 'NONE', *, *, #15974, .F. ) ;
#121888 = CIRCLE ( 'NONE', #98901, 0.1000000000000002554 ) ;
#121889 = DIRECTION ( 'NONE',  ( -0.000000000000000000, -1.000000000000000000, -0.000000000000000000 ) ) ;
#121890 = DIRECTION ( 'NONE',  ( 0.000000000000000000, 1.000000000000000000, 0.000000000000000000 ) ) ;
#121891 = VECTOR ( 'NONE', #45003, 1000.000000000000000 ) ;
#121893 = LINE ( 'NONE', #123194, #61786 ) ;
#121892 = AXIS2_PLACEMENT_3D ( 'NONE', #42722, #94359, #91795 ) ;
#121894 = CARTESIAN_POINT ( 'NONE',  ( 6.249999999999968914, 12.50000000000000000, -6.495190528383302464 ) ) ;
#121895 = AXIS2_PLACEMENT_3D ( 'NONE', #32817, #103471, #104117 ) ;
#121896 = DIRECTION ( 'NONE',  ( -4.274815082592931898E-19, -0.9999939076577903929, -0.003490651415223739937 ) ) ;
#121897 = DIRECTION ( 'NONE',  ( -0.000000000000000000, 1.000000000000000000, -0.000000000000000000 ) ) ;
#121898 = DIRECTION ( 'NONE',  ( 0.000000000000000000, 0.000000000000000000, 1.000000000000000000 ) ) ;
#121899 = DIRECTION ( 'NONE',  ( 0.000000000000000000, -0.000000000000000000, 1.000000000000000000 ) ) ;
#121900 = CARTESIAN_POINT ( 'NONE',  ( -8.950000000000009948, 2.500000000000000000, -6.741600689897071952 ) ) ;
#121901 = CARTESIAN_POINT ( 'NONE',  ( -11.89999999999999680, 2.500000000000000000, -0.3464101615137741841 ) ) ;
#121902 = CIRCLE ( 'NONE', #61275, 0.06509327318403745899 ) ;
#121903 = DIRECTION ( 'NONE',  ( 0.000000000000000000, 0.000000000000000000, 1.000000000000000000 ) ) ;
#121904 = EDGE_LOOP ( 'NONE', ( #49280, #124448 ) ) ;
#121905 = ORIENTED_EDGE ( 'NONE', *, *, #118116, .F. ) ;
#121906 = ADVANCED_FACE ( 'NONE', ( #68656 ), #84584, .F. ) ;
#121907 = ORIENTED_EDGE ( 'NONE', *, *, #129287, .T. ) ;
#121908 = DIRECTION ( 'NONE',  ( -0.000000000000000000, -1.000000000000000000, -0.000000000000000000 ) ) ;
#121910 = EDGE_LOOP ( 'NONE', ( #57705, #96133 ) ) ;
#121909 = AXIS2_PLACEMENT_3D ( 'NONE', #108963, #118160, #90633 ) ;
#121911 = VECTOR ( 'NONE', #8123, 1000.000000000000000 ) ;
#121912 = AXIS2_PLACEMENT_3D ( 'NONE', #90841, #81029, #120941 ) ;
#121913 = DIRECTION ( 'NONE',  ( 0.000000000000000000, 0.000000000000000000, 1.000000000000000000 ) ) ;
#121914 = CARTESIAN_POINT ( 'NONE',  ( -3.550000000000027800, 2.500000000000000000, 6.048780366869520364 ) ) ;
#121916 = EDGE_LOOP ( 'NONE', ( #84452, #113055 ) ) ;
#121915 = ORIENTED_EDGE ( 'NONE', *, *, #75545, .T. ) ;
#121917 = EDGE_LOOP ( 'NONE', ( #10616, #64290, #96168, #7398 ) ) ;
#121918 = CONICAL_SURFACE ( 'NONE', #25761, 0.1000000000000002554, 0.003490658503988666988 ) ;
#121919 = CARTESIAN_POINT ( 'NONE',  ( 7.699999999999922018, 2.500000000000000000, 0.3464101615137735735 ) ) ;
#121920 = CARTESIAN_POINT ( 'NONE',  ( -10.20000000000000462, 12.50000000000000000, 0.3464101615137735735 ) ) ;
#121921 = CONICAL_SURFACE ( 'NONE', #12950, 0.1000000000000002554, 0.003490658503988666988 ) ;
#121922 =( NAMED_UNIT ( * ) SI_UNIT ( $, .STERADIAN. ) SOLID_ANGLE_UNIT ( ) );
#121923 = CARTESIAN_POINT ( 'NONE',  ( 2.499999999999947153, 2.500000000000000000, 3.737306695894644371 ) ) ;
#121924 = CARTESIAN_POINT ( 'NONE',  ( 8.149999999999923972, 12.50000000000000000, -6.213873640053564351 ) ) ;
#121925 = DIRECTION ( 'NONE',  ( -0.000000000000000000, -1.000000000000000000, -0.000000000000000000 ) ) ;
#121926 = DIRECTION ( 'NONE',  ( 0.000000000000000000, 0.000000000000000000, 1.000000000000000000 ) ) ;
#121927 = EDGE_CURVE ( 'NONE', #14735, #72399, #104560, .T. ) ;
#121928 = VERTEX_POINT ( 'NONE', #106495 ) ;
#121929 = CARTESIAN_POINT ( 'NONE',  ( -6.650000000000015454, 2.500000000000000000, 7.188010851410848723 ) ) ;
#121930 = ORIENTED_EDGE ( 'NONE', *, *, #7406, .T. ) ;
#121931 = ORIENTED_EDGE ( 'NONE', *, *, #56952, .F. ) ;
#121932 = VERTEX_POINT ( 'NONE', #124204 ) ;
#121933 = CARTESIAN_POINT ( 'NONE',  ( -3.469446951953614189E-14, 2.500000000000000000, -0.6928203230275519209 ) ) ;
#121934 = CIRCLE ( 'NONE', #55126, 0.06509327318403745899 ) ;
#121935 = VECTOR ( 'NONE', #42547, 1000.000000000000000 ) ;
#121936 = VERTEX_POINT ( 'NONE', #85561 ) ;
#121937 = ORIENTED_EDGE ( 'NONE', *, *, #114871, .F. ) ;
#121938 = ORIENTED_EDGE ( 'NONE', *, *, #65545, .T. ) ;
#121939 = SURFACE_STYLE_FILL_AREA ( #208 ) ;
#121941 = CARTESIAN_POINT ( 'NONE',  ( 9.349999999999919709, 12.50000000000000000, 1.818653347947321475 ) ) ;
#121940 = AXIS2_PLACEMENT_3D ( 'NONE', #76916, #16040, #57933 ) ;
#121942 = CARTESIAN_POINT ( 'NONE',  ( -8.950000000000006395, 12.50000000000000000, 6.906693963081109722 ) ) ;
#121944 = CARTESIAN_POINT ( 'NONE',  ( 8.349999999999919709, 12.50000000000000000, 6.495190528383297135 ) ) ;
#121943 = CONICAL_SURFACE ( 'NONE', #48891, 0.09999999999999982514, 0.003490658503988666988 ) ;
#121945 = DIRECTION ( 'NONE',  ( 0.000000000000000000, -0.9999939076577903929, 0.003490651415223739937 ) ) ;
#121946 = AXIS2_PLACEMENT_3D ( 'NONE', #100024, #90170, #40473 ) ;
#121947 = CARTESIAN_POINT ( 'NONE',  ( 6.449999999999930012, 12.50000000000000000, -1.883746621131363597 ) ) ;
#121948 = DIRECTION ( 'NONE',  ( -0.000000000000000000, -1.000000000000000000, -0.000000000000000000 ) ) ;
#121949 = CIRCLE ( 'NONE', #75965, 0.06509327318403745899 ) ;
#121951 = ORIENTED_EDGE ( 'NONE', *, *, #121641, .F. ) ;
#121950 = CONICAL_SURFACE ( 'NONE', #67649, 0.09999999999999982514, 0.003490658503988666988 ) ;
#121952 = CARTESIAN_POINT ( 'NONE',  ( -13.14999999999999147, 2.500000000000000000, -2.511473670974875727 ) ) ;
#121953 = ADVANCED_FACE ( 'NONE', ( #16793 ), #100621, .T. ) ;
#121954 = ORIENTED_EDGE ( 'NONE', *, *, #85160, .T. ) ;
#121955 = CARTESIAN_POINT ( 'NONE',  ( 7.299999999999927880, 2.500000000000000000, 3.883716857408421319 ) ) ;
#121956 = CONICAL_SURFACE ( 'NONE', #111480, 0.1000000000000002554, 0.003490658503988666988 ) ;
#121957 = ORIENTED_EDGE ( 'NONE', *, *, #125056, .T. ) ;
#121958 = AXIS2_PLACEMENT_3D ( 'NONE', #73473, #95067, #53850 ) ;
#121959 = PLANE ( 'NONE',  #44738 ) ;
#121960 = ORIENTED_EDGE ( 'NONE', *, *, #115363, .T. ) ;
#121961 = ADVANCED_FACE ( 'NONE', ( #75106 ), #25339, .T. ) ;
#121962 = CARTESIAN_POINT ( 'NONE',  ( 12.49999999999993605, 2.500000000000000000, -2.276824562219559311E-15 ) ) ;
#121963 = DIRECTION ( 'NONE',  ( 0.000000000000000000, -0.9999939076577903929, 0.003490651415223739937 ) ) ;
#121964 = ORIENTED_EDGE ( 'NONE', *, *, #50975, .T. ) ;
#121965 = EDGE_CURVE ( 'NONE', #2395, #12221, #94370, .T. ) ;
#121967 = ORIENTED_EDGE ( 'NONE', *, *, #82673, .T. ) ;
#121966 = ADVANCED_FACE ( 'NONE', ( #9586 ), #50020, .T. ) ;
#121968 = DIRECTION ( 'NONE',  ( 0.000000000000000000, 0.000000000000000000, 1.000000000000000000 ) ) ;
#121969 = DIRECTION ( 'NONE',  ( -0.000000000000000000, -1.000000000000000000, -0.000000000000000000 ) ) ;
#121970 = EDGE_CURVE ( 'NONE', #40079, #98189, #117570, .T. ) ;
#121971 = DIRECTION ( 'NONE',  ( -0.000000000000000000, 1.000000000000000000, -0.000000000000000000 ) ) ;
#121972 = EDGE_CURVE ( 'NONE', #124183, #1645, #45520, .T. ) ;
#121973 = DIRECTION ( 'NONE',  ( -0.000000000000000000, -1.000000000000000000, -0.000000000000000000 ) ) ;
#121974 = VECTOR ( 'NONE', #108151, 1000.000000000000000 ) ;
#121975 = CARTESIAN_POINT ( 'NONE',  ( -8.100000000000013856, 12.50000000000000000, -3.918623584224389056 ) ) ;
#121976 = ORIENTED_EDGE ( 'NONE', *, *, #14099, .F. ) ;
#121977 = CARTESIAN_POINT ( 'NONE',  ( 2.500000000000001332, -2.392226903609812272, 9.521986658763283984 ) ) ;
#121978 = ADVANCED_FACE ( 'NONE', ( #67852 ), #114738, .T. ) ;
#121979 = CIRCLE ( 'NONE', #109450, 0.06509327318403745899 ) ;
#121980 = VERTEX_POINT ( 'NONE', #99267 ) ;
#121981 = EDGE_CURVE ( 'NONE', #71812, #35395, #98584, .T. ) ;
#121982 = FACE_OUTER_BOUND ( 'NONE', #77629, .T. ) ;
#121983 = PLANE ( 'NONE',  #91838 ) ;
#121984 = CONICAL_SURFACE ( 'NONE', #69744, 0.09999999999999982514, 0.003490658503988666988 ) ;
#121985 = EDGE_CURVE ( 'NONE', #56742, #27176, #80266, .T. ) ;
#121986 = CARTESIAN_POINT ( 'NONE',  ( 3.099999999999945022, 12.50000000000000000, -0.3464101615137783474 ) ) ;
#121987 = FACE_OUTER_BOUND ( 'NONE', #116634, .T. ) ;
#121988 = FACE_OUTER_BOUND ( 'NONE', #72500, .T. ) ;
#121989 = AXIS2_PLACEMENT_3D ( 'NONE', #51679, #13659, #122354 ) ;
#121991 = VECTOR ( 'NONE', #48876, 1000.000000000000000 ) ;
#121990 = DIRECTION ( 'NONE',  ( -4.274815082592931898E-19, -0.9999939076577903929, -0.003490651415223739937 ) ) ;
#121992 = ORIENTED_EDGE ( 'NONE', *, *, #45709, .F. ) ;
#121993 = AXIS2_PLACEMENT_3D ( 'NONE', #6930, #86807, #48837 ) ;
#121994 = AXIS2_PLACEMENT_3D ( 'NONE', #38451, #78373, #118273 ) ;
#121995 = CARTESIAN_POINT ( 'NONE',  ( 4.599999999999940137, 2.500000000000000000, -4.922947341949753586 ) ) ;
#121996 = DIRECTION ( 'NONE',  ( 0.000000000000000000, 0.000000000000000000, 1.000000000000000000 ) ) ;
#121997 = DIRECTION ( 'NONE',  ( -0.000000000000000000, 1.000000000000000000, -0.000000000000000000 ) ) ;
#121998 = EDGE_LOOP ( 'NONE', ( #88600, #54566, #13279, #39825 ) ) ;
#121999 = AXIS2_PLACEMENT_3D ( 'NONE', #15470, #75676, #16744 ) ;
#122000 = EDGE_LOOP ( 'NONE', ( #113528, #127447 ) ) ;
#122001 = DIRECTION ( 'NONE',  ( 0.000000000000000000, 1.000000000000000000, 0.000000000000000000 ) ) ;
#122002 = VERTEX_POINT ( 'NONE', #57399 ) ;
#122003 = CIRCLE ( 'NONE', #21657, 0.06509327318403745899 ) ;
#122005 = ORIENTED_EDGE ( 'NONE', *, *, #74986, .T. ) ;
#122004 = CIRCLE ( 'NONE', #94904, 0.06509327318403745899 ) ;
#122006 = CIRCLE ( 'NONE', #119945, 0.1000000000000000056 ) ;
#122007 = DIRECTION ( 'NONE',  ( -0.000000000000000000, 1.000000000000000000, -0.000000000000000000 ) ) ;
#122009 = VERTEX_POINT ( 'NONE', #97957 ) ;
#122008 = VECTOR ( 'NONE', #33667, 1000.000000000000000 ) ;
#122010 = DIRECTION ( 'NONE',  ( 0.000000000000000000, 0.000000000000000000, 1.000000000000000000 ) ) ;
#122011 = FACE_OUTER_BOUND ( 'NONE', #6423, .T. ) ;
#122012 = CARTESIAN_POINT ( 'NONE',  ( 17.84432265422787722, 2.533187527836262554, 5.021315468706709417 ) ) ;
#122013 = CIRCLE ( 'NONE', #109485, 0.1000000000000000056 ) ;
#122014 = EDGE_LOOP ( 'NONE', ( #44381, #105444 ) ) ;
#122015 = DIRECTION ( 'NONE',  ( -4.274815082592931898E-19, -0.9999939076577903929, -0.003490651415223739937 ) ) ;
#122016 = CARTESIAN_POINT ( 'NONE',  ( 12.29999999999990301, 2.500000000000000000, -0.2464101615137782308 ) ) ;
#122017 = ADVANCED_FACE ( 'NONE', ( #97321 ), #7635, .T. ) ;
#122018 = ORIENTED_EDGE ( 'NONE', *, *, #117414, .T. ) ;
#122019 = EDGE_CURVE ( 'NONE', #77678, #39357, #12332, .T. ) ;
#122020 = ORIENTED_EDGE ( 'NONE', *, *, #45192, .T. ) ;
#122021 = ADVANCED_FACE ( 'NONE', ( #68495 ), #112694, .T. ) ;
#122022 = VERTEX_POINT ( 'NONE', #20062 ) ;
#122023 = DIRECTION ( 'NONE',  ( 0.000000000000000000, 1.000000000000000000, 0.000000000000000000 ) ) ;
#122024 = DIRECTION ( 'NONE',  ( 0.000000000000000000, 1.000000000000000000, 0.000000000000000000 ) ) ;
#122026 = CARTESIAN_POINT ( 'NONE',  ( -10.00000000000000711, 2.500000000000000000, -3.637306695894645614 ) ) ;
#122025 = CONICAL_SURFACE ( 'NONE', #40571, 0.1000000000000002554, 0.003490658503988666988 ) ;
#122027 = CIRCLE ( 'NONE', #109504, 0.1000000000000000472 ) ;
#122028 = FACE_BOUND ( 'NONE', #39648, .T. ) ;
#122029 = ORIENTED_EDGE ( 'NONE', *, *, #65033, .F. ) ;
#122030 = DIRECTION ( 'NONE',  ( 0.000000000000000000, 1.000000000000000000, 0.000000000000000000 ) ) ;
#122031 = CARTESIAN_POINT ( 'NONE',  ( -1.050000000000038680, 12.50000000000000000, 6.841600689897072485 ) ) ;
#122032 = ORIENTED_EDGE ( 'NONE', *, *, #49969, .F. ) ;
#122033 = EDGE_CURVE ( 'NONE', #36138, #11513, #93823, .T. ) ;
#122034 = CARTESIAN_POINT ( 'NONE',  ( -2.500000000000032863, 2.500000000000000000, 5.022947341949748790 ) ) ;
#122036 = CARTESIAN_POINT ( 'NONE',  ( -7.100000000000013856, 12.50000000000000000, 5.022947341949748790 ) ) ;
#122035 = AXIS2_PLACEMENT_3D ( 'NONE', #129271, #39603, #79507 ) ;
#122037 = VECTOR ( 'NONE', #99995, 1000.000000000000000 ) ;
#122038 = CIRCLE ( 'NONE', #67642, 0.06509327318403745899 ) ;
#122040 = CONICAL_SURFACE ( 'NONE', #103257, 0.09999999999999982514, 0.003490658503988666988 ) ;
#122039 = PLANE ( 'NONE',  #67426 ) ;
#122041 = CARTESIAN_POINT ( 'NONE',  ( -0.6500000000000403233, 2.500000000000000000, 6.148780366869520009 ) ) ;
#122042 = CARTESIAN_POINT ( 'NONE',  ( 11.69999999999990870, 2.500000000000000000, 4.330127018922196314 ) ) ;
#122043 = FACE_OUTER_BOUND ( 'NONE', #32221, .T. ) ;
#122044 = DIRECTION ( 'NONE',  ( 0.000000000000000000, -0.9999939076577903929, 0.003490651415223739937 ) ) ;
#122045 = AXIS2_PLACEMENT_3D ( 'NONE', #116596, #47236, #66207 ) ;
#122046 = VECTOR ( 'NONE', #2232, 1000.000000000000000 ) ;
#122047 = ORIENTED_EDGE ( 'NONE', *, *, #61431, .F. ) ;
#122048 = EDGE_LOOP ( 'NONE', ( #124295, #2186, #69441, #15371 ) ) ;
#122049 = ORIENTED_EDGE ( 'NONE', *, *, #26019, .F. ) ;
#122050 = ORIENTED_EDGE ( 'NONE', *, *, #72324, .T. ) ;
#122051 = DIRECTION ( 'NONE',  ( 0.000000000000000000, 0.000000000000000000, 1.000000000000000000 ) ) ;
#122052 = CARTESIAN_POINT ( 'NONE',  ( -1.250000000000035749, 12.50000000000000000, -7.122917578226816815 ) ) ;
#122053 = AXIS2_PLACEMENT_3D ( 'NONE', #83166, #63522, #3938 ) ;
#122054 = DIRECTION ( 'NONE',  ( 0.000000000000000000, 1.000000000000000000, 0.000000000000000000 ) ) ;
#122055 = ORIENTED_EDGE ( 'NONE', *, *, #2588, .F. ) ;
#122056 = FACE_BOUND ( 'NONE', #111071, .T. ) ;
#122057 = EDGE_CURVE ( 'NONE', #46303, #48905, #39721, .T. ) ;
#122058 = CARTESIAN_POINT ( 'NONE',  ( -13.14999999999999147, 12.50000000000000000, 2.511473670974877503 ) ) ;
#122059 = DIRECTION ( 'NONE',  ( 0.000000000000000000, -0.000000000000000000, 1.000000000000000000 ) ) ;
#122060 = LINE ( 'NONE', #61853, #15685 ) ;
#122061 = CARTESIAN_POINT ( 'NONE',  ( -9.200000000000009948, 2.500000000000000000, -4.330127018922197202 ) ) ;
#122062 = CARTESIAN_POINT ( 'NONE',  ( 11.64999999999990443, 12.50000000000000000, 1.472243186433545459 ) ) ;
#122063 = DIRECTION ( 'NONE',  ( 0.000000000000000000, 0.000000000000000000, 1.000000000000000000 ) ) ;
#122065 = DIRECTION ( 'NONE',  ( 0.000000000000000000, 1.000000000000000000, 0.000000000000000000 ) ) ;
#122064 =( BOUNDED_CURVE ( )  B_SPLINE_CURVE ( 2, ( #61824, #11412, #22548, #40238, #29769, #72288, #109628 ),
 .UNSPECIFIED., .F., .T. ) 
 B_SPLINE_CURVE_WITH_KNOTS ( ( 3, 2, 2, 3 ),
 ( 0.9285714285714292693, 0.9523809523809527722, 0.9761904761904763861, 1.000000000000000000 ),
 .UNSPECIFIED. ) 
 CURVE ( )  GEOMETRIC_REPRESENTATION_ITEM ( )  RATIONAL_B_SPLINE_CURVE ( ( 0.9999999999999962252, 0.8660254037844424824, 1.000000000000000000, 0.8660254037844387076, 1.000000000000000000, 0.8660254037844387076, 1.000000000000000000 ) ) 
 REPRESENTATION_ITEM ( '' )  );
#122066 = DIRECTION ( 'NONE',  ( -0.000000000000000000, 1.000000000000000000, -0.000000000000000000 ) ) ;
#122067 = CARTESIAN_POINT ( 'NONE',  ( 1.658312395177699017, -2.500000000000000444, -5.000000000000004441 ) ) ;
#122068 = AXIS2_PLACEMENT_3D ( 'NONE', #54386, #91741, #81909 ) ;
#122069 = ORIENTED_EDGE ( 'NONE', *, *, #22038, .F. ) ;
#122070 = ORIENTED_EDGE ( 'NONE', *, *, #127538, .F. ) ;
#122071 = EDGE_LOOP ( 'NONE', ( #55052, #98645 ) ) ;
#122072 = EDGE_CURVE ( 'NONE', #59946, #37252, #104287, .T. ) ;
#122073 = ORIENTED_EDGE ( 'NONE', *, *, #94102, .F. ) ;
#122074 = ORIENTED_EDGE ( 'NONE', *, *, #45305, .F. ) ;
#122075 = EDGE_LOOP ( 'NONE', ( #15150, #41778 ) ) ;
#122076 = DIRECTION ( 'NONE',  ( 0.000000000000000000, 0.000000000000000000, -1.000000000000000000 ) ) ;
#122077 = ORIENTED_EDGE ( 'NONE', *, *, #2706, .F. ) ;
#122078 = ORIENTED_EDGE ( 'NONE', *, *, #21353, .F. ) ;
#122079 = VECTOR ( 'NONE', #29324, 1000.000000000000000 ) ;
#122080 = AXIS2_PLACEMENT_3D ( 'NONE', #65495, #5913, #26234 ) ;
#122081 = DIRECTION ( 'NONE',  ( 0.000000000000000000, 0.000000000000000000, -1.000000000000000000 ) ) ;
#122082 = DIRECTION ( 'NONE',  ( 0.000000000000000000, 1.000000000000000000, 0.000000000000000000 ) ) ;
#122083 = DIRECTION ( 'NONE',  ( 0.000000000000000000, -0.000000000000000000, 1.000000000000000000 ) ) ;
#122084 = FACE_OUTER_BOUND ( 'NONE', #46881, .T. ) ;
#122085 = EDGE_CURVE ( 'NONE', #79702, #112590, #72982, .T. ) ;
#122086 = AXIS2_PLACEMENT_3D ( 'NONE', #54874, #16857, #75802 ) ;
#122087 = VERTEX_POINT ( 'NONE', #90061 ) ;
#122088 = DIRECTION ( 'NONE',  ( -0.000000000000000000, -1.000000000000000000, -0.000000000000000000 ) ) ;
#122089 = CIRCLE ( 'NONE', #105356, 0.1000000000000002554 ) ;
#122090 = EDGE_LOOP ( 'NONE', ( #110076, #78040 ) ) ;
#122091 = AXIS2_PLACEMENT_3D ( 'NONE', #112332, #100563, #50832 ) ;
#122092 = ORIENTED_EDGE ( 'NONE', *, *, #4062, .F. ) ;
#122093 = CARTESIAN_POINT ( 'NONE',  ( 0.8499999999999527933, 2.500000000000000000, 7.288010851410849256 ) ) ;
#122095 = ADVANCED_FACE ( 'NONE', ( #39072 ), #87481, .T. ) ;
#122094 = DIRECTION ( 'NONE',  ( 0.000000000000000000, 1.000000000000000000, 0.000000000000000000 ) ) ;
#122096 = ORIENTED_EDGE ( 'NONE', *, *, #39824, .F. ) ;
#122097 = VERTEX_POINT ( 'NONE', #118245 ) ;
#122098 = DIRECTION ( 'NONE',  ( 0.000000000000000000, 1.000000000000000000, 0.000000000000000000 ) ) ;
#122100 = AXIS2_PLACEMENT_3D ( 'NONE', #109454, #108792, #19792 ) ;
#122099 = PLANE ( 'NONE',  #49579 ) ;
#122102 = CIRCLE ( 'NONE', #48945, 0.1000000000000002554 ) ;
#122101 = DIRECTION ( 'NONE',  ( 0.000000000000000000, 0.000000000000000000, -1.000000000000000000 ) ) ;
#122103 = AXIS2_PLACEMENT_3D ( 'NONE', #97696, #59078, #47975 ) ;
#122104 = CARTESIAN_POINT ( 'NONE',  ( -9.600000000000008527, 12.50000000000000000, -3.637306695894645614 ) ) ;
#122105 = LINE ( 'NONE', #120805, #56533 ) ;
#122106 = CIRCLE ( 'NONE', #119949, 0.1000000000000002554 ) ;
#122107 = EDGE_LOOP ( 'NONE', ( #91168, #51589 ) ) ;
#122108 = AXIS2_PLACEMENT_3D ( 'NONE', #31238, #22708, #71798 ) ;
#122109 = CARTESIAN_POINT ( 'NONE',  ( 1.049999999999952971, 2.500000000000000000, 6.048780366869521252 ) ) ;
#122110 = EDGE_LOOP ( 'NONE', ( #78556, #62364, #90132, #124514 ) ) ;
#122111 = CARTESIAN_POINT ( 'NONE',  ( 87.50000000000002842, 7.032605354647524010, 2.693424153406289712 ) ) ;
#122112 = EDGE_CURVE ( 'NONE', #120532, #62968, #127431, .T. ) ;
#122113 = CARTESIAN_POINT ( 'NONE',  ( 4.799999999999934097, 2.500000000000000000, 4.776537180435972196 ) ) ;
#122114 = CARTESIAN_POINT ( 'NONE',  ( 8.749999999999921840, 2.500000000000000000, 2.757883832488649656 ) ) ;
#122115 = CARTESIAN_POINT ( 'NONE',  ( 15.19999999999989271, 2.500000000000000000, -0.2464101615137783419 ) ) ;
#122116 = DIRECTION ( 'NONE',  ( 0.000000000000000000, 0.000000000000000000, -1.000000000000000000 ) ) ;
#122117 = EDGE_LOOP ( 'NONE', ( #79335, #2065, #85997, #121530 ) ) ;
#122118 = EDGE_CURVE ( 'NONE', #64939, #9837, #19386, .T. ) ;
#122119 = DIRECTION ( 'NONE',  ( 0.000000000000000000, -0.9999939076577903929, 0.003490651415223739937 ) ) ;
#122121 = DIRECTION ( 'NONE',  ( 0.000000000000000000, -0.000000000000000000, 1.000000000000000000 ) ) ;
#122120 = VECTOR ( 'NONE', #127438, 1000.000000000000000 ) ;
#122122 = ORIENTED_EDGE ( 'NONE', *, *, #4002, .F. ) ;
#122123 = ORIENTED_EDGE ( 'NONE', *, *, #65311, .F. ) ;
#122124 = AXIS2_PLACEMENT_3D ( 'NONE', #61912, #103105, #33722 ) ;
#122125 = ADVANCED_FACE ( 'NONE', ( #92656 ), #14458, .T. ) ;
#122126 = CIRCLE ( 'NONE', #117898, 0.06509327318403741736 ) ;
#122128 = ORIENTED_EDGE ( 'NONE', *, *, #89257, .T. ) ;
#122127 = EDGE_CURVE ( 'NONE', #24551, #12644, #6062, .T. ) ;
#122129 = CARTESIAN_POINT ( 'NONE',  ( 17.50000000000000000, 0.9166666666666684060, 3.432456362931491700 ) ) ;
#122130 = CARTESIAN_POINT ( 'NONE',  ( 1.249999999999952038, 2.500000000000000000, -1.472243186433550122 ) ) ;
#122131 = ADVANCED_FACE ( 'NONE', ( #32480 ), #83497, .T. ) ;
#122132 = CARTESIAN_POINT ( 'NONE',  ( 186.4843750003414016, -8.734944146203032389, -1.604583208406768146E-15 ) ) ;
#122133 = EDGE_CURVE ( 'NONE', #63089, #25747, #29088, .T. ) ;
#122134 = CARTESIAN_POINT ( 'NONE',  ( -0.4000000000000396572, 2.500000000000000000, 4.430127018922196847 ) ) ;
#122135 = DIRECTION ( 'NONE',  ( 0.000000000000000000, 0.000000000000000000, -1.000000000000000000 ) ) ;
#122136 = AXIS2_PLACEMENT_3D ( 'NONE', #87215, #105588, #35562 ) ;
#122137 = AXIS2_PLACEMENT_3D ( 'NONE', #12790, #73022, #104414 ) ;
#122138 = CARTESIAN_POINT ( 'NONE',  ( 5.849999999999933031, 2.500000000000000000, -1.372243186433550033 ) ) ;
#122139 = VECTOR ( 'NONE', #31050, 1000.000000000000000 ) ;
#122141 = VECTOR ( 'NONE', #30505, 1000.000000000000000 ) ;
#122140 = CARTESIAN_POINT ( 'NONE',  ( 7.949999999999925571, 12.50000000000000000, -6.495190528383302464 ) ) ;
#122142 = ADVANCED_FACE ( 'NONE', ( #93305 ), #24863, .T. ) ;
#122143 = ADVANCED_FACE ( 'NONE', ( #122763 ), #63198, .T. ) ;
#122144 = EDGE_CURVE ( 'NONE', #11888, #46085, #75037, .T. ) ;
#122145 = EDGE_CURVE ( 'NONE', #181, #104766, #13438, .T. ) ;
#122146 = CIRCLE ( 'NONE', #69999, 0.1000000000000002554 ) ;
#122147 = CARTESIAN_POINT ( 'NONE',  ( 2.899999999999946620, 12.50000000000000000, 0.6928203230275494784 ) ) ;
#122148 = CIRCLE ( 'NONE', #3008, 0.06509327318403745899 ) ;
#122149 = EDGE_CURVE ( 'NONE', #62966, #70666, #73017, .T. ) ;
#122150 = ORIENTED_EDGE ( 'NONE', *, *, #32448, .F. ) ;
#122151 = DIRECTION ( 'NONE',  ( 0.000000000000000000, 0.000000000000000000, 1.000000000000000000 ) ) ;
#122152 = AXIS2_PLACEMENT_3D ( 'NONE', #80432, #79149, #100688 ) ;
#122153 = DIRECTION ( 'NONE',  ( -0.000000000000000000, 1.000000000000000000, -0.000000000000000000 ) ) ;
#122154 = DIRECTION ( 'NONE',  ( 0.000000000000000000, 0.000000000000000000, 1.000000000000000000 ) ) ;
#122155 = DIRECTION ( 'NONE',  ( 0.000000000000000000, 1.000000000000000000, 0.000000000000000000 ) ) ;
#122156 = ADVANCED_FACE ( 'NONE', ( #110357 ), #43659, .T. ) ;
#122157 = ORIENTED_EDGE ( 'NONE', *, *, #47155, .T. ) ;
#122158 = LINE ( 'NONE', #32497, #46737 ) ;
#122159 = FACE_OUTER_BOUND ( 'NONE', #121017, .T. ) ;
#122161 = ORIENTED_EDGE ( 'NONE', *, *, #24505, .T. ) ;
#122160 = CARTESIAN_POINT ( 'NONE',  ( 0.7999999999999553024, 2.500000000000000000, -4.330127018922201643 ) ) ;
#122162 = AXIS2_PLACEMENT_3D ( 'NONE', #127434, #27281, #67179 ) ;
#122163 = ORIENTED_EDGE ( 'NONE', *, *, #34732, .T. ) ;
#122164 = LINE ( 'NONE', #90751, #7036 ) ;
#122165 = ORIENTED_EDGE ( 'NONE', *, *, #46463, .F. ) ;
#122166 = VERTEX_POINT ( 'NONE', #20700 ) ;
#122167 = DIRECTION ( 'NONE',  ( 0.000000000000000000, 1.000000000000000000, 0.000000000000000000 ) ) ;
#122168 = CARTESIAN_POINT ( 'NONE',  ( -10.00000000000000533, 2.500000000000000000, -5.022947341949749678 ) ) ;
#122169 = CARTESIAN_POINT ( 'NONE',  ( 7.699999999999923794, 2.500000000000000000, -3.883716857408426648 ) ) ;
#122170 = CARTESIAN_POINT ( 'NONE',  ( -14.59999999999998366, 12.50000000000000000, -0.6928203230275520319 ) ) ;
#122171 = AXIS2_PLACEMENT_3D ( 'NONE', #42514, #62150, #3222 ) ;
#122172 = ORIENTED_EDGE ( 'NONE', *, *, #87055, .F. ) ;
#122173 = CARTESIAN_POINT ( 'NONE',  ( -2.300000000000032685, 12.50000000000000000, -4.676537180435978769 ) ) ;
#122174 = ORIENTED_EDGE ( 'NONE', *, *, #36442, .T. ) ;
#122175 = DIRECTION ( 'NONE',  ( 0.000000000000000000, 0.000000000000000000, 1.000000000000000000 ) ) ;
#122176 = CARTESIAN_POINT ( 'NONE',  ( -5.400000000000019895, 12.50000000000000000, 4.395220292106234439 ) ) ;
#122177 = VERTEX_POINT ( 'NONE', #50804 ) ;
#122178 = EDGE_CURVE ( 'NONE', #18500, #107528, #60637, .T. ) ;
#122179 = ORIENTED_EDGE ( 'NONE', *, *, #86344, .T. ) ;
#122181 = EDGE_LOOP ( 'NONE', ( #3020, #121976, #116699, #103195 ) ) ;
#122180 = EDGE_CURVE ( 'NONE', #70884, #108643, #116788, .T. ) ;
#122182 = VERTEX_POINT ( 'NONE', #94576 ) ;
#122183 = DIRECTION ( 'NONE',  ( 0.000000000000000000, 0.000000000000000000, 1.000000000000000000 ) ) ;
#122184 = CARTESIAN_POINT ( 'NONE',  ( 14.66596006039175748, 2.500000000000513811, 7.515560524214964566 ) ) ;
#122185 = CARTESIAN_POINT ( 'NONE',  ( -6.900000000000015454, 2.500000000000000000, 4.776537180435972196 ) ) ;
#122186 = FACE_BOUND ( 'NONE', #15668, .T. ) ;
#122187 = ORIENTED_EDGE ( 'NONE', *, *, #125677, .T. ) ;
#122188 = CARTESIAN_POINT ( 'NONE',  ( 184.2395833340161175, 4.445597072760117285, 7.699999999999999289 ) ) ;
#122189 = DIRECTION ( 'NONE',  ( -0.000000000000000000, 1.000000000000000000, -0.000000000000000000 ) ) ;
#122190 = CARTESIAN_POINT ( 'NONE',  ( 4.599999999999938360, 12.50000000000000000, 0.06509327318403515528 ) ) ;
#122191 = ADVANCED_FACE ( 'NONE', ( #95242 ), #86032, .T. ) ;
#122192 = VECTOR ( 'NONE', #54391, 1000.000000000000000 ) ;
#122193 = AXIS2_PLACEMENT_3D ( 'NONE', #116239, #26586, #75038 ) ;
#122194 = FACE_OUTER_BOUND ( 'NONE', #44510, .T. ) ;
#122195 = DIRECTION ( 'NONE',  ( 0.000000000000000000, 0.000000000000000000, -1.000000000000000000 ) ) ;
#122196 = AXIS2_PLACEMENT_3D ( 'NONE', #22420, #101613, #119957 ) ;
#122197 = CARTESIAN_POINT ( 'NONE',  ( 13.34999999999989662, 12.50000000000000000, -1.407149913249512663 ) ) ;
#122198 = AXIS2_PLACEMENT_3D ( 'NONE', #116210, #6881, #63906 ) ;
#122199 = CARTESIAN_POINT ( 'NONE',  ( 9.149999999999918643, 2.500000000000000000, -6.495190528383302464 ) ) ;
#122200 = ORIENTED_EDGE ( 'NONE', *, *, #49089, .F. ) ;
#122201 = VERTEX_POINT ( 'NONE', #36339 ) ;
#122202 = ORIENTED_EDGE ( 'NONE', *, *, #21939, .F. ) ;
#122203 = ORIENTED_EDGE ( 'NONE', *, *, #118860, .T. ) ;
#122204 = ORIENTED_EDGE ( 'NONE', *, *, #56333, .F. ) ;
#122205 = FACE_OUTER_BOUND ( 'NONE', #97110, .T. ) ;
#122206 = CARTESIAN_POINT ( 'NONE',  ( -7.100000000000013856, 12.50000000000000000, 5.022947341949748790 ) ) ;
#122207 = EDGE_LOOP ( 'NONE', ( #119693, #5643 ) ) ;
#122208 = FACE_BOUND ( 'NONE', #11766, .T. ) ;
#122209 = FACE_OUTER_BOUND ( 'NONE', #8895, .T. ) ;
#122210 = AXIS2_PLACEMENT_3D ( 'NONE', #10386, #98754, #91531 ) ;
#122211 = CIRCLE ( 'NONE', #78310, 0.06509327318403745899 ) ;
#122213 = EDGE_LOOP ( 'NONE', ( #112721, #95319, #13830, #115229 ) ) ;
#122212 = AXIS2_PLACEMENT_3D ( 'NONE', #125958, #105025, #26490 ) ;
#122214 = AXIS2_PLACEMENT_3D ( 'NONE', #42738, #4056, #11948 ) ;
#122215 = CARTESIAN_POINT ( 'NONE',  ( 4.599999999999938360, 12.50000000000000000, -0.6928203230275541413 ) ) ;
#122216 = CARTESIAN_POINT ( 'NONE',  ( -13.34999999999999076, 2.500000000000000000, -2.165063509461099489 ) ) ;
#122217 = DIRECTION ( 'NONE',  ( 0.000000000000000000, 0.000000000000000000, 1.000000000000000000 ) ) ;
#122218 = EDGE_LOOP ( 'NONE', ( #63079, #38759 ) ) ;
#122219 = DIRECTION ( 'NONE',  ( 0.000000000000000000, 0.000000000000000000, 1.000000000000000000 ) ) ;
#122220 = EDGE_CURVE ( 'NONE', #102068, #25999, #121006, .T. ) ;
#122221 = AXIS2_PLACEMENT_3D ( 'NONE', #3770, #1826, #124191 ) ;
#122222 = VERTEX_POINT ( 'NONE', #64478 ) ;
#122223 = AXIS2_PLACEMENT_3D ( 'NONE', #66818, #94356, #34828 ) ;
#122224 = AXIS2_PLACEMENT_3D ( 'NONE', #114095, #63711, #64976 ) ;
#122225 = ORIENTED_EDGE ( 'NONE', *, *, #128228, .F. ) ;
#122226 = ORIENTED_EDGE ( 'NONE', *, *, #230, .T. ) ;
#122227 = DIRECTION ( 'NONE',  ( 0.000000000000000000, 0.000000000000000000, 1.000000000000000000 ) ) ;
#122228 = CIRCLE ( 'NONE', #72060, 0.06509327318403745899 ) ;
#122229 = DIRECTION ( 'NONE',  ( 0.000000000000000000, -0.000000000000000000, 1.000000000000000000 ) ) ;
#122230 = FACE_OUTER_BOUND ( 'NONE', #54118, .T. ) ;
#122231 = ORIENTED_EDGE ( 'NONE', *, *, #23284, .T. ) ;
#122232 = DIRECTION ( 'NONE',  ( 0.000000000000000000, 1.000000000000000000, 0.000000000000000000 ) ) ;
#122233 = AXIS2_PLACEMENT_3D ( 'NONE', #23413, #104561, #5062 ) ;
#122234 = AXIS2_PLACEMENT_3D ( 'NONE', #54269, #24163, #14947 ) ;
#122235 = DIRECTION ( 'NONE',  ( -0.000000000000000000, 1.000000000000000000, -0.000000000000000000 ) ) ;
#122236 = DIRECTION ( 'NONE',  ( -0.000000000000000000, -1.000000000000000000, -0.000000000000000000 ) ) ;
#122237 = DIRECTION ( 'NONE',  ( 0.000000000000000000, 0.000000000000000000, -1.000000000000000000 ) ) ;
#122238 = CARTESIAN_POINT ( 'NONE',  ( 186.6562500006828316, 8.891194145520236347, 5.444286225454521982E-16 ) ) ;
#122240 = ORIENTED_EDGE ( 'NONE', *, *, #11897, .T. ) ;
#122239 = AXIS2_PLACEMENT_3D ( 'NONE', #103931, #103292, #92832 ) ;
#122241 = EDGE_CURVE ( 'NONE', #83886, #94318, #4901, .T. ) ;
#122242 = FACE_OUTER_BOUND ( 'NONE', #121310, .T. ) ;
#122243 = EDGE_CURVE ( 'NONE', #23306, #41996, #81298, .T. ) ;
#122244 = ORIENTED_EDGE ( 'NONE', *, *, #6011, .T. ) ;
#122245 = DIRECTION ( 'NONE',  ( 0.000000000000000000, -0.000000000000000000, 1.000000000000000000 ) ) ;
#122246 = VERTEX_POINT ( 'NONE', #74954 ) ;
#122247 = ORIENTED_EDGE ( 'NONE', *, *, #120225, .F. ) ;
#122248 = DIRECTION ( 'NONE',  ( 0.000000000000000000, 0.000000000000000000, 1.000000000000000000 ) ) ;
#122249 = CARTESIAN_POINT ( 'NONE',  ( 12.09999999999990550, 2.500000000000000000, 3.637306695894644726 ) ) ;
#122250 = CARTESIAN_POINT ( 'NONE',  ( -9.999999999999971578, 12.50000000000000000, -4.265033745738159965 ) ) ;
#122252 = EDGE_CURVE ( 'NONE', #79726, #35730, #91754, .T. ) ;
#122251 = CARTESIAN_POINT ( 'NONE',  ( -13.34999999999999076, 2.500000000000000000, -1.472243186433547901 ) ) ;
#122253 = CARTESIAN_POINT ( 'NONE',  ( 3.349999999999945466, 12.50000000000000000, -6.430097255199264339 ) ) ;
#122254 = CONICAL_SURFACE ( 'NONE', #11423, 0.09999999999999982514, 0.003490658503988666988 ) ;
#122255 = EDGE_LOOP ( 'NONE', ( #40778, #15171, #51508, #72284 ) ) ;
#122256 = ORIENTED_EDGE ( 'NONE', *, *, #61565, .F. ) ;
#122257 = DIRECTION ( 'NONE',  ( 0.000000000000000000, -0.000000000000000000, 1.000000000000000000 ) ) ;
#122258 = FACE_OUTER_BOUND ( 'NONE', #8388, .T. ) ;
#122259 = DIRECTION ( 'NONE',  ( -0.000000000000000000, -1.000000000000000000, -0.000000000000000000 ) ) ;
#122260 = ORIENTED_EDGE ( 'NONE', *, *, #11237, .F. ) ;
#122261 = VERTEX_POINT ( 'NONE', #105707 ) ;
#122262 = DIRECTION ( 'NONE',  ( 0.000000000000000000, -0.000000000000000000, 1.000000000000000000 ) ) ;
#122263 = CIRCLE ( 'NONE', #49021, 0.06509327318403745899 ) ;
#122264 = VERTEX_POINT ( 'NONE', #103773 ) ;
#122265 = DIRECTION ( 'NONE',  ( 0.000000000000000000, 1.000000000000000000, 0.000000000000000000 ) ) ;
#122267 = CIRCLE ( 'NONE', #107677, 0.09999999999999982514 ) ;
#122266 = CARTESIAN_POINT ( 'NONE',  ( -0.6000000000000383915, 2.500000000000000000, -3.983716857408426293 ) ) ;
#122268 = LINE ( 'NONE', #11653, #109607 ) ;
#122269 = ORIENTED_EDGE ( 'NONE', *, *, #69248, .F. ) ;
#122270 = DIRECTION ( 'NONE',  ( -0.000000000000000000, -1.000000000000000000, -0.000000000000000000 ) ) ;
#122271 = DIRECTION ( 'NONE',  ( -4.274815082592931898E-19, -0.9999939076577903929, -0.003490651415223739937 ) ) ;
#122272 = CARTESIAN_POINT ( 'NONE',  ( -7.500000000000001776, 1.500000000000000000, 1.734723475976807094E-15 ) ) ;
#122273 = CARTESIAN_POINT ( 'NONE',  ( -15.19999999999998330, 12.50000000000000000, 0.3464101615137758494 ) ) ;
#122274 = PLANE ( 'NONE',  #72952 ) ;
#122275 = EDGE_LOOP ( 'NONE', ( #32400, #126879, #88664, #32811 ) ) ;
#122276 = AXIS2_PLACEMENT_3D ( 'NONE', #102987, #5430, #54524 ) ;
#122277 = ADVANCED_FACE ( 'NONE', ( #55317 ), #34406, .F. ) ;
#122278 = CARTESIAN_POINT ( 'NONE',  ( 9.149999999999916866, 12.50000000000000000, 7.188010851410848723 ) ) ;
#122280 = AXIS2_PLACEMENT_3D ( 'NONE', #35288, #66016, #116394 ) ;
#122279 = DIRECTION ( 'NONE',  ( 0.000000000000000000, 0.000000000000000000, -1.000000000000000000 ) ) ;
#122281 = VERTEX_POINT ( 'NONE', #104410 ) ;
#122282 = ORIENTED_EDGE ( 'NONE', *, *, #43960, .F. ) ;
#122283 = EDGE_CURVE ( 'NONE', #124086, #22468, #108473, .T. ) ;
#122284 = CARTESIAN_POINT ( 'NONE',  ( 187.0052083336747444, -6.551208109652278289, 3.782341765624995134 ) ) ;
#122285 = DIRECTION ( 'NONE',  ( -0.000000000000000000, -1.000000000000000000, -0.000000000000000000 ) ) ;
#122286 = DIRECTION ( 'NONE',  ( -0.000000000000000000, 1.000000000000000000, -0.000000000000000000 ) ) ;
#122287 = EDGE_CURVE ( 'NONE', #125928, #95328, #33292, .T. ) ;
#122288 = CARTESIAN_POINT ( 'NONE',  ( -10.85000000000000142, 2.500000000000000000, -2.857883832488649745 ) ) ;
#122289 = CARTESIAN_POINT ( 'NONE',  ( 4.399999999999939071, 2.500000000000000000, 0.4464101615137736623 ) ) ;
#122290 = AXIS2_PLACEMENT_3D ( 'NONE', #97539, #127019, #37351 ) ;
#122291 = CARTESIAN_POINT ( 'NONE',  ( 5.849999999999933920, 12.50000000000000000, 5.802370205355744659 ) ) ;
#122292 = CIRCLE ( 'NONE', #86758, 0.09999999999999982514 ) ;
#122293 = CARTESIAN_POINT ( 'NONE',  ( 2.699999999999946443, 12.50000000000000000, -4.048810130592463530 ) ) ;
#122294 = LINE ( 'NONE', #11016, #49830 ) ;
#122295 = EDGE_CURVE ( 'NONE', #58087, #96104, #125969, .T. ) ;
#122296 = ADVANCED_FACE ( 'NONE', ( #66409 ), #20667, .T. ) ;
#122297 = ADVANCED_FACE ( 'NONE', ( #14073 ), #112414, .T. ) ;
#122298 = FACE_OUTER_BOUND ( 'NONE', #68330, .T. ) ;
#122299 = ORIENTED_EDGE ( 'NONE', *, *, #90083, .T. ) ;
#122300 = VERTEX_POINT ( 'NONE', #75580 ) ;
#122301 = ADVANCED_FACE ( 'NONE', ( #126636 ), #47666, .T. ) ;
#122302 = ORIENTED_EDGE ( 'NONE', *, *, #79472, .F. ) ;
#122303 = ORIENTED_EDGE ( 'NONE', *, *, #51701, .T. ) ;
#122304 = CIRCLE ( 'NONE', #32521, 0.1000000000000000472 ) ;
#122305 = FACE_OUTER_BOUND ( 'NONE', #72159, .T. ) ;
#122306 = CARTESIAN_POINT ( 'NONE',  ( -11.44999999999999751, 12.50000000000000000, -6.776507416713037024 ) ) ;
#122307 = EDGE_CURVE ( 'NONE', #1969, #62361, #81115, .T. ) ;
#122308 = ORIENTED_EDGE ( 'NONE', *, *, #80202, .T. ) ;
#122309 = DIRECTION ( 'NONE',  ( -0.000000000000000000, 1.000000000000000000, -0.000000000000000000 ) ) ;
#122310 = AXIS2_PLACEMENT_3D ( 'NONE', #61443, #109885, #80430 ) ;
#122311 = VECTOR ( 'NONE', #39572, 1000.000000000000000 ) ;
#122312 = CARTESIAN_POINT ( 'NONE',  ( 14.99999999999989164, 12.50000000000000000, 0.6928203230275494784 ) ) ;
#122314 = ORIENTED_EDGE ( 'NONE', *, *, #55185, .T. ) ;
#122313 = DIRECTION ( 'NONE',  ( 0.000000000000000000, 1.000000000000000000, 0.000000000000000000 ) ) ;
#122315 = CIRCLE ( 'NONE', #116033, 0.1000000000000002554 ) ;
#122316 = DIRECTION ( 'NONE',  ( 0.000000000000000000, 0.000000000000000000, 1.000000000000000000 ) ) ;
#122317 = DIRECTION ( 'NONE',  ( 0.000000000000000000, -0.000000000000000000, 1.000000000000000000 ) ) ;
#122318 = EDGE_LOOP ( 'NONE', ( #110913, #68311, #43842, #111803 ) ) ;
#122319 = AXIS2_PLACEMENT_3D ( 'NONE', #117555, #881, #27919 ) ;
#122320 = CIRCLE ( 'NONE', #19814, 0.1000000000000000472 ) ;
#122321 = CIRCLE ( 'NONE', #19815, 0.06509327318403745899 ) ;
#122322 = ORIENTED_EDGE ( 'NONE', *, *, #19105, .T. ) ;
#122323 = ORIENTED_EDGE ( 'NONE', *, *, #105152, .T. ) ;
#122324 = ORIENTED_EDGE ( 'NONE', *, *, #60190, .T. ) ;
#122325 = CARTESIAN_POINT ( 'NONE',  ( 12.09999999999990550, 2.500000000000000000, 5.022947341949748790 ) ) ;
#122326 = VECTOR ( 'NONE', #124879, 1000.000000000000000 ) ;
#122327 = CARTESIAN_POINT ( 'NONE',  ( 1.249999999999954259, 2.500000000000000000, -7.188010851410854052 ) ) ;
#122328 = CARTESIAN_POINT ( 'NONE',  ( -10.20000000000000462, 2.500000000000000000, -4.676537180435973440 ) ) ;
#122329 = AXIS2_PLACEMENT_3D ( 'NONE', #2995, #113591, #15361 ) ;
#122330 = DIRECTION ( 'NONE',  ( 0.000000000000000000, 0.000000000000000000, 1.000000000000000000 ) ) ;
#122331 = EDGE_LOOP ( 'NONE', ( #59087, #7509, #41990, #97782 ) ) ;
#122333 = VECTOR ( 'NONE', #49532, 1000.000000000000000 ) ;
#122332 = DIRECTION ( 'NONE',  ( 0.000000000000000000, 0.000000000000000000, 1.000000000000000000 ) ) ;
#122334 = EDGE_LOOP ( 'NONE', ( #6310, #18567 ) ) ;
#122335 = DIRECTION ( 'NONE',  ( 0.000000000000000000, 0.000000000000000000, -1.000000000000000000 ) ) ;
#122336 = CARTESIAN_POINT ( 'NONE',  ( 6.649999999999930189, 2.500000000000000000, -1.572243186433550211 ) ) ;
#122337 = DIRECTION ( 'NONE',  ( 0.000000000000000000, 0.000000000000000000, 1.000000000000000000 ) ) ;
#122338 = DIRECTION ( 'NONE',  ( 0.000000000000000000, 0.000000000000000000, 1.000000000000000000 ) ) ;
#122339 = ORIENTED_EDGE ( 'NONE', *, *, #89048, .F. ) ;
#122340 = EDGE_CURVE ( 'NONE', #97064, #69733, #33003, .T. ) ;
#122341 = ORIENTED_EDGE ( 'NONE', *, *, #8043, .F. ) ;
#122342 = EDGE_LOOP ( 'NONE', ( #80838, #6046, #21942, #56799 ) ) ;
#122343 = DIRECTION ( 'NONE',  ( -4.274815082592931898E-19, -0.9999939076577903929, -0.003490651415223739937 ) ) ;
#122344 = DIRECTION ( 'NONE',  ( 0.000000000000000000, 0.000000000000000000, 1.000000000000000000 ) ) ;
#122345 = FACE_OUTER_BOUND ( 'NONE', #16391, .T. ) ;
#122346 = FACE_BOUND ( 'NONE', #37703, .T. ) ;
#122347 = DIRECTION ( 'NONE',  ( 0.000000000000000000, 0.000000000000000000, -1.000000000000000000 ) ) ;
#122348 = CIRCLE ( 'NONE', #84672, 0.1000000000000002554 ) ;
#122349 = DIRECTION ( 'NONE',  ( 0.000000000000000000, -0.000000000000000000, 1.000000000000000000 ) ) ;
#122350 = CARTESIAN_POINT ( 'NONE',  ( -1.050000000000038236, 2.500000000000000000, -1.818653347947326138 ) ) ;
#122351 = ADVANCED_FACE ( 'NONE', ( #105038 ), #58132, .T. ) ;
#122352 = CARTESIAN_POINT ( 'NONE',  ( 186.9635416670080303, -4.367472073101520635, 7.564683531249999149 ) ) ;
#122353 = CIRCLE ( 'NONE', #99365, 0.09999999999999982514 ) ;
#122354 = DIRECTION ( 'NONE',  ( -0.8660254037844391517, 0.000000000000000000, -0.4999999999999992228 ) ) ;
#122355 = FACE_OUTER_BOUND ( 'NONE', #111643, .T. ) ;
#122356 = VERTEX_POINT ( 'NONE', #24560 ) ;
#122357 = AXIS2_PLACEMENT_3D ( 'NONE', #111589, #23198, #991 ) ;
#122358 = VECTOR ( 'NONE', #4312, 1000.000000000000000 ) ;
#122359 = FACE_OUTER_BOUND ( 'NONE', #46863, .T. ) ;
#122360 = CARTESIAN_POINT ( 'NONE',  ( -7.100000000000017408, 12.50000000000000000, 0.6928203230275494784 ) ) ;
#122361 = VERTEX_POINT ( 'NONE', #14716 ) ;
#122362 = VERTEX_POINT ( 'NONE', #15360 ) ;
#122363 = CARTESIAN_POINT ( 'NONE',  ( 2.899999999999946620, 12.50000000000000000, -3.637306695894650055 ) ) ;
#122364 = CARTESIAN_POINT ( 'NONE',  ( 9.199999999999915801, 2.500000000000000000, 4.230127018922196669 ) ) ;
#122365 = FACE_BOUND ( 'NONE', #47805, .T. ) ;
#122366 = DIRECTION ( 'NONE',  ( 0.000000000000000000, 0.000000000000000000, -1.000000000000000000 ) ) ;
#122367 = AXIS2_PLACEMENT_3D ( 'NONE', #2692, #73372, #104135 ) ;
#122368 = CIRCLE ( 'NONE', #34643, 0.1000000000000000056 ) ;
#122369 = ORIENTED_EDGE ( 'NONE', *, *, #65354, .T. ) ;
#122370 = CARTESIAN_POINT ( 'NONE',  ( 21.24754738303297330, 0.7337760880902002292, -4.182111650399407132 ) ) ;
#122371 = DIRECTION ( 'NONE',  ( -0.000000000000000000, 1.000000000000000000, -0.000000000000000000 ) ) ;
#122372 = ORIENTED_EDGE ( 'NONE', *, *, #50634, .T. ) ;
#122373 = CARTESIAN_POINT ( 'NONE',  ( -11.04999999999999893, 2.500000000000000000, 1.718653347947321386 ) ) ;
#122374 = DIRECTION ( 'NONE',  ( 0.000000000000000000, 1.000000000000000000, 0.000000000000000000 ) ) ;
#122375 = EDGE_CURVE ( 'NONE', #122097, #40089, #129159, .T. ) ;
#122376 = VECTOR ( 'NONE', #29155, 1000.000000000000000 ) ;
#122377 = VECTOR ( 'NONE', #42721, 1000.000000000000000 ) ;
#122378 = ORIENTED_EDGE ( 'NONE', *, *, #126380, .F. ) ;
#122379 = CARTESIAN_POINT ( 'NONE',  ( -12.29999999999999538, 2.500000000000000000, 4.676537180435972552 ) ) ;
#122380 = FACE_OUTER_BOUND ( 'NONE', #12813, .T. ) ;
#122381 = EDGE_CURVE ( 'NONE', #63670, #126127, #28889, .T. ) ;
#122382 = ORIENTED_EDGE ( 'NONE', *, *, #62386, .F. ) ;
#122383 = CARTESIAN_POINT ( 'NONE',  ( -12.04999999999999716, 2.500000000000000000, -2.165063509461097713 ) ) ;
#122384 = CARTESIAN_POINT ( 'NONE',  ( 186.9062500006828316, -8.891194145520236347, -1.633285867636356299E-15 ) ) ;
#122385 = DIRECTION ( 'NONE',  ( 0.000000000000000000, 1.000000000000000000, 0.000000000000000000 ) ) ;
#122386 = ORIENTED_EDGE ( 'NONE', *, *, #46646, .T. ) ;
#122387 = EDGE_CURVE ( 'NONE', #110101, #26341, #53915, .T. ) ;
#122388 = ORIENTED_EDGE ( 'NONE', *, *, #51996, .T. ) ;
#122389 = ADVANCED_FACE ( 'NONE', ( #50026 ), #49378, .T. ) ;
#122390 = DIRECTION ( 'NONE',  ( 0.000000000000000000, 1.000000000000000000, 0.000000000000000000 ) ) ;
#122391 = CIRCLE ( 'NONE', #97336, 0.06509327318403745899 ) ;
#122392 = VERTEX_POINT ( 'NONE', #77520 ) ;
#122393 = DIRECTION ( 'NONE',  ( -0.000000000000000000, 1.000000000000000000, -0.000000000000000000 ) ) ;
#122394 = LINE ( 'NONE', #53643, #13865 ) ;
#122395 = DIRECTION ( 'NONE',  ( 0.000000000000000000, 0.000000000000000000, -1.000000000000000000 ) ) ;
#122396 = VERTEX_POINT ( 'NONE', #87964 ) ;
#122397 = ADVANCED_FACE ( 'NONE', ( #7487 ), #91567, .T. ) ;
#122398 = CIRCLE ( 'NONE', #84813, 0.06509327318403745899 ) ;
#122399 = CARTESIAN_POINT ( 'NONE',  ( 7.099999999999926814, 2.500000000000000000, -2.276824562219559311E-15 ) ) ;
#122400 = DIRECTION ( 'NONE',  ( 0.000000000000000000, 0.000000000000000000, 1.000000000000000000 ) ) ;
#122401 = DIRECTION ( 'NONE',  ( 0.000000000000000000, 0.000000000000000000, -1.000000000000000000 ) ) ;
#122402 = PLANE ( 'NONE',  #8928 ) ;
#122403 = EDGE_CURVE ( 'NONE', #2627, #12624, #68990, .T. ) ;
#122404 = DIRECTION ( 'NONE',  ( 0.000000000000000000, 0.000000000000000000, 1.000000000000000000 ) ) ;
#122405 = AXIS2_PLACEMENT_3D ( 'NONE', #59003, #85861, #57722 ) ;
#122406 = ORIENTED_EDGE ( 'NONE', *, *, #67483, .F. ) ;
#122407 = ORIENTED_EDGE ( 'NONE', *, *, #1690, .T. ) ;
#122409 = CARTESIAN_POINT ( 'NONE',  ( 10.19999999999991047, 2.500000000000000000, -3.983716857408426293 ) ) ;
#122408 = AXIS2_PLACEMENT_3D ( 'NONE', #77359, #71231, #78660 ) ;
#122410 = ORIENTED_EDGE ( 'NONE', *, *, #36108, .F. ) ;
#122411 = CARTESIAN_POINT ( 'NONE',  ( 4.599999999999940137, 12.50000000000000000, -5.088040615133791356 ) ) ;
#122413 = EDGE_LOOP ( 'NONE', ( #15483, #16078, #17610, #56034 ) ) ;
#122412 = ORIENTED_EDGE ( 'NONE', *, *, #38193, .T. ) ;
#122414 = EDGE_LOOP ( 'NONE', ( #53000, #105085, #42891, #16271 ) ) ;
#122415 = CARTESIAN_POINT ( 'NONE',  ( 2.099999999999950351, 2.500000000000000000, -5.122947341949753763 ) ) ;
#122416 = AXIS2_PLACEMENT_3D ( 'NONE', #42119, #89918, #41500 ) ;
#122418 = CIRCLE ( 'NONE', #38816, 0.1000000000000002554 ) ;
#122417 = DIRECTION ( 'NONE',  ( 0.000000000000000000, -0.9999939076577903929, 0.003490651415223739937 ) ) ;
#122419 = DIRECTION ( 'NONE',  ( -0.000000000000000000, 1.000000000000000000, -0.000000000000000000 ) ) ;
#122420 = CONICAL_SURFACE ( 'NONE', #128704, 0.1000000000000002554, 0.003490658503988666988 ) ;
#122421 = PLANE ( 'NONE',  #13913 ) ;
#122422 = DIRECTION ( 'NONE',  ( -4.274815082592931898E-19, -0.9999939076577903929, -0.003490651415223739937 ) ) ;
#122423 = PLANE ( 'NONE',  #105067 ) ;
#122424 = CONICAL_SURFACE ( 'NONE', #84762, 0.1000000000000002554, 0.003490658503988666988 ) ;
#122425 = LINE ( 'NONE', #30834, #30932 ) ;
#122426 = CARTESIAN_POINT ( 'NONE',  ( -2.050000000000033129, 12.50000000000000000, 6.560283801567334372 ) ) ;
#122427 = DIRECTION ( 'NONE',  ( -0.000000000000000000, -1.000000000000000000, -0.000000000000000000 ) ) ;
#122428 = EDGE_LOOP ( 'NONE', ( #86571, #92362, #60899, #62307 ) ) ;
#122429 = EDGE_CURVE ( 'NONE', #17323, #103868, #62245, .T. ) ;
#122430 = FACE_OUTER_BOUND ( 'NONE', #48235, .T. ) ;
#122431 = EDGE_LOOP ( 'NONE', ( #4893, #21361 ) ) ;
#122432 = VERTEX_POINT ( 'NONE', #108899 ) ;
#122433 = CARTESIAN_POINT ( 'NONE',  ( 8.949999999999921130, 12.50000000000000000, 1.818653347947321475 ) ) ;
#122434 = CARTESIAN_POINT ( 'NONE',  ( -9.350000000000008527, 2.500000000000000000, -6.841600689897072485 ) ) ;
#122435 = AXIS2_PLACEMENT_3D ( 'NONE', #13202, #103544, #3398 ) ;
#122436 = DIRECTION ( 'NONE',  ( 0.000000000000000000, 1.000000000000000000, 0.000000000000000000 ) ) ;
#122437 = EDGE_CURVE ( 'NONE', #90797, #15482, #24675, .T. ) ;
#122438 = DIRECTION ( 'NONE',  ( 1.000000000000000000, 0.000000000000000000, -0.000000000000000000 ) ) ;
#122439 = CARTESIAN_POINT ( 'NONE',  ( -4.200000000000029488, 2.500000000000000000, -4.330127018922201643 ) ) ;
#122440 = DIRECTION ( 'NONE',  ( 0.000000000000000000, 1.000000000000000000, 0.000000000000000000 ) ) ;
#122441 = FACE_OUTER_BOUND ( 'NONE', #121998, .T. ) ;
#122442 = EDGE_LOOP ( 'NONE', ( #18400, #94713 ) ) ;
#122443 = ADVANCED_FACE ( 'NONE', ( #97805 ), #62334, .T. ) ;
#122444 = AXIS2_PLACEMENT_3D ( 'NONE', #7902, #17716, #38691 ) ;
#122445 = ADVANCED_FACE ( 'NONE', ( #27770 ), #67695, .T. ) ;
#122446 = CIRCLE ( 'NONE', #55543, 0.06509327318403745899 ) ;
#122447 = EDGE_CURVE ( 'NONE', #81045, #66966, #74848, .T. ) ;
#122448 = AXIS2_PLACEMENT_3D ( 'NONE', #110909, #60561, #23178 ) ;
#122449 = VERTEX_POINT ( 'NONE', #28436 ) ;
#122450 = EDGE_LOOP ( 'NONE', ( #88528, #63270 ) ) ;
#122451 = AXIS2_PLACEMENT_3D ( 'NONE', #786, #51838, #69528 ) ;
#122452 = EDGE_CURVE ( 'NONE', #38135, #20260, #127090, .T. ) ;
#122453 = ORIENTED_EDGE ( 'NONE', *, *, #80935, .T. ) ;
#122454 = ORIENTED_EDGE ( 'NONE', *, *, #34235, .T. ) ;
#122455 = CARTESIAN_POINT ( 'NONE',  ( 4.199999999999938005, 12.50000000000000000, 4.395220292106234439 ) ) ;
#122456 = DIRECTION ( 'NONE',  ( -0.000000000000000000, 1.000000000000000000, -0.000000000000000000 ) ) ;
#122457 = ADVANCED_FACE ( 'NONE', ( #67036 ), #64370, .T. ) ;
#122458 = AXIS2_PLACEMENT_3D ( 'NONE', #40579, #83704, #3215 ) ;
#122459 = ADVANCED_FACE ( 'NONE', ( #48725 ), #66426, .T. ) ;
#122460 = CARTESIAN_POINT ( 'NONE',  ( 6.049999999999932321, 12.50000000000000000, 6.841600689897072485 ) ) ;
#122461 = DIRECTION ( 'NONE',  ( 0.000000000000000000, 0.000000000000000000, 1.000000000000000000 ) ) ;
#122463 = CIRCLE ( 'NONE', #114127, 0.06509327318403745899 ) ;
#122462 = AXIS2_PLACEMENT_3D ( 'NONE', #128380, #111260, #38717 ) ;
#122464 = CARTESIAN_POINT ( 'NONE',  ( 9.349999999999919709, 2.500000000000000000, 1.818653347947321475 ) ) ;
#122465 = EDGE_LOOP ( 'NONE', ( #124231, #13548, #64099, #38898 ) ) ;
#122466 = DIRECTION ( 'NONE',  ( -0.000000000000000000, 1.000000000000000000, -0.000000000000000000 ) ) ;
#122467 = DIRECTION ( 'NONE',  ( 0.000000000000000000, 0.000000000000000000, -1.000000000000000000 ) ) ;
#122468 = CARTESIAN_POINT ( 'NONE',  ( 5.849999999999935696, 2.500000000000000000, -6.595190528383302109 ) ) ;
#122469 = CARTESIAN_POINT ( 'NONE',  ( 0.6499999999999561684, 2.500000000000000000, -1.818653347947325916 ) ) ;
#122470 = EDGE_LOOP ( 'NONE', ( #83922, #94149, #23994, #71916 ) ) ;
#122471 = CONICAL_SURFACE ( 'NONE', #51374, 0.1000000000000002554, 0.003490658503988666988 ) ;
#122472 = AXIS2_PLACEMENT_3D ( 'NONE', #13863, #53795, #54435 ) ;
#122473 = VERTEX_POINT ( 'NONE', #8130 ) ;
#122474 = VERTEX_POINT ( 'NONE', #17956 ) ;
#122475 = DIRECTION ( 'NONE',  ( 0.000000000000000000, 0.000000000000000000, 1.000000000000000000 ) ) ;
#122476 = ORIENTED_EDGE ( 'NONE', *, *, #117738, .F. ) ;
#122477 = CARTESIAN_POINT ( 'NONE',  ( -1.050000000000037792, 2.500000000000000000, 6.148780366869520009 ) ) ;
#122478 = DIRECTION ( 'NONE',  ( -4.274815082592931898E-19, -0.9999939076577903929, -0.003490651415223739937 ) ) ;
#122479 = EDGE_LOOP ( 'NONE', ( #23203, #118920, #60618, #25765 ) ) ;
#122480 = CARTESIAN_POINT ( 'NONE',  ( -13.29999999999999005, 2.500000000000000000, 1.843143693225357538E-15 ) ) ;
#122482 = ADVANCED_FACE ( 'NONE', ( #29714 ), #69638, .T. ) ;
#122481 = DIRECTION ( 'NONE',  ( 0.000000000000000000, -0.9999939076577903929, 0.003490651415223739937 ) ) ;
#122483 = CARTESIAN_POINT ( 'NONE',  ( 1.449999999999951328, 2.500000000000000000, 2.511473670974873507 ) ) ;
#122484 = DIRECTION ( 'NONE',  ( 0.000000000000000000, -0.9999939076577903929, 0.003490651415223739937 ) ) ;
#122485 = VECTOR ( 'NONE', #114170, 1000.000000000000000 ) ;
#122486 = CARTESIAN_POINT ( 'NONE',  ( -11.25000000000000178, 12.50000000000000000, -1.407149913249508666 ) ) ;
#122487 = AXIS2_PLACEMENT_3D ( 'NONE', #18454, #48567, #39413 ) ;
#122488 = VERTEX_POINT ( 'NONE', #57242 ) ;
#122489 = EDGE_LOOP ( 'NONE', ( #104590, #17969, #2780, #15439 ) ) ;
#122490 = DIRECTION ( 'NONE',  ( 0.000000000000000000, 1.000000000000000000, 0.000000000000000000 ) ) ;
#122491 = FACE_OUTER_BOUND ( 'NONE', #40681, .T. ) ;
#122492 = FACE_OUTER_BOUND ( 'NONE', #37954, .T. ) ;
#122493 = LINE ( 'NONE', #120554, #104405 ) ;
#122494 = EDGE_CURVE ( 'NONE', #8018, #35473, #5770, .T. ) ;
#122495 = ORIENTED_EDGE ( 'NONE', *, *, #12712, .F. ) ;
#122496 = VERTEX_POINT ( 'NONE', #12003 ) ;
#122497 = LINE ( 'NONE', #42665, #106501 ) ;
#122498 = FACE_OUTER_BOUND ( 'NONE', #4425, .T. ) ;
#122499 = DIRECTION ( 'NONE',  ( 0.000000000000000000, 0.000000000000000000, 1.000000000000000000 ) ) ;
#122500 = CARTESIAN_POINT ( 'NONE',  ( -2.050000000000032685, 2.500000000000000000, -2.165063509461101710 ) ) ;
#122501 = EDGE_LOOP ( 'NONE', ( #29818, #75415 ) ) ;
#122502 = AXIS2_PLACEMENT_3D ( 'NONE', #56433, #85260, #6659 ) ;
#122503 = CARTESIAN_POINT ( 'NONE',  ( -12.29999999999999538, 2.500000000000000000, -4.676537180435976104 ) ) ;
#122504 = VECTOR ( 'NONE', #108071, 1000.000000000000000 ) ;
#122505 = CARTESIAN_POINT ( 'NONE',  ( -13.29999999999999005, 2.500000000000000000, 1.843143693225357538E-15 ) ) ;
#122506 = CIRCLE ( 'NONE', #111754, 0.06509327318403745899 ) ;
#122507 = ORIENTED_EDGE ( 'NONE', *, *, #13977, .F. ) ;
#122508 = DIRECTION ( 'NONE',  ( 0.000000000000000000, 0.000000000000000000, 1.000000000000000000 ) ) ;
#122509 = ORIENTED_EDGE ( 'NONE', *, *, #58136, .T. ) ;
#122510 = DIRECTION ( 'NONE',  ( 0.000000000000000000, 1.000000000000000000, 0.000000000000000000 ) ) ;
#122511 = ORIENTED_EDGE ( 'NONE', *, *, #37934, .T. ) ;
#122512 = FACE_OUTER_BOUND ( 'NONE', #21567, .T. ) ;
#122513 = LINE ( 'NONE', #112696, #43909 ) ;
#122514 = ORIENTED_EDGE ( 'NONE', *, *, #5425, .F. ) ;
#122515 = EDGE_LOOP ( 'NONE', ( #89364, #49927, #104409, #66220 ) ) ;
#122516 = DIRECTION ( 'NONE',  ( 0.000000000000000000, 0.000000000000000000, -1.000000000000000000 ) ) ;
#122517 = CARTESIAN_POINT ( 'NONE',  ( -7.900000000000014566, 12.50000000000000000, -0.6928203230275541413 ) ) ;
#122518 = AXIS2_PLACEMENT_3D ( 'NONE', #12409, #52343, #73270 ) ;
#122519 = CARTESIAN_POINT ( 'NONE',  ( 187.0468750003414300, -8.734944146203032389, -1.604583208406767949E-15 ) ) ;
#122520 = CARTESIAN_POINT ( 'NONE',  ( 184.1510416670080588, 4.367472073101518859, -7.564683531249999149 ) ) ;
#122521 = DIRECTION ( 'NONE',  ( -0.000000000000000000, -1.000000000000000000, -0.000000000000000000 ) ) ;
#122522 = CIRCLE ( 'NONE', #127021, 0.06509327318403745899 ) ;
#122523 = DIRECTION ( 'NONE',  ( 0.000000000000000000, -0.9999939076577903929, 0.003490651415223739937 ) ) ;
#122524 = DIRECTION ( 'NONE',  ( 0.000000000000000000, -0.9999939076577903929, 0.003490651415223739937 ) ) ;
#122525 = CARTESIAN_POINT ( 'NONE',  ( -0.4000000000000404898, 2.500000000000000000, 5.022947341949748790 ) ) ;
#122526 = CONICAL_SURFACE ( 'NONE', #112158, 0.1000000000000000472, 0.003490658503988666988 ) ;
#122527 = DIRECTION ( 'NONE',  ( -1.000000000000000000, 0.000000000000000000, 0.000000000000000000 ) ) ;
#122528 = AXIS2_PLACEMENT_3D ( 'NONE', #123789, #55069, #43331 ) ;
#122529 = EDGE_CURVE ( 'NONE', #102213, #105669, #23114, .T. ) ;
#122530 = VERTEX_POINT ( 'NONE', #80760 ) ;
#122531 = AXIS2_PLACEMENT_3D ( 'NONE', #4006, #68085, #16384 ) ;
#122532 = ORIENTED_EDGE ( 'NONE', *, *, #58465, .T. ) ;
#122533 = CARTESIAN_POINT ( 'NONE',  ( -1.650000000000034772, 12.50000000000000000, 6.495190528383297135 ) ) ;
#122534 = ORIENTED_EDGE ( 'NONE', *, *, #92235, .T. ) ;
#122535 = CARTESIAN_POINT ( 'NONE',  ( 9.199999999999919353, 12.50000000000000000, -2.276824562219559311E-15 ) ) ;
#122536 = CARTESIAN_POINT ( 'NONE',  ( -7.500000000000011546, 12.50000000000000000, 3.637306695894644726 ) ) ;
#122537 = LINE ( 'NONE', #72154, #30174 ) ;
#122539 = VERTEX_POINT ( 'NONE', #30381 ) ;
#122538 = EDGE_LOOP ( 'NONE', ( #90981, #25116 ) ) ;
#122540 = EDGE_CURVE ( 'NONE', #91908, #123357, #120680, .T. ) ;
#122541 = FACE_BOUND ( 'NONE', #37878, .T. ) ;
#122542 = ORIENTED_EDGE ( 'NONE', *, *, #128169, .F. ) ;
#122543 = ADVANCED_FACE ( 'NONE', ( #101684 ), #40188, .T. ) ;
#122544 = FACE_OUTER_BOUND ( 'NONE', #86014, .T. ) ;
#122545 = CARTESIAN_POINT ( 'NONE',  ( 19.01901804971378240, -2.576149587736908941, 2.431039412660930044 ) ) ;
#122546 = VECTOR ( 'NONE', #121677, 1000.000000000000000 ) ;
#122547 = LINE ( 'NONE', #71499, #109894 ) ;
#122548 = FACE_OUTER_BOUND ( 'NONE', #45681, .T. ) ;
#122549 = CARTESIAN_POINT ( 'NONE',  ( 184.2812500006828031, 0.000000000000000000, 7.700000000000000178 ) ) ;
#122551 = AXIS2_PLACEMENT_3D ( 'NONE', #9853, #20321, #110625 ) ;
#122550 = CIRCLE ( 'NONE', #28551, 0.06509327318403743123 ) ;
#122552 = CARTESIAN_POINT ( 'NONE',  ( 15.19999999999989271, 12.50000000000000000, -0.3464101615137783474 ) ) ;
#122553 = EDGE_CURVE ( 'NONE', #30037, #72858, #43467, .T. ) ;
#122554 = DIRECTION ( 'NONE',  ( 0.000000000000000000, 1.000000000000000000, 0.000000000000000000 ) ) ;
#122555 = ADVANCED_FACE ( 'NONE', ( #82028 ), #3734, .T. ) ;
#122556 = CARTESIAN_POINT ( 'NONE',  ( 9.349999999999919709, 2.500000000000000000, -6.248780366869526759 ) ) ;
#122557 = FACE_OUTER_BOUND ( 'NONE', #125517, .T. ) ;
#122558 = CARTESIAN_POINT ( 'NONE',  ( -6.900000000000019007, 2.500000000000000000, 0.3464101615137735735 ) ) ;
#122559 = EDGE_CURVE ( 'NONE', #67957, #29548, #93628, .T. ) ;
#122560 = DIRECTION ( 'NONE',  ( 0.000000000000000000, 0.000000000000000000, 1.000000000000000000 ) ) ;
#122561 = ORIENTED_EDGE ( 'NONE', *, *, #79815, .T. ) ;
#122562 = ORIENTED_EDGE ( 'NONE', *, *, #29898, .F. ) ;
#122563 = EDGE_LOOP ( 'NONE', ( #44482, #16132, #114085, #95381 ) ) ;
#122564 = DIRECTION ( 'NONE',  ( -0.000000000000000000, 1.000000000000000000, -0.000000000000000000 ) ) ;
#122565 = ORIENTED_EDGE ( 'NONE', *, *, #67463, .F. ) ;
#122566 = DIRECTION ( 'NONE',  ( 0.000000000000000000, 0.000000000000000000, -1.000000000000000000 ) ) ;
#122568 = ORIENTED_EDGE ( 'NONE', *, *, #110666, .T. ) ;
#122567 = ORIENTED_EDGE ( 'NONE', *, *, #648, .F. ) ;
#122569 = VERTEX_POINT ( 'NONE', #72866 ) ;
#122570 = FACE_OUTER_BOUND ( 'NONE', #17580, .T. ) ;
#122571 = CARTESIAN_POINT ( 'NONE',  ( 1.249999999999988898, 2.500000000000000000, -6.495190528383302464 ) ) ;
#122572 = DIRECTION ( 'NONE',  ( 0.000000000000000000, 0.000000000000000000, 1.000000000000000000 ) ) ;
#122573 = CARTESIAN_POINT ( 'NONE',  ( -0.8500000000000386136, 12.50000000000000000, 2.857883832488649301 ) ) ;
#122574 = DIRECTION ( 'NONE',  ( -0.000000000000000000, 1.000000000000000000, -0.000000000000000000 ) ) ;
#122575 = CARTESIAN_POINT ( 'NONE',  ( 5.649999999999934630, 2.500000000000000000, 6.741600689897071952 ) ) ;
#122576 = VERTEX_POINT ( 'NONE', #31034 ) ;
#122577 = CARTESIAN_POINT ( 'NONE',  ( 1.649999999999951950, 2.500000000000000000, -5.802370205355749988 ) ) ;
#122578 = ORIENTED_EDGE ( 'NONE', *, *, #2875, .F. ) ;
#122579 = ORIENTED_EDGE ( 'NONE', *, *, #74952, .T. ) ;
#122580 = EDGE_LOOP ( 'NONE', ( #50008, #79228, #71177, #29033 ) ) ;
#122581 = CIRCLE ( 'NONE', #24377, 0.06509327318403745899 ) ;
#122582 = CARTESIAN_POINT ( 'NONE',  ( 185.0729166673495172, 4.445597072760072876, -7.700000000000080114 ) ) ;
#122583 = ORIENTED_EDGE ( 'NONE', *, *, #103226, .T. ) ;
#122584 = ORIENTED_EDGE ( 'NONE', *, *, #81655, .T. ) ;
#122585 = ORIENTED_EDGE ( 'NONE', *, *, #25008, .F. ) ;
#122586 = DIRECTION ( 'NONE',  ( 0.000000000000000000, 1.000000000000000000, 0.000000000000000000 ) ) ;
#122587 = CIRCLE ( 'NONE', #11845, 0.09999999999999982514 ) ;
#122588 = DIRECTION ( 'NONE',  ( 0.000000000000000000, -0.000000000000000000, 1.000000000000000000 ) ) ;
#122589 = CARTESIAN_POINT ( 'NONE',  ( 14.79999999999989413, 2.500000000000000000, -0.2464101615137782308 ) ) ;
#122590 = DIRECTION ( 'NONE',  ( 0.000000000000000000, 0.000000000000000000, 1.000000000000000000 ) ) ;
#122591 = FACE_OUTER_BOUND ( 'NONE', #29125, .T. ) ;
#122592 = ADVANCED_FACE ( 'NONE', ( #62415 ), #120816, .T. ) ;
#122593 = CARTESIAN_POINT ( 'NONE',  ( 1.849999999999949685, 2.500000000000000000, 1.718653347947321386 ) ) ;
#122594 = ADVANCED_FACE ( 'NONE', ( #112148 ), #78975, .T. ) ;
#122595 = EDGE_CURVE ( 'NONE', #123681, #8315, #91864, .T. ) ;
#122596 = CARTESIAN_POINT ( 'NONE',  ( 9.149999999999920419, 12.50000000000000000, 2.857883832488649301 ) ) ;
#122598 = CIRCLE ( 'NONE', #22258, 0.1000000000000000056 ) ;
#122597 = CONICAL_SURFACE ( 'NONE', #28507, 0.1000000000000002554, 0.003490658503988666988 ) ;
#122599 = ORIENTED_EDGE ( 'NONE', *, *, #40895, .F. ) ;
#122600 = PLANE ( 'NONE',  #102807 ) ;
#122601 = ORIENTED_EDGE ( 'NONE', *, *, #21943, .F. ) ;
#122603 = VERTEX_POINT ( 'NONE', #110841 ) ;
#122602 = ADVANCED_FACE ( 'NONE', ( #12639 ), #39279, .T. ) ;
#122604 = DIRECTION ( 'NONE',  ( -0.000000000000000000, -1.000000000000000000, -0.000000000000000000 ) ) ;
#122605 = EDGE_CURVE ( 'NONE', #2437, #28355, #95693, .T. ) ;
#122606 = ORIENTED_EDGE ( 'NONE', *, *, #90346, .F. ) ;
#122607 = EDGE_CURVE ( 'NONE', #45548, #14446, #100394, .T. ) ;
#122608 = CARTESIAN_POINT ( 'NONE',  ( 9.399999999999915090, 2.500000000000000000, 4.676537180435972552 ) ) ;
#122609 = EDGE_CURVE ( 'NONE', #89145, #702, #43564, .T. ) ;
#122610 = EDGE_CURVE ( 'NONE', #43078, #8727, #93714, .T. ) ;
#122611 = CARTESIAN_POINT ( 'NONE',  ( 11.04999999999991012, 2.500000000000000000, 6.941600689897073018 ) ) ;
#122612 = VERTEX_POINT ( 'NONE', #53235 ) ;
#122613 = ORIENTED_EDGE ( 'NONE', *, *, #121073, .F. ) ;
#122614 = CARTESIAN_POINT ( 'NONE',  ( 3.549999999999942091, 2.500000000000000000, 2.511473670974873507 ) ) ;
#122615 = CARTESIAN_POINT ( 'NONE',  ( -8.350000000000013856, 12.50000000000000000, -7.253104124594885960 ) ) ;
#122616 = DIRECTION ( 'NONE',  ( -0.000000000000000000, 1.000000000000000000, -0.000000000000000000 ) ) ;
#122617 = CIRCLE ( 'NONE', #34799, 0.06509327318403745899 ) ;
#122618 = DIRECTION ( 'NONE',  ( 0.000000000000000000, 1.000000000000000000, 0.000000000000000000 ) ) ;
#122619 = ADVANCED_FACE ( 'NONE', ( #13280 ), #87444, .T. ) ;
#122620 = LINE ( 'NONE', #23120, #81449 ) ;
#122621 = VERTEX_POINT ( 'NONE', #41499 ) ;
#122622 = FACE_OUTER_BOUND ( 'NONE', #61995, .T. ) ;
#122623 = AXIS2_PLACEMENT_3D ( 'NONE', #499, #61382, #101308 ) ;
#122624 = AXIS2_PLACEMENT_3D ( 'NONE', #43966, #34145, #100930 ) ;
#122625 = EDGE_LOOP ( 'NONE', ( #62932, #110932 ) ) ;
#122626 = CARTESIAN_POINT ( 'NONE',  ( 12.89999999999989910, 2.500000000000000000, -0.7928203230275543412 ) ) ;
#122627 = DIRECTION ( 'NONE',  ( 0.000000000000000000, 0.000000000000000000, -1.000000000000000000 ) ) ;
#122628 = AXIS2_PLACEMENT_3D ( 'NONE', #63434, #113830, #64076 ) ;
#122629 = CARTESIAN_POINT ( 'NONE',  ( 184.0052083336747160, -6.551208109652278289, 3.782341765624995134 ) ) ;
#122630 = FACE_OUTER_BOUND ( 'NONE', #99292, .T. ) ;
#122631 = LINE ( 'NONE', #32977, #69545 ) ;
#122632 = CARTESIAN_POINT ( 'NONE',  ( -10.40000000000000213, 2.500000000000000000, -0.1000000000000022815 ) ) ;
#122633 = CARTESIAN_POINT ( 'NONE',  ( -11.64999999999999858, 2.500000000000000000, -1.572243186433546214 ) ) ;
#122634 = ORIENTED_EDGE ( 'NONE', *, *, #84894, .T. ) ;
#122635 = CIRCLE ( 'NONE', #36961, 0.1000000000000002554 ) ;
#122636 = DIRECTION ( 'NONE',  ( 0.000000000000000000, 1.000000000000000000, 0.000000000000000000 ) ) ;
#122637 = VECTOR ( 'NONE', #94709, 1000.000000000000000 ) ;
#122638 = CARTESIAN_POINT ( 'NONE',  ( 7.049999999999928768, 12.50000000000000000, 6.495190528383297135 ) ) ;
#122639 = CARTESIAN_POINT ( 'NONE',  ( 0.5999999999999560130, 12.50000000000000000, -3.983716857408426293 ) ) ;
#122640 = ORIENTED_EDGE ( 'NONE', *, *, #81120, .T. ) ;
#122641 = DIRECTION ( 'NONE',  ( 0.000000000000000000, 0.000000000000000000, -1.000000000000000000 ) ) ;
#122642 = EDGE_CURVE ( 'NONE', #77248, #118978, #81409, .T. ) ;
#122643 = ORIENTED_EDGE ( 'NONE', *, *, #126383, .T. ) ;
#122644 = ORIENTED_EDGE ( 'NONE', *, *, #70517, .F. ) ;
#122645 = CARTESIAN_POINT ( 'NONE',  ( 2.049999999999950084, 2.500000000000000000, 2.265063509461097357 ) ) ;
#122646 = ORIENTED_EDGE ( 'NONE', *, *, #46130, .F. ) ;
#122647 = CARTESIAN_POINT ( 'NONE',  ( 12.04999999999990834, 12.50000000000000000, -2.165063509461101710 ) ) ;
#122648 = CARTESIAN_POINT ( 'NONE',  ( 13.34999999999990017, 2.500000000000000000, 2.857883832488649301 ) ) ;
#122649 = DIRECTION ( 'NONE',  ( -0.000000000000000000, 1.000000000000000000, -0.000000000000000000 ) ) ;
#122650 = ORIENTED_EDGE ( 'NONE', *, *, #24422, .F. ) ;
#122651 = CARTESIAN_POINT ( 'NONE',  ( -9.150000000000009237, 2.500000000000000000, 2.165063509461097713 ) ) ;
#122652 = CARTESIAN_POINT ( 'NONE',  ( -4.250072516143177381E-14, 2.500000000000000000, -3.637306695894650055 ) ) ;
#122653 = EDGE_CURVE ( 'NONE', #18590, #69752, #76993, .T. ) ;
#122654 = EDGE_LOOP ( 'NONE', ( #26821, #44778, #74643, #36279 ) ) ;
#122655 = VECTOR ( 'NONE', #68776, 1000.000000000000000 ) ;
#122656 = ORIENTED_EDGE ( 'NONE', *, *, #62119, .T. ) ;
#122657 = CONICAL_SURFACE ( 'NONE', #68367, 0.09999999999999982514, 0.003490658503988666988 ) ;
#122658 = VERTEX_POINT ( 'NONE', #13927 ) ;
#122659 = DIRECTION ( 'NONE',  ( 0.000000000000000000, 0.000000000000000000, 1.000000000000000000 ) ) ;
#122660 = FACE_OUTER_BOUND ( 'NONE', #82290, .T. ) ;
#122661 = FACE_OUTER_BOUND ( 'NONE', #62395, .T. ) ;
#122662 = ORIENTED_EDGE ( 'NONE', *, *, #67077, .T. ) ;
#122663 = CARTESIAN_POINT ( 'NONE',  ( 11.64999999999990443, 12.50000000000000000, -5.802370205355749988 ) ) ;
#122664 = DIRECTION ( 'NONE',  ( 0.000000000000000000, 0.000000000000000000, -1.000000000000000000 ) ) ;
#122665 = ORIENTED_EDGE ( 'NONE', *, *, #83606, .T. ) ;
#122667 = CIRCLE ( 'NONE', #26525, 0.1000000000000002554 ) ;
#122666 = CONICAL_SURFACE ( 'NONE', #64173, 0.1000000000000000472, 0.003490658503988666988 ) ;
#122668 = CARTESIAN_POINT ( 'NONE',  ( 7.899999999999921307, 12.50000000000000000, -2.385244779468109755E-15 ) ) ;
#122669 = CARTESIAN_POINT ( 'NONE',  ( 3.099999999999945466, 2.500000000000000000, -3.883716857408426648 ) ) ;
#122670 = FACE_OUTER_BOUND ( 'NONE', #89958, .T. ) ;
#122671 = CARTESIAN_POINT ( 'NONE',  ( -11.89999999999999503, 2.500000000000000000, 4.083716857408420609 ) ) ;
#122672 = DIRECTION ( 'NONE',  ( -0.000000000000000000, -1.000000000000000000, -0.000000000000000000 ) ) ;
#122673 = AXIS2_PLACEMENT_3D ( 'NONE', #5973, #64898, #4673 ) ;
#122674 = CARTESIAN_POINT ( 'NONE',  ( 11.84999999999990372, 12.50000000000000000, -6.776507416713040577 ) ) ;
#122675 = CARTESIAN_POINT ( 'NONE',  ( 1.649999999999951950, 2.500000000000000000, -5.702370205355749455 ) ) ;
#122677 = CIRCLE ( 'NONE', #126888, 0.1000000000000002554 ) ;
#122676 = AXIS2_PLACEMENT_3D ( 'NONE', #59025, #100865, #21682 ) ;
#122679 = ADVANCED_FACE ( 'NONE', ( #44049 ), #5957, .T. ) ;
#122678 = CIRCLE ( 'NONE', #11857, 0.1000000000000002554 ) ;
#122680 = VERTEX_POINT ( 'NONE', #5402 ) ;
#122681 = ORIENTED_EDGE ( 'NONE', *, *, #92064, .F. ) ;
#122682 = ORIENTED_EDGE ( 'NONE', *, *, #39830, .T. ) ;
#122683 = ORIENTED_EDGE ( 'NONE', *, *, #12046, .T. ) ;
#122684 = FACE_OUTER_BOUND ( 'NONE', #99007, .T. ) ;
#122685 = DIRECTION ( 'NONE',  ( 1.000000000000000000, 0.000000000000000000, 0.000000000000000000 ) ) ;
#122686 = LINE ( 'NONE', #61192, #122008 ) ;
#122687 = ORIENTED_EDGE ( 'NONE', *, *, #1956, .F. ) ;
#122688 = FACE_BOUND ( 'NONE', #76778, .T. ) ;
#122689 = ADVANCED_FACE ( 'NONE', ( #16498 ), #39370, .T. ) ;
#122690 = DIRECTION ( 'NONE',  ( 0.000000000000000000, 1.000000000000000000, 0.000000000000000000 ) ) ;
#122691 = DIRECTION ( 'NONE',  ( 0.000000000000000000, 0.000000000000000000, 1.000000000000000000 ) ) ;
#122692 = CARTESIAN_POINT ( 'NONE',  ( -9.350000000000006750, 2.500000000000000000, 2.411473670974873862 ) ) ;
#122693 = DIRECTION ( 'NONE',  ( -4.274815082592931898E-19, -0.9999939076577903929, -0.003490651415223739937 ) ) ;
#122694 = CARTESIAN_POINT ( 'NONE',  ( -8.750000000000008882, 12.50000000000000000, -2.857883832488653741 ) ) ;
#122695 = EDGE_CURVE ( 'NONE', #105744, #63695, #125189, .T. ) ;
#122696 = DIRECTION ( 'NONE',  ( -0.000000000000000000, -1.000000000000000000, -0.000000000000000000 ) ) ;
#122697 = EDGE_CURVE ( 'NONE', #23087, #949, #26350, .T. ) ;
#122698 = DIRECTION ( 'NONE',  ( 0.000000000000000000, 1.000000000000000000, 0.000000000000000000 ) ) ;
#122699 = CARTESIAN_POINT ( 'NONE',  ( -2.499999999999996003, 12.50000000000000000, -4.330127018922201643 ) ) ;
#122700 = EDGE_CURVE ( 'NONE', #113873, #42980, #34893, .T. ) ;
#122701 = CARTESIAN_POINT ( 'NONE',  ( 1.449999999999949551, 2.500000000000000000, 6.841600689897072485 ) ) ;
#122702 = ADVANCED_FACE ( 'NONE', ( #73492 ), #68670, .T. ) ;
#122703 = VECTOR ( 'NONE', #114962, 1000.000000000000000 ) ;
#122704 = EDGE_CURVE ( 'NONE', #13568, #75204, #47755, .T. ) ;
#122705 = VERTEX_POINT ( 'NONE', #94421 ) ;
#122706 = ORIENTED_EDGE ( 'NONE', *, *, #64494, .T. ) ;
#122708 = ORIENTED_EDGE ( 'NONE', *, *, #5042, .T. ) ;
#122707 = CIRCLE ( 'NONE', #34993, 0.09999999999999982514 ) ;
#122709 = ORIENTED_EDGE ( 'NONE', *, *, #97151, .F. ) ;
#122710 = ORIENTED_EDGE ( 'NONE', *, *, #6971, .T. ) ;
#122711 = ORIENTED_EDGE ( 'NONE', *, *, #49604, .T. ) ;
#122712 = DIRECTION ( 'NONE',  ( 0.000000000000000000, -0.9999939076577903929, 0.003490651415223739937 ) ) ;
#122713 = EDGE_LOOP ( 'NONE', ( #77946, #11774 ) ) ;
#122714 = ADVANCED_FACE ( 'NONE', ( #34249 ), #114078, .T. ) ;
#122716 = EDGE_LOOP ( 'NONE', ( #91361, #12226 ) ) ;
#122715 = AXIS2_PLACEMENT_3D ( 'NONE', #80361, #109810, #1770 ) ;
#122717 = CIRCLE ( 'NONE', #1516, 0.06509327318403745899 ) ;
#122718 = EDGE_CURVE ( 'NONE', #126712, #112141, #5868, .T. ) ;
#122719 = CARTESIAN_POINT ( 'NONE',  ( 16.04744068708433247, -2.499999999999937828, 6.586254740843006772 ) ) ;
#122720 = DIRECTION ( 'NONE',  ( 0.000000000000000000, 0.000000000000000000, 1.000000000000000000 ) ) ;
#122721 = CARTESIAN_POINT ( 'NONE',  ( -10.65000000000000213, 12.50000000000000000, 2.511473670974873507 ) ) ;
#122722 = CONICAL_SURFACE ( 'NONE', #66279, 0.1000000000000002554, 0.003490658503988666988 ) ;
#122723 = ORIENTED_EDGE ( 'NONE', *, *, #27902, .F. ) ;
#122724 = CARTESIAN_POINT ( 'NONE',  ( 7.049999999999928768, 2.500000000000000000, -2.065063509461102065 ) ) ;
#122725 = VECTOR ( 'NONE', #41383, 1000.000000000000000 ) ;
#122726 = EDGE_LOOP ( 'NONE', ( #28493, #29687, #70152, #42713 ) ) ;
#122728 = AXIS2_PLACEMENT_3D ( 'NONE', #74571, #15631, #66034 ) ;
#122727 = CONICAL_SURFACE ( 'NONE', #18260, 0.1000000000000002554, 0.003490658503988666988 ) ;
#122729 = EDGE_LOOP ( 'NONE', ( #69181, #117046 ) ) ;
#122730 = CARTESIAN_POINT ( 'NONE',  ( 12.49999999999993960, 2.500000000000000000, 4.330127018922196314 ) ) ;
#122731 = FACE_OUTER_BOUND ( 'NONE', #60498, .T. ) ;
#122732 = ORIENTED_EDGE ( 'NONE', *, *, #102954, .T. ) ;
#122733 = ORIENTED_EDGE ( 'NONE', *, *, #52414, .T. ) ;
#122734 = DIRECTION ( 'NONE',  ( 0.000000000000000000, 0.000000000000000000, -1.000000000000000000 ) ) ;
#122735 = FACE_OUTER_BOUND ( 'NONE', #20090, .T. ) ;
#122736 = CARTESIAN_POINT ( 'NONE',  ( 0.1999999999999627909, 12.50000000000000000, 0.3464101615137758494 ) ) ;
#122737 = FACE_OUTER_BOUND ( 'NONE', #66443, .T. ) ;
#122738 = CARTESIAN_POINT ( 'NONE',  ( 14.34999999999989306, 12.50000000000000000, -1.818653347947326138 ) ) ;
#122739 = CONICAL_SURFACE ( 'NONE', #118527, 0.1000000000000002554, 0.003490658503988666988 ) ;
#122740 = ORIENTED_EDGE ( 'NONE', *, *, #18555, .F. ) ;
#122741 = EDGE_CURVE ( 'NONE', #65687, #127955, #89511, .T. ) ;
#122742 = DIRECTION ( 'NONE',  ( 0.000000000000000000, 0.000000000000000000, 1.000000000000000000 ) ) ;
#122743 = ORIENTED_EDGE ( 'NONE', *, *, #93943, .F. ) ;
#122745 = EDGE_CURVE ( 'NONE', #119361, #14309, #102134, .T. ) ;
#122744 = DIRECTION ( 'NONE',  ( 0.000000000000000000, 1.000000000000000000, 0.000000000000000000 ) ) ;
#122746 = ORIENTED_EDGE ( 'NONE', *, *, #73044, .T. ) ;
#122747 = LINE ( 'NONE', #22633, #92296 ) ;
#122748 = LINE ( 'NONE', #73005, #44856 ) ;
#122749 = ADVANCED_BREP_SHAPE_REPRESENTATION ( '', ( #57280, #108296 ), #106243 ) ;
#122750 = CARTESIAN_POINT ( 'NONE',  ( -2.100000000000033396, 2.500000000000000000, -3.637306695894650055 ) ) ;
#122751 = EDGE_CURVE ( 'NONE', #15438, #50878, #118848, .T. ) ;
#122752 = PLANE ( 'NONE',  #108628 ) ;
#122753 = EDGE_LOOP ( 'NONE', ( #82777, #123159, #122050, #41832 ) ) ;
#122754 = EDGE_CURVE ( 'NONE', #27176, #82484, #91662, .T. ) ;
#122755 = LINE ( 'NONE', #110351, #96931 ) ;
#122756 = CIRCLE ( 'NONE', #112298, 0.09999999999999982514 ) ;
#122757 = AXIS2_PLACEMENT_3D ( 'NONE', #78206, #28462, #38947 ) ;
#122758 = EDGE_CURVE ( 'NONE', #9515, #118519, #112506, .T. ) ;
#122759 = DIRECTION ( 'NONE',  ( 0.000000000000000000, 0.000000000000000000, 1.000000000000000000 ) ) ;
#122760 = ORIENTED_EDGE ( 'NONE', *, *, #7323, .T. ) ;
#122761 = ORIENTED_EDGE ( 'NONE', *, *, #98551, .T. ) ;
#122762 = ORIENTED_EDGE ( 'NONE', *, *, #59486, .T. ) ;
#122763 = FACE_OUTER_BOUND ( 'NONE', #48956, .T. ) ;
#122764 = DIRECTION ( 'NONE',  ( 0.000000000000000000, 0.000000000000000000, -1.000000000000000000 ) ) ;
#122765 = CARTESIAN_POINT ( 'NONE',  ( 186.8177083336747160, 4.367472073101515306, 7.564683531250000925 ) ) ;
#122766 = DIRECTION ( 'NONE',  ( 0.000000000000000000, 0.000000000000000000, 1.000000000000000000 ) ) ;
#122767 = EDGE_CURVE ( 'NONE', #45205, #76614, #33104, .T. ) ;
#122770 = AXIS2_PLACEMENT_3D ( 'NONE', #128270, #98781, #9121 ) ;
#122769 = DIRECTION ( 'NONE',  ( 0.000000000000000000, 1.000000000000000000, 0.000000000000000000 ) ) ;
#122768 = VECTOR ( 'NONE', #34609, 1000.000000000000000 ) ;
#122771 = CONICAL_SURFACE ( 'NONE', #39265, 0.1000000000000002554, 0.003490658503988666988 ) ;
#122772 = DIRECTION ( 'NONE',  ( 0.000000000000000000, -0.000000000000000000, 1.000000000000000000 ) ) ;
#122773 = CARTESIAN_POINT ( 'NONE',  ( -12.69999999999999396, 12.50000000000000000, -4.048810130592460865 ) ) ;
#122774 = CONICAL_SURFACE ( 'NONE', #9903, 0.1000000000000002554, 0.003490658503988666988 ) ;
#122775 = DIRECTION ( 'NONE',  ( 0.000000000000000000, 0.000000000000000000, -1.000000000000000000 ) ) ;
#122776 = VECTOR ( 'NONE', #42710, 1000.000000000000000 ) ;
#122777 = ORIENTED_EDGE ( 'NONE', *, *, #19538, .T. ) ;
#122778 = CARTESIAN_POINT ( 'NONE',  ( -4.250072516143177381E-14, 12.50000000000000000, -3.637306695894650055 ) ) ;
#122779 = DIRECTION ( 'NONE',  ( -0.000000000000000000, -1.000000000000000000, -0.000000000000000000 ) ) ;
#122780 = EDGE_CURVE ( 'NONE', #10245, #39901, #24407, .T. ) ;
#122781 = DIRECTION ( 'NONE',  ( 0.000000000000000000, -0.000000000000000000, 1.000000000000000000 ) ) ;
#122782 = CARTESIAN_POINT ( 'NONE',  ( 2.949999999999945111, 2.500000000000000000, 2.265063509461097357 ) ) ;
#122783 = EDGE_LOOP ( 'NONE', ( #5278, #54181, #3468, #89181 ) ) ;
#122784 = DIRECTION ( 'NONE',  ( -0.000000000000000000, 1.000000000000000000, -0.000000000000000000 ) ) ;
#122785 = CIRCLE ( 'NONE', #110258, 0.1000000000000002554 ) ;
#122786 = LINE ( 'NONE', #13462, #65958 ) ;
#122788 = EDGE_LOOP ( 'NONE', ( #29925, #66901 ) ) ;
#122787 = CARTESIAN_POINT ( 'NONE',  ( 2.099999999999950351, 2.500000000000000000, -2.276824562219559311E-15 ) ) ;
#122789 = AXIS2_PLACEMENT_3D ( 'NONE', #112262, #44152, #91321 ) ;
#122790 = AXIS2_PLACEMENT_3D ( 'NONE', #117050, #9703, #27383 ) ;
#122791 = VERTEX_POINT ( 'NONE', #64330 ) ;
#122792 = CONICAL_SURFACE ( 'NONE', #89347, 0.1000000000000002554, 0.003490658503988666988 ) ;
#122793 = DIRECTION ( 'NONE',  ( 0.000000000000000000, 0.000000000000000000, -1.000000000000000000 ) ) ;
#122794 = CIRCLE ( 'NONE', #68406, 0.06509327318403745899 ) ;
#122795 = EDGE_CURVE ( 'NONE', #98740, #68909, #45700, .T. ) ;
#122796 = ORIENTED_EDGE ( 'NONE', *, *, #46458, .F. ) ;
#122797 = ORIENTED_EDGE ( 'NONE', *, *, #65633, .T. ) ;
#122798 = DIRECTION ( 'NONE',  ( -0.000000000000000000, 1.000000000000000000, -0.000000000000000000 ) ) ;
#122799 = AXIS2_PLACEMENT_3D ( 'NONE', #116729, #15295, #27079 ) ;
#122800 = ORIENTED_EDGE ( 'NONE', *, *, #44800, .T. ) ;
#122801 = CARTESIAN_POINT ( 'NONE',  ( -5.200000000000024158, 2.500000000000000000, -4.676537180435977881 ) ) ;
#122802 = DIRECTION ( 'NONE',  ( -4.274815082592931898E-19, -0.9999939076577903929, -0.003490651415223739937 ) ) ;
#122803 = AXIS2_PLACEMENT_3D ( 'NONE', #24655, #95966, #116241 ) ;
#122804 = CARTESIAN_POINT ( 'NONE',  ( -6.050000000000020250, 2.500000000000000000, -6.841600689897078702 ) ) ;
#122805 = VERTEX_POINT ( 'NONE', #123255 ) ;
#122806 = AXIS2_PLACEMENT_3D ( 'NONE', #83792, #76557, #13749 ) ;
#122807 = AXIS2_PLACEMENT_3D ( 'NONE', #1891, #49731, #19608 ) ;
#122808 = DIRECTION ( 'NONE',  ( -0.000000000000000000, -1.000000000000000000, -0.000000000000000000 ) ) ;
#122810 = VERTEX_POINT ( 'NONE', #86542 ) ;
#122809 = DIRECTION ( 'NONE',  ( 1.000000000000000000, 0.000000000000000000, 0.000000000000000000 ) ) ;
#122811 = CARTESIAN_POINT ( 'NONE',  ( 17.41715230668771852, 1.872943439152341183, 4.643388583733590202 ) ) ;
#122812 = AXIS2_PLACEMENT_3D ( 'NONE', #109183, #10354, #19524 ) ;
#122813 = EDGE_CURVE ( 'NONE', #58229, #70966, #31048, .T. ) ;
#122814 = DIRECTION ( 'NONE',  ( 0.000000000000000000, 0.000000000000000000, -1.000000000000000000 ) ) ;
#122815 = ORIENTED_EDGE ( 'NONE', *, *, #26963, .F. ) ;
#122817 = AXIS2_PLACEMENT_3D ( 'NONE', #101297, #86461, #47202 ) ;
#122816 = AXIS2_PLACEMENT_3D ( 'NONE', #65080, #95216, #5517 ) ;
#122818 = ORIENTED_EDGE ( 'NONE', *, *, #98480, .F. ) ;
#122819 = EDGE_LOOP ( 'NONE', ( #110568, #127573, #107119, #80250 ) ) ;
#122820 = VERTEX_POINT ( 'NONE', #46616 ) ;
#122821 = DIRECTION ( 'NONE',  ( -0.000000000000000000, -1.000000000000000000, -0.000000000000000000 ) ) ;
#122822 = CARTESIAN_POINT ( 'NONE',  ( 13.51931942373995099, 2.499999999999999112, 8.074217332245385848 ) ) ;
#122823 =( BOUNDED_CURVE ( )  B_SPLINE_CURVE ( 2, ( #104650, #112565, #33999, #122384, #124954, #54278, #114480 ),
 .UNSPECIFIED., .F., .F. ) 
 B_SPLINE_CURVE_WITH_KNOTS ( ( 3, 2, 2, 3 ),
 ( 0.07142857142857149400, 0.09523809523809532995, 0.1190476190476191520, 0.1428571428571429880 ),
 .UNSPECIFIED. ) 
 CURVE ( )  GEOMETRIC_REPRESENTATION_ITEM ( )  RATIONAL_B_SPLINE_CURVE ( ( 0.9999999999999996669, 0.8660254037844390407, 1.000000000000000000, 0.8660254037844387076, 1.000000000000000000, 0.8660254037844379305, 1.000000000000000666 ) ) 
 REPRESENTATION_ITEM ( '' )  );
#122824 = DIRECTION ( 'NONE',  ( 0.000000000000000000, 0.000000000000000000, 1.000000000000000000 ) ) ;
#122825 = FACE_BOUND ( 'NONE', #62956, .T. ) ;
#122826 = ORIENTED_EDGE ( 'NONE', *, *, #54173, .T. ) ;
#122827 = CARTESIAN_POINT ( 'NONE',  ( 185.5312500006828031, 9.429780353434619030E-16, -7.700000000000000178 ) ) ;
#122828 = DIRECTION ( 'NONE',  ( -0.000000000000000000, 1.000000000000000000, -0.000000000000000000 ) ) ;
#122829 = DIRECTION ( 'NONE',  ( 0.000000000000000000, 1.000000000000000000, 0.000000000000000000 ) ) ;
#122830 = CARTESIAN_POINT ( 'NONE',  ( -6.450000000000019718, 2.500000000000000000, -1.818653347947326138 ) ) ;
#122831 = FACE_OUTER_BOUND ( 'NONE', #24940, .T. ) ;
#122832 = AXIS2_PLACEMENT_3D ( 'NONE', #35292, #115096, #25432 ) ;
#122833 = CARTESIAN_POINT ( 'NONE',  ( 3.749999999999975131, 2.500000000000000000, 6.495190528383297135 ) ) ;
#122834 = CARTESIAN_POINT ( 'NONE',  ( -8.550000000000011369, 2.500000000000000000, 1.918653347947321564 ) ) ;
#122835 = ADVANCED_FACE ( 'NONE', ( #7329 ), #64464, .T. ) ;
#122836 = EDGE_LOOP ( 'NONE', ( #10360, #19745 ) ) ;
#122837 = ORIENTED_EDGE ( 'NONE', *, *, #69347, .T. ) ;
#122838 = EDGE_LOOP ( 'NONE', ( #55130, #104216, #61344, #67733 ) ) ;
#122839 = ORIENTED_EDGE ( 'NONE', *, *, #117260, .T. ) ;
#122840 = EDGE_LOOP ( 'NONE', ( #7370, #66085, #62206, #76956 ) ) ;
#122841 = CARTESIAN_POINT ( 'NONE',  ( 12.29999999999990656, 12.50000000000000000, -4.676537180435977881 ) ) ;
#122842 = DIRECTION ( 'NONE',  ( 0.000000000000000000, 1.000000000000000000, 0.000000000000000000 ) ) ;
#122843 = VERTEX_POINT ( 'NONE', #108114 ) ;
#122844 = FACE_BOUND ( 'NONE', #74982, .T. ) ;
#122845 = CARTESIAN_POINT ( 'NONE',  ( 7.299999999999924327, 2.500000000000000000, 0.2464101615137735679 ) ) ;
#122846 = EDGE_CURVE ( 'NONE', #119087, #76531, #116644, .T. ) ;
#122847 = VECTOR ( 'NONE', #2146, 1000.000000000000000 ) ;
#122848 = VECTOR ( 'NONE', #121990, 1000.000000000000000 ) ;
#122849 = ORIENTED_EDGE ( 'NONE', *, *, #47067, .T. ) ;
#122850 = EDGE_CURVE ( 'NONE', #55169, #77714, #89125, .T. ) ;
#122851 = FACE_OUTER_BOUND ( 'NONE', #113246, .T. ) ;
#122852 = EDGE_CURVE ( 'NONE', #1184, #30745, #26994, .T. ) ;
#122853 = DIRECTION ( 'NONE',  ( 0.000000000000000000, 1.000000000000000000, 0.000000000000000000 ) ) ;
#122854 = EDGE_CURVE ( 'NONE', #92073, #126313, #16326, .T. ) ;
#122855 = FACE_OUTER_BOUND ( 'NONE', #109514, .T. ) ;
#122856 = EDGE_CURVE ( 'NONE', #1725, #95822, #97009, .T. ) ;
#122857 = ORIENTED_EDGE ( 'NONE', *, *, #37875, .F. ) ;
#122858 = LINE ( 'NONE', #92092, #57613 ) ;
#122859 = EDGE_LOOP ( 'NONE', ( #38308, #79878 ) ) ;
#122860 = AXIS2_PLACEMENT_3D ( 'NONE', #67481, #117226, #47241 ) ;
#122861 = CONICAL_SURFACE ( 'NONE', #49720, 0.1000000000000002554, 0.003490658503988666988 ) ;
#122862 = EDGE_CURVE ( 'NONE', #112423, #84654, #58230, .T. ) ;
#122863 = ORIENTED_EDGE ( 'NONE', *, *, #71564, .T. ) ;
#122864 = EDGE_CURVE ( 'NONE', #32927, #23200, #106238, .T. ) ;
#122865 = VERTEX_POINT ( 'NONE', #37463 ) ;
#122866 = DIRECTION ( 'NONE',  ( 0.000000000000000000, 1.000000000000000000, 0.000000000000000000 ) ) ;
#122867 = LINE ( 'NONE', #72483, #16302 ) ;
#122868 = CARTESIAN_POINT ( 'NONE',  ( -5.650000000000019895, 12.50000000000000000, 2.511473670974873507 ) ) ;
#122869 = ORIENTED_EDGE ( 'NONE', *, *, #75856, .F. ) ;
#122870 = EDGE_CURVE ( 'NONE', #35208, #49210, #107479, .T. ) ;
#122871 = DIRECTION ( 'NONE',  ( 0.000000000000000000, -0.9999939076577903929, 0.003490651415223739937 ) ) ;
#122872 = ADVANCED_FACE ( 'NONE', ( #126481 ), #99987, .T. ) ;
#122873 = AXIS2_PLACEMENT_3D ( 'NONE', #100780, #39956, #111239 ) ;
#122874 = FACE_OUTER_BOUND ( 'NONE', #20223, .T. ) ;
#122875 = EDGE_CURVE ( 'NONE', #48799, #37790, #27605, .T. ) ;
#122876 = CARTESIAN_POINT ( 'NONE',  ( -12.49999999999999289, 2.500000000000000000, 5.022947341949748790 ) ) ;
#122877 = CARTESIAN_POINT ( 'NONE',  ( 185.7395833340161460, 4.445597072760117285, 7.699999999999999289 ) ) ;
#122878 = ORIENTED_EDGE ( 'NONE', *, *, #30995, .T. ) ;
#122879 = CARTESIAN_POINT ( 'NONE',  ( 2.299999999999946976, 2.500000000000000000, 4.776537180435972196 ) ) ;
#122880 = EDGE_CURVE ( 'NONE', #124753, #76648, #78012, .T. ) ;
#122881 = ORIENTED_EDGE ( 'NONE', *, *, #58416, .F. ) ;
#122882 = DIRECTION ( 'NONE',  ( 0.000000000000000000, -0.000000000000000000, 1.000000000000000000 ) ) ;
#122883 = CONICAL_SURFACE ( 'NONE', #93633, 0.09999999999999982514, 0.003490658503988666988 ) ;
#122884 = ORIENTED_EDGE ( 'NONE', *, *, #10416, .T. ) ;
#122885 = ORIENTED_EDGE ( 'NONE', *, *, #78087, .F. ) ;
#122886 = CARTESIAN_POINT ( 'NONE',  ( 11.64999999999990798, 2.500000000000000000, 5.902370205355745192 ) ) ;
#122887 = AXIS2_PLACEMENT_3D ( 'NONE', #79251, #117857, #88392 ) ;
#122888 = DIRECTION ( 'NONE',  ( -0.000000000000000000, 1.000000000000000000, -0.000000000000000000 ) ) ;
#122889 = CARTESIAN_POINT ( 'NONE',  ( -5.400000000000020783, 12.50000000000000000, 0.6928203230275494784 ) ) ;
#122890 = DIRECTION ( 'NONE',  ( 0.000000000000000000, 0.000000000000000000, -1.000000000000000000 ) ) ;
#122892 = CIRCLE ( 'NONE', #81129, 0.1000000000000000472 ) ;
#122891 = DIRECTION ( 'NONE',  ( 0.000000000000000000, 1.000000000000000000, 0.000000000000000000 ) ) ;
#122893 = EDGE_LOOP ( 'NONE', ( #126158, #54444 ) ) ;
#122894 = VECTOR ( 'NONE', #115131, 1000.000000000000000 ) ;
#122895 = ORIENTED_EDGE ( 'NONE', *, *, #108983, .T. ) ;
#122896 = PLANE ( 'NONE',  #64220 ) ;
#122897 = AXIS2_PLACEMENT_3D ( 'NONE', #102361, #12661, #63069 ) ;
#122898 = DIRECTION ( 'NONE',  ( 0.000000000000000000, 1.000000000000000000, 0.000000000000000000 ) ) ;
#122899 = FACE_OUTER_BOUND ( 'NONE', #38115, .T. ) ;
#122900 = ORIENTED_EDGE ( 'NONE', *, *, #54126, .T. ) ;
#122901 = ORIENTED_EDGE ( 'NONE', *, *, #91088, .F. ) ;
#122902 = DIRECTION ( 'NONE',  ( 0.000000000000000000, -0.000000000000000000, 1.000000000000000000 ) ) ;
#122903 = CONICAL_SURFACE ( 'NONE', #9932, 0.1000000000000002554, 0.003490658503988666988 ) ;
#122904 = ORIENTED_EDGE ( 'NONE', *, *, #48870, .F. ) ;
#122905 = PLANE ( 'NONE',  #65417 ) ;
#122906 = CARTESIAN_POINT ( 'NONE',  ( -10.40000000000000213, 2.500000000000000000, -4.330127018922197202 ) ) ;
#122907 = CIRCLE ( 'NONE', #14121, 0.1000000000000002554 ) ;
#122908 = CARTESIAN_POINT ( 'NONE',  ( 1.849999999999949685, 12.50000000000000000, 1.818653347947321475 ) ) ;
#122909 = ORIENTED_EDGE ( 'NONE', *, *, #41928, .F. ) ;
#122910 = DIRECTION ( 'NONE',  ( 0.000000000000000000, -0.9999939076577903929, 0.003490651415223739937 ) ) ;
#122911 = CARTESIAN_POINT ( 'NONE',  ( 12.49999999999993605, 2.500000000000000000, -2.276824562219559311E-15 ) ) ;
#122912 = CARTESIAN_POINT ( 'NONE',  ( 9.149999999999918643, 12.50000000000000000, -6.495190528383302464 ) ) ;
#122913 = FACE_OUTER_BOUND ( 'NONE', #87108, .T. ) ;
#122914 = AXIS2_PLACEMENT_3D ( 'NONE', #117546, #48192, #37095 ) ;
#122915 = DIRECTION ( 'NONE',  ( 0.000000000000000000, -0.000000000000000000, 1.000000000000000000 ) ) ;
#122916 = ORIENTED_EDGE ( 'NONE', *, *, #49537, .T. ) ;
#122917 = ADVANCED_FACE ( 'NONE', ( #18451 ), #98288, .T. ) ;
#122918 = DIRECTION ( 'NONE',  ( 0.000000000000000000, 0.000000000000000000, -1.000000000000000000 ) ) ;
#122920 = AXIS2_PLACEMENT_3D ( 'NONE', #86799, #25284, #125440 ) ;
#122919 = AXIS2_PLACEMENT_3D ( 'NONE', #2805, #20526, #101664 ) ;
#122922 = EDGE_CURVE ( 'NONE', #20150, #88083, #52057, .T. ) ;
#122921 = DIRECTION ( 'NONE',  ( 0.000000000000000000, 1.000000000000000000, 0.000000000000000000 ) ) ;
#122923 = ORIENTED_EDGE ( 'NONE', *, *, #36547, .F. ) ;
#122924 = ORIENTED_EDGE ( 'NONE', *, *, #108437, .F. ) ;
#122925 = CARTESIAN_POINT ( 'NONE',  ( 184.2343750003414016, 8.734944146203032389, 5.348610694689227483E-16 ) ) ;
#122926 = CARTESIAN_POINT ( 'NONE',  ( 14.34999999999989306, 2.500000000000000000, -1.718653347947326049 ) ) ;
#122927 = CARTESIAN_POINT ( 'NONE',  ( -1.700000000000035261, 2.500000000000000000, 4.230127018922196669 ) ) ;
#122928 = DIRECTION ( 'NONE',  ( -0.000000000000000000, -1.000000000000000000, -0.000000000000000000 ) ) ;
#122929 = EDGE_CURVE ( 'NONE', #81018, #123846, #118573, .T. ) ;
#122930 = DIRECTION ( 'NONE',  ( 0.000000000000000000, 0.000000000000000000, 1.000000000000000000 ) ) ;
#122931 = DIRECTION ( 'NONE',  ( 0.000000000000000000, 1.000000000000000000, 0.000000000000000000 ) ) ;
#122932 = DIRECTION ( 'NONE',  ( 0.000000000000000000, 0.000000000000000000, 1.000000000000000000 ) ) ;
#122933 = CARTESIAN_POINT ( 'NONE',  ( 11.24999999999990585, 12.50000000000000000, 2.857883832488649301 ) ) ;
#122934 = LINE ( 'NONE', #65276, #108387 ) ;
#122935 = DIRECTION ( 'NONE',  ( 0.000000000000000000, -0.000000000000000000, 1.000000000000000000 ) ) ;
#122936 = EDGE_LOOP ( 'NONE', ( #41279, #15648, #35324, #116603 ) ) ;
#122937 = EDGE_LOOP ( 'NONE', ( #29707, #26194, #44754, #67743 ) ) ;
#122938 = VERTEX_POINT ( 'NONE', #59024 ) ;
#122939 = CONICAL_SURFACE ( 'NONE', #12186, 0.1000000000000000472, 0.003490658503988666988 ) ;
#122940 = CONICAL_SURFACE ( 'NONE', #3801, 0.1000000000000002554, 0.003490658503988666988 ) ;
#122941 = ORIENTED_EDGE ( 'NONE', *, *, #122387, .F. ) ;
#122942 = CARTESIAN_POINT ( 'NONE',  ( 11.64999999999990443, 12.50000000000000000, 2.857883832488649301 ) ) ;
#122943 = DIRECTION ( 'NONE',  ( 0.000000000000000000, 0.000000000000000000, -1.000000000000000000 ) ) ;
#122944 = EDGE_LOOP ( 'NONE', ( #74606, #107182, #55501, #77227 ) ) ;
#122945 = VECTOR ( 'NONE', #25646, 1000.000000000000000 ) ;
#122946 = CARTESIAN_POINT ( 'NONE',  ( 4.349999999999938360, 2.500000000000000000, 1.818653347947321475 ) ) ;
#122947 = CIRCLE ( 'NONE', #37180, 0.06509327318403745899 ) ;
#122948 = DIRECTION ( 'NONE',  ( -4.274815082592931898E-19, -0.9999939076577903929, -0.003490651415223739937 ) ) ;
#122950 = ORIENTED_EDGE ( 'NONE', *, *, #79295, .T. ) ;
#122949 = CARTESIAN_POINT ( 'NONE',  ( 184.5312500006828031, 9.429780353434619030E-16, -7.700000000000000178 ) ) ;
#122951 = DIRECTION ( 'NONE',  ( 0.000000000000000000, 0.000000000000000000, 1.000000000000000000 ) ) ;
#122952 = CIRCLE ( 'NONE', #49806, 0.06509327318403745899 ) ;
#122953 = DIRECTION ( 'NONE',  ( 0.000000000000000000, -0.9999939076577903929, 0.003490651415223739937 ) ) ;
#122954 = ORIENTED_EDGE ( 'NONE', *, *, #4770, .F. ) ;
#122955 = AXIS2_PLACEMENT_3D ( 'NONE', #111989, #3315, #123094 ) ;
#122956 = ORIENTED_EDGE ( 'NONE', *, *, #36254, .T. ) ;
#122957 = ORIENTED_EDGE ( 'NONE', *, *, #45197, .F. ) ;
#122958 = EDGE_LOOP ( 'NONE', ( #1947, #124777, #99474, #74850 ) ) ;
#122959 = FACE_OUTER_BOUND ( 'NONE', #119444, .T. ) ;
#122960 = DIRECTION ( 'NONE',  ( 0.000000000000000000, 0.000000000000000000, -1.000000000000000000 ) ) ;
#122961 = CARTESIAN_POINT ( 'NONE',  ( 13.94999999999989626, 12.50000000000000000, 2.576566944158910744 ) ) ;
#122962 = DIRECTION ( 'NONE',  ( -0.000000000000000000, -1.000000000000000000, -0.000000000000000000 ) ) ;
#122963 = AXIS2_PLACEMENT_3D ( 'NONE', #56198, #76502, #77141 ) ;
#122964 = VERTEX_POINT ( 'NONE', #98946 ) ;
#122965 = CARTESIAN_POINT ( 'NONE',  ( -2.900000000000030109, 12.50000000000000000, -3.572213422710612374 ) ) ;
#122967 = VERTEX_POINT ( 'NONE', #69471 ) ;
#122966 = ADVANCED_FACE ( 'NONE', ( #9279 ), #45797, .T. ) ;
#122968 = VECTOR ( 'NONE', #77377, 1000.000000000000000 ) ;
#122969 = LINE ( 'NONE', #23470, #85197 ) ;
#122970 = DIRECTION ( 'NONE',  ( -0.000000000000000000, 1.000000000000000000, -0.000000000000000000 ) ) ;
#122971 = FACE_OUTER_BOUND ( 'NONE', #78458, .T. ) ;
#122972 = DIRECTION ( 'NONE',  ( 0.000000000000000000, 0.000000000000000000, 1.000000000000000000 ) ) ;
#122973 = EDGE_CURVE ( 'NONE', #29920, #28513, #43652, .T. ) ;
#122974 = ORIENTED_EDGE ( 'NONE', *, *, #13986, .T. ) ;
#122975 = CIRCLE ( 'NONE', #33109, 0.06509327318403745899 ) ;
#122976 = VECTOR ( 'NONE', #38216, 1000.000000000000000 ) ;
#122977 = ORIENTED_EDGE ( 'NONE', *, *, #101753, .F. ) ;
#122978 = VERTEX_POINT ( 'NONE', #10545 ) ;
#122979 = CARTESIAN_POINT ( 'NONE',  ( -3.150000000000029665, 2.500000000000000000, 6.841600689897072485 ) ) ;
#122980 = CARTESIAN_POINT ( 'NONE',  ( -5.850000000000019185, 2.500000000000000000, 2.065063509461097624 ) ) ;
#122981 = EDGE_CURVE ( 'NONE', #28898, #105571, #100073, .T. ) ;
#122982 = DIRECTION ( 'NONE',  ( 0.000000000000000000, 1.000000000000000000, 0.000000000000000000 ) ) ;
#122983 = FACE_BOUND ( 'NONE', #35693, .T. ) ;
#122984 = CARTESIAN_POINT ( 'NONE',  ( 10.84999999999991260, 12.50000000000000000, 5.802370205355744659 ) ) ;
#122985 = DIRECTION ( 'NONE',  ( 0.000000000000000000, 0.000000000000000000, 1.000000000000000000 ) ) ;
#122986 = AXIS2_PLACEMENT_3D ( 'NONE', #17594, #21980, #80890 ) ;
#122987 = CARTESIAN_POINT ( 'NONE',  ( -12.69999999999999396, 2.500000000000000000, 0.4464101615137776591 ) ) ;
#122988 = CONICAL_SURFACE ( 'NONE', #77008, 0.1000000000000002554, 0.003490658503988666988 ) ;
#122989 = CARTESIAN_POINT ( 'NONE',  ( 187.4218750003414016, 0.000000000000000000, 7.564683531250000925 ) ) ;
#122990 = DIRECTION ( 'NONE',  ( -0.000000000000000000, -1.000000000000000000, -0.000000000000000000 ) ) ;
#122991 = AXIS2_PLACEMENT_3D ( 'NONE', #127056, #114638, #46538 ) ;
#122992 = LINE ( 'NONE', #113160, #9293 ) ;
#122993 = ORIENTED_EDGE ( 'NONE', *, *, #127512, .T. ) ;
#122994 = DIRECTION ( 'NONE',  ( 0.000000000000000000, 0.000000000000000000, -1.000000000000000000 ) ) ;
#122995 = ADVANCED_FACE ( 'NONE', ( #32157 ), #101527, .T. ) ;
#122996 = VERTEX_POINT ( 'NONE', #111997 ) ;
#122997 = VERTEX_POINT ( 'NONE', #81246 ) ;
#122998 = VECTOR ( 'NONE', #66642, 1000.000000000000000 ) ;
#122999 = CARTESIAN_POINT ( 'NONE',  ( 133.2169897921533845, 2.500000000000000000, -0.01898911740318533561 ) ) ;
#123000 = FACE_BOUND ( 'NONE', #12302, .T. ) ;
#123001 = CARTESIAN_POINT ( 'NONE',  ( -4.550000000000026468, 2.500000000000000000, -6.495190528383302464 ) ) ;
#123002 = ADVANCED_FACE ( 'NONE', ( #121161 ), #95954, .T. ) ;
#123004 = AXIS2_PLACEMENT_3D ( 'NONE', #33472, #113297, #11870 ) ;
#123003 = AXIS2_PLACEMENT_3D ( 'NONE', #63348, #122921, #92820 ) ;
#123005 = ORIENTED_EDGE ( 'NONE', *, *, #75693, .F. ) ;
#123006 = EDGE_CURVE ( 'NONE', #114427, #56742, #64555, .T. ) ;
#123007 = CARTESIAN_POINT ( 'NONE',  ( 59.88087687670552128, 3.776023963378999149, 4.996435080099743686 ) ) ;
#123008 = EDGE_CURVE ( 'NONE', #50768, #29262, #125203, .T. ) ;
#123009 = LINE ( 'NONE', #73257, #93859 ) ;
#123010 = EDGE_CURVE ( 'NONE', #28226, #108826, #8121, .T. ) ;
#123011 = EDGE_CURVE ( 'NONE', #104378, #118365, #84294, .T. ) ;
#123012 = EDGE_LOOP ( 'NONE', ( #16290, #46159 ) ) ;
#123013 = LINE ( 'NONE', #33362, #46933 ) ;
#123014 = FACE_OUTER_BOUND ( 'NONE', #65151, .T. ) ;
#123015 = EDGE_CURVE ( 'NONE', #7925, #4623, #26907, .T. ) ;
#123016 = EDGE_LOOP ( 'NONE', ( #49418, #51063 ) ) ;
#123017 = VECTOR ( 'NONE', #93543, 1000.000000000000000 ) ;
#123018 = CARTESIAN_POINT ( 'NONE',  ( 185.5312500006828031, 9.429780353434619030E-16, -7.700000000000000178 ) ) ;
#123019 = EDGE_CURVE ( 'NONE', #76567, #72606, #41604, .T. ) ;
#123020 = DIRECTION ( 'NONE',  ( 0.000000000000000000, -0.000000000000000000, 1.000000000000000000 ) ) ;
#123021 = EDGE_LOOP ( 'NONE', ( #19613, #104034 ) ) ;
#123022 = AXIS2_PLACEMENT_3D ( 'NONE', #80611, #118579, #68842 ) ;
#123023 = DIRECTION ( 'NONE',  ( 0.000000000000000000, 0.000000000000000000, -1.000000000000000000 ) ) ;
#123024 = ADVANCED_FACE ( 'NONE', ( #30870 ), #94117, .T. ) ;
#123025 = VECTOR ( 'NONE', #64151, 1000.000000000000000 ) ;
#123026 = DIRECTION ( 'NONE',  ( -0.000000000000000000, -1.000000000000000000, -0.000000000000000000 ) ) ;
#123027 = CIRCLE ( 'NONE', #47818, 0.06509327318403741736 ) ;
#123028 = DIRECTION ( 'NONE',  ( 0.000000000000000000, -0.000000000000000000, 1.000000000000000000 ) ) ;
#123029 = ORIENTED_EDGE ( 'NONE', *, *, #57991, .T. ) ;
#123030 = VERTEX_POINT ( 'NONE', #11194 ) ;
#123031 = EDGE_CURVE ( 'NONE', #113064, #56167, #112603, .T. ) ;
#123032 = DIRECTION ( 'NONE',  ( 0.000000000000000000, 1.000000000000000000, 0.000000000000000000 ) ) ;
#123033 = EDGE_CURVE ( 'NONE', #27106, #129486, #70141, .T. ) ;
#123035 = VERTEX_POINT ( 'NONE', #60946 ) ;
#123034 = VECTOR ( 'NONE', #8874, 1000.000000000000000 ) ;
#123036 = CARTESIAN_POINT ( 'NONE',  ( -5.400000000000020783, 12.50000000000000000, 5.022947341949748790 ) ) ;
#123037 = LINE ( 'NONE', #43848, #20139 ) ;
#123038 = CONICAL_SURFACE ( 'NONE', #62410, 0.1000000000000002554, 0.003490658503988666988 ) ;
#123039 = EDGE_LOOP ( 'NONE', ( #11277, #51707, #104503, #24964 ) ) ;
#123040 = CARTESIAN_POINT ( 'NONE',  ( -0.6500000000000398792, 12.50000000000000000, -2.511473670974877948 ) ) ;
#123041 = DIRECTION ( 'NONE',  ( 0.000000000000000000, 0.000000000000000000, -1.000000000000000000 ) ) ;
#123042 = LINE ( 'NONE', #41910, #6793 ) ;
#123043 = DIRECTION ( 'NONE',  ( 0.000000000000000000, -0.9999939076577903929, 0.003490651415223739937 ) ) ;
#123044 = CARTESIAN_POINT ( 'NONE',  ( -11.64999999999999680, 2.500000000000000000, 6.495190528383297135 ) ) ;
#123045 = ORIENTED_EDGE ( 'NONE', *, *, #34383, .F. ) ;
#123047 = VERTEX_POINT ( 'NONE', #1375 ) ;
#123046 = CONICAL_SURFACE ( 'NONE', #120989, 0.1000000000000002554, 0.003490658503988666988 ) ;
#123048 = LINE ( 'NONE', #72020, #13948 ) ;
#123049 = VERTEX_POINT ( 'NONE', #51149 ) ;
#123050 = DIRECTION ( 'NONE',  ( 0.000000000000000000, 1.000000000000000000, 0.000000000000000000 ) ) ;
#123052 = ORIENTED_EDGE ( 'NONE', *, *, #55869, .F. ) ;
#123051 = ORIENTED_EDGE ( 'NONE', *, *, #326, .F. ) ;
#123053 = ORIENTED_EDGE ( 'NONE', *, *, #124067, .F. ) ;
#123054 = DIRECTION ( 'NONE',  ( -0.000000000000000000, -1.000000000000000000, -0.000000000000000000 ) ) ;
#123056 = DIRECTION ( 'NONE',  ( 0.000000000000000000, 1.000000000000000000, 0.000000000000000000 ) ) ;
#123055 = CIRCLE ( 'NONE', #108461, 0.06509327318403745899 ) ;
#123057 = DIRECTION ( 'NONE',  ( 0.000000000000000000, -0.000000000000000000, 1.000000000000000000 ) ) ;
#123058 = DIRECTION ( 'NONE',  ( 0.000000000000000000, 0.000000000000000000, 1.000000000000000000 ) ) ;
#123059 = LINE ( 'NONE', #13076, #48173 ) ;
#123060 = CIRCLE ( 'NONE', #62430, 0.06509327318403745899 ) ;
#123061 = LINE ( 'NONE', #113887, #65273 ) ;
#123062 = DIRECTION ( 'NONE',  ( 0.000000000000000000, 1.000000000000000000, 0.000000000000000000 ) ) ;
#123063 = AXIS2_PLACEMENT_3D ( 'NONE', #45031, #47604, #104577 ) ;
#123064 = DIRECTION ( 'NONE',  ( 0.000000000000000000, 0.000000000000000000, 1.000000000000000000 ) ) ;
#123065 = DIRECTION ( 'NONE',  ( 0.000000000000000000, 1.000000000000000000, 0.000000000000000000 ) ) ;
#123066 = EDGE_LOOP ( 'NONE', ( #38259, #122640, #105812, #3425 ) ) ;
#123067 = ADVANCED_FACE ( 'NONE', ( #54200 ), #110530, .T. ) ;
#123068 =( GEOMETRIC_REPRESENTATION_CONTEXT ( 3 ) GLOBAL_UNCERTAINTY_ASSIGNED_CONTEXT ( ( #105543 ) ) GLOBAL_UNIT_ASSIGNED_CONTEXT ( ( #103418, #114508, #75878 ) ) REPRESENTATION_CONTEXT ( 'NONE', 'WORKASPACE' ) );
#123069 = EDGE_CURVE ( 'NONE', #16889, #19644, #33192, .T. ) ;
#123070 = CARTESIAN_POINT ( 'NONE',  ( 9.999999999999948486, 2.500000000000000000, -4.430127018922202176 ) ) ;
#123071 = EDGE_LOOP ( 'NONE', ( #89836, #793 ) ) ;
#123072 = ORIENTED_EDGE ( 'NONE', *, *, #70132, .F. ) ;
#123073 = DIRECTION ( 'NONE',  ( 0.000000000000000000, 0.000000000000000000, 1.000000000000000000 ) ) ;
#123074 = DIRECTION ( 'NONE',  ( -0.000000000000000000, 1.000000000000000000, -0.000000000000000000 ) ) ;
#123075 = CIRCLE ( 'NONE', #26926, 0.1000000000000002554 ) ;
#123076 = DIRECTION ( 'NONE',  ( -0.000000000000000000, 1.000000000000000000, -0.000000000000000000 ) ) ;
#123078 = CIRCLE ( 'NONE', #47869, 0.09999999999999999167 ) ;
#123077 = DIRECTION ( 'NONE',  ( 0.000000000000000000, 1.000000000000000000, 0.000000000000000000 ) ) ;
#123079 = DIRECTION ( 'NONE',  ( -0.000000000000000000, 1.000000000000000000, -0.000000000000000000 ) ) ;
#123080 = DIRECTION ( 'NONE',  ( -0.000000000000000000, 1.000000000000000000, -0.000000000000000000 ) ) ;
#123081 = CARTESIAN_POINT ( 'NONE',  ( -3.550000000000028244, 2.500000000000000000, 2.511473670974873507 ) ) ;
#123082 = VERTEX_POINT ( 'NONE', #121795 ) ;
#123083 = DIRECTION ( 'NONE',  ( 0.000000000000000000, -0.9999939076577903929, 0.003490651415223739937 ) ) ;
#123084 = AXIS2_PLACEMENT_3D ( 'NONE', #103075, #13395, #104991 ) ;
#123085 = DIRECTION ( 'NONE',  ( 0.000000000000000000, 0.000000000000000000, -1.000000000000000000 ) ) ;
#123086 = ORIENTED_EDGE ( 'NONE', *, *, #55037, .F. ) ;
#123087 = ORIENTED_EDGE ( 'NONE', *, *, #35679, .T. ) ;
#123089 = AXIS2_PLACEMENT_3D ( 'NONE', #62144, #119751, #70654 ) ;
#123088 = AXIS2_PLACEMENT_3D ( 'NONE', #40700, #70774, #60948 ) ;
#123090 = VERTEX_POINT ( 'NONE', #34575 ) ;
#123091 = VECTOR ( 'NONE', #113020, 1000.000000000000000 ) ;
#123092 = ORIENTED_EDGE ( 'NONE', *, *, #10518, .F. ) ;
#123093 = DIRECTION ( 'NONE',  ( 1.000000000000000000, 0.000000000000000000, 0.000000000000000000 ) ) ;
#123094 = DIRECTION ( 'NONE',  ( 0.000000000000000000, -0.000000000000000000, 1.000000000000000000 ) ) ;
#123096 = AXIS2_PLACEMENT_3D ( 'NONE', #75147, #82412, #122330 ) ;
#123095 = VECTOR ( 'NONE', #33039, 1000.000000000000000 ) ;
#123097 = CARTESIAN_POINT ( 'NONE',  ( 4.199999999999941558, 2.500000000000000000, -4.330127018922201643 ) ) ;
#123098 = CARTESIAN_POINT ( 'NONE',  ( 7.299999999999926104, 12.50000000000000000, -3.918623584224389056 ) ) ;
#123099 = DIRECTION ( 'NONE',  ( 0.000000000000000000, 1.000000000000000000, 0.000000000000000000 ) ) ;
#123100 = ORIENTED_EDGE ( 'NONE', *, *, #58048, .T. ) ;
#123101 = DIRECTION ( 'NONE',  ( 0.000000000000000000, 0.000000000000000000, 1.000000000000000000 ) ) ;
#123102 = CARTESIAN_POINT ( 'NONE',  ( -12.69999999999999218, 12.50000000000000000, -4.611443907251937091 ) ) ;
#123103 = FACE_OUTER_BOUND ( 'NONE', #18800, .T. ) ;
#123104 = DIRECTION ( 'NONE',  ( 0.000000000000000000, 0.000000000000000000, -1.000000000000000000 ) ) ;
#123105 = EDGE_CURVE ( 'NONE', #119556, #87886, #74481, .T. ) ;
#123106 = ORIENTED_EDGE ( 'NONE', *, *, #124039, .T. ) ;
#123107 = ORIENTED_EDGE ( 'NONE', *, *, #64731, .T. ) ;
#123108 = ORIENTED_EDGE ( 'NONE', *, *, #5771, .F. ) ;
#123109 = AXIS2_PLACEMENT_3D ( 'NONE', #105940, #77128, #16243 ) ;
#123110 = CARTESIAN_POINT ( 'NONE',  ( -6.650000000000018119, 2.500000000000000000, -6.395190528383301931 ) ) ;
#123111 = DIRECTION ( 'NONE',  ( -4.274815082592931898E-19, -0.9999939076577903929, -0.003490651415223739937 ) ) ;
#123113 = EDGE_CURVE ( 'NONE', #22205, #110118, #114729, .T. ) ;
#123112 = DIRECTION ( 'NONE',  ( -0.000000000000000000, -1.000000000000000000, -0.000000000000000000 ) ) ;
#123114 = CONICAL_SURFACE ( 'NONE', #74993, 0.09999999999999982514, 0.003490658503988666988 ) ;
#123115 = CIRCLE ( 'NONE', #66658, 0.1000000000000002554 ) ;
#123117 = ORIENTED_EDGE ( 'NONE', *, *, #40558, .F. ) ;
#123116 = ADVANCED_FACE ( 'NONE', ( #84937 ), #54099, .T. ) ;
#123118 = DIRECTION ( 'NONE',  ( 0.000000000000000000, 0.000000000000000000, -1.000000000000000000 ) ) ;
#123119 = CARTESIAN_POINT ( 'NONE',  ( -7.500000000000016875, 2.500000000000000000, -3.537306695894649966 ) ) ;
#123120 = CARTESIAN_POINT ( 'NONE',  ( 5.799999999999934985, 2.500000000000000000, -4.330127018922201643 ) ) ;
#123121 = ADVANCED_FACE ( 'NONE', ( #65934 ), #35215, .T. ) ;
#123122 = CARTESIAN_POINT ( 'NONE',  ( -11.05000000000000071, 2.500000000000000000, 6.741600689897071952 ) ) ;
#123123 = AXIS2_PLACEMENT_3D ( 'NONE', #10083, #50034, #80767 ) ;
#123124 = CIRCLE ( 'NONE', #24829, 0.06509327318403745899 ) ;
#123125 = AXIS2_PLACEMENT_3D ( 'NONE', #85545, #75716, #70424 ) ;
#123126 = DIRECTION ( 'NONE',  ( -0.000000000000000000, -1.000000000000000000, -0.000000000000000000 ) ) ;
#123127 = EDGE_LOOP ( 'NONE', ( #31225, #93798 ) ) ;
#123128 = EDGE_LOOP ( 'NONE', ( #124015, #86149 ) ) ;
#123129 = EDGE_CURVE ( 'NONE', #113061, #86174, #62528, .T. ) ;
#123130 = CARTESIAN_POINT ( 'NONE',  ( -1.050000000000038236, 2.500000000000000000, -6.048780366869526581 ) ) ;
#123131 = DIRECTION ( 'NONE',  ( -0.000000000000000000, 1.000000000000000000, -0.000000000000000000 ) ) ;
#123132 = CIRCLE ( 'NONE', #79330, 0.06509327318403745899 ) ;
#123133 = CARTESIAN_POINT ( 'NONE',  ( 21.23528140090977345, 2.699413673072321718, -2.293764360948945757 ) ) ;
#123134 = DIRECTION ( 'NONE',  ( -4.274815082592931898E-19, -0.9999939076577903929, -0.003490651415223739937 ) ) ;
#123135 = CARTESIAN_POINT ( 'NONE',  ( 10.19999999999991580, 2.500000000000000000, -0.4464101615137783252 ) ) ;
#123136 = VECTOR ( 'NONE', #23440, 1000.000000000000000 ) ;
#123137 = ORIENTED_EDGE ( 'NONE', *, *, #105591, .F. ) ;
#123138 = ORIENTED_EDGE ( 'NONE', *, *, #70827, .T. ) ;
#123139 = DIRECTION ( 'NONE',  ( -0.000000000000000000, 1.000000000000000000, -0.000000000000000000 ) ) ;
#123140 = DIRECTION ( 'NONE',  ( 0.000000000000000000, -0.000000000000000000, 1.000000000000000000 ) ) ;
#123141 = DIRECTION ( 'NONE',  ( 0.000000000000000000, 1.000000000000000000, 0.000000000000000000 ) ) ;
#123142 = DIRECTION ( 'NONE',  ( -0.000000000000000000, 1.000000000000000000, -0.000000000000000000 ) ) ;
#123143 = CARTESIAN_POINT ( 'NONE',  ( -12.69999999999999218, 2.500000000000000000, 4.576537180435972019 ) ) ;
#123144 = EDGE_LOOP ( 'NONE', ( #17871, #79158, #85008, #9260 ) ) ;
#123145 = AXIS2_PLACEMENT_3D ( 'NONE', #30329, #61049, #70880 ) ;
#123146 = DIRECTION ( 'NONE',  ( 0.000000000000000000, 0.000000000000000000, -1.000000000000000000 ) ) ;
#123147 = CARTESIAN_POINT ( 'NONE',  ( -9.350000000000004974, 2.500000000000000000, 6.741600689897071952 ) ) ;
#123148 = AXIS2_PLACEMENT_3D ( 'NONE', #40368, #67867, #18770 ) ;
#123149 = ORIENTED_EDGE ( 'NONE', *, *, #119429, .T. ) ;
#123150 = DIRECTION ( 'NONE',  ( 0.000000000000000000, 1.000000000000000000, 0.000000000000000000 ) ) ;
#123151 = ORIENTED_EDGE ( 'NONE', *, *, #32015, .F. ) ;
#123152 = DIRECTION ( 'NONE',  ( -0.000000000000000000, -1.000000000000000000, -0.000000000000000000 ) ) ;
#123153 = EDGE_CURVE ( 'NONE', #4134, #33730, #124872, .T. ) ;
#123154 = ORIENTED_EDGE ( 'NONE', *, *, #83833, .T. ) ;
#123155 = AXIS2_PLACEMENT_3D ( 'NONE', #3629, #31812, #112304 ) ;
#123156 = DIRECTION ( 'NONE',  ( 0.000000000000000000, 0.000000000000000000, 1.000000000000000000 ) ) ;
#123157 = DIRECTION ( 'NONE',  ( 0.000000000000000000, 0.000000000000000000, -1.000000000000000000 ) ) ;
#123158 = ORIENTED_EDGE ( 'NONE', *, *, #40337, .F. ) ;
#123159 = ORIENTED_EDGE ( 'NONE', *, *, #23139, .T. ) ;
#123160 = EDGE_CURVE ( 'NONE', #9507, #37294, #16811, .T. ) ;
#123161 = CARTESIAN_POINT ( 'NONE',  ( 184.6302083336747444, -4.367472073101514418, -7.564683531250002702 ) ) ;
#123162 = CARTESIAN_POINT ( 'NONE',  ( -4.800000000000022915, 12.50000000000000000, -0.3464101615137783474 ) ) ;
#123163 = VECTOR ( 'NONE', #26965, 1000.000000000000000 ) ;
#123164 = EDGE_CURVE ( 'NONE', #89915, #58166, #76417, .T. ) ;
#123165 = CARTESIAN_POINT ( 'NONE',  ( 187.0052083336747444, -6.551208109652278289, 3.782341765624995134 ) ) ;
#123166 = CARTESIAN_POINT ( 'NONE',  ( 184.1093750003413732, 9.264065473108010111E-16, -7.564683531250000925 ) ) ;
#123167 = CIRCLE ( 'NONE', #129458, 0.1000000000000002554 ) ;
#123168 = DIRECTION ( 'NONE',  ( 0.000000000000000000, -0.000000000000000000, 1.000000000000000000 ) ) ;
#123169 = CARTESIAN_POINT ( 'NONE',  ( 8.149999999999920419, 2.500000000000000000, 6.148780366869520897 ) ) ;
#123170 = EDGE_CURVE ( 'NONE', #64066, #378, #127273, .T. ) ;
#123171 = EDGE_CURVE ( 'NONE', #119497, #54885, #22819, .T. ) ;
#123172 = DIRECTION ( 'NONE',  ( -0.000000000000000000, 1.000000000000000000, -0.000000000000000000 ) ) ;
#123173 = CARTESIAN_POINT ( 'NONE',  ( -11.44999999999999751, 2.500000000000000000, 2.511473670974873507 ) ) ;
#123174 = CIRCLE ( 'NONE', #35351, 0.1000000000000000472 ) ;
#123175 = EDGE_CURVE ( 'NONE', #79817, #20424, #66609, .T. ) ;
#123176 = ADVANCED_FACE ( 'NONE', ( #46293 ), #47849, .T. ) ;
#123177 = ORIENTED_EDGE ( 'NONE', *, *, #54434, .F. ) ;
#123178 = EDGE_LOOP ( 'NONE', ( #44747, #59065 ) ) ;
#123179 = DIRECTION ( 'NONE',  ( 0.000000000000000000, 1.000000000000000000, 0.000000000000000000 ) ) ;
#123181 = ADVANCED_FACE ( 'NONE', ( #106511 ), #104273, .T. ) ;
#123180 = CIRCLE ( 'NONE', #20770, 0.1000000000000002554 ) ;
#123182 = ORIENTED_EDGE ( 'NONE', *, *, #50333, .F. ) ;
#123183 = CARTESIAN_POINT ( 'NONE',  ( 1.849999999999949019, 2.500000000000000000, 6.841600689897072485 ) ) ;
#123184 = PLANE ( 'NONE',  #1052 ) ;
#123185 = DIRECTION ( 'NONE',  ( 0.000000000000000000, 0.000000000000000000, -1.000000000000000000 ) ) ;
#123186 = AXIS2_PLACEMENT_3D ( 'NONE', #74237, #2928, #62501 ) ;
#123188 = ORIENTED_EDGE ( 'NONE', *, *, #76033, .F. ) ;
#123187 = ORIENTED_EDGE ( 'NONE', *, *, #60253, .F. ) ;
#123189 = FACE_BOUND ( 'NONE', #82560, .T. ) ;
#123190 = ORIENTED_EDGE ( 'NONE', *, *, #29087, .T. ) ;
#123191 = CARTESIAN_POINT ( 'NONE',  ( -9.400000000000009237, 2.500000000000000000, -3.883716857408422207 ) ) ;
#123192 = DIRECTION ( 'NONE',  ( -0.000000000000000000, 1.000000000000000000, -0.000000000000000000 ) ) ;
#123193 = EDGE_CURVE ( 'NONE', #70406, #104107, #25355, .T. ) ;
#123194 = CARTESIAN_POINT ( 'NONE',  ( -10.20000000000000462, 2.500000000000000000, 0.2464101615137735679 ) ) ;
#123197 = CARTESIAN_POINT ( 'NONE',  ( 4.399999999999937295, 2.500000000000000000, 4.676537180435972552 ) ) ;
#123196 = AXIS2_PLACEMENT_3D ( 'NONE', #29917, #40390, #80311 ) ;
#123195 = AXIS2_PLACEMENT_3D ( 'NONE', #45658, #23414, #25342 ) ;
#123198 = LINE ( 'NONE', #36100, #20068 ) ;
#123199 = DIRECTION ( 'NONE',  ( -0.000000000000000000, -1.000000000000000000, -0.000000000000000000 ) ) ;
#123200 = CARTESIAN_POINT ( 'NONE',  ( 12.09999999999990550, 2.500000000000000000, -4.330127018922201643 ) ) ;
#123201 = CARTESIAN_POINT ( 'NONE',  ( 8.349999999999923261, 2.500000000000000000, 2.957883832488649389 ) ) ;
#123202 = DIRECTION ( 'NONE',  ( -0.000000000000000000, 1.000000000000000000, -0.000000000000000000 ) ) ;
#123203 = DIRECTION ( 'NONE',  ( 0.000000000000000000, -0.9999939076577903929, 0.003490651415223739937 ) ) ;
#123204 = CARTESIAN_POINT ( 'NONE',  ( -11.89999999999999503, 2.500000000000000000, 4.576537180435972019 ) ) ;
#123205 = ORIENTED_EDGE ( 'NONE', *, *, #128917, .T. ) ;
#123206 = VERTEX_POINT ( 'NONE', #77056 ) ;
#123207 = ORIENTED_EDGE ( 'NONE', *, *, #72228, .F. ) ;
#123208 = LINE ( 'NONE', #69745, #111740 ) ;
#123209 = ORIENTED_EDGE ( 'NONE', *, *, #31221, .F. ) ;
#123210 = DIRECTION ( 'NONE',  ( -0.000000000000000000, -1.000000000000000000, -0.000000000000000000 ) ) ;
#123212 = ORIENTED_EDGE ( 'NONE', *, *, #84455, .F. ) ;
#123211 = ORIENTED_EDGE ( 'NONE', *, *, #47704, .T. ) ;
#123213 = ORIENTED_EDGE ( 'NONE', *, *, #124232, .F. ) ;
#123214 = LINE ( 'NONE', #112105, #64736 ) ;
#123215 = CIRCLE ( 'NONE', #89751, 0.1000000000000002554 ) ;
#123216 = CONICAL_SURFACE ( 'NONE', #110587, 0.1000000000000002554, 0.003490658503988666988 ) ;
#123217 = DIRECTION ( 'NONE',  ( 0.000000000000000000, -0.000000000000000000, 1.000000000000000000 ) ) ;
#123218 = CARTESIAN_POINT ( 'NONE',  ( -7.050000000000016698, 2.500000000000000000, -2.165063509461101710 ) ) ;
#123219 = CARTESIAN_POINT ( 'NONE',  ( -6.450000000000019718, 12.50000000000000000, -1.818653347947326138 ) ) ;
#123220 = CARTESIAN_POINT ( 'NONE',  ( 1.649999999999951505, 2.500000000000000000, -2.857883832488653741 ) ) ;
#123221 = ORIENTED_EDGE ( 'NONE', *, *, #124276, .F. ) ;
#123222 = AXIS2_PLACEMENT_3D ( 'NONE', #6667, #116650, #25054 ) ;
#123224 = CARTESIAN_POINT ( 'NONE',  ( -10.40000000000000213, 2.500000000000000000, 4.230127018922196669 ) ) ;
#123223 = CIRCLE ( 'NONE', #127424, 0.06509327318403745899 ) ;
#123225 = ORIENTED_EDGE ( 'NONE', *, *, #36165, .T. ) ;
#123226 = AXIS2_PLACEMENT_3D ( 'NONE', #73293, #113878, #123667 ) ;
#123227 = EDGE_LOOP ( 'NONE', ( #28698, #126253 ) ) ;
#123228 = EDGE_CURVE ( 'NONE', #3365, #82926, #1857, .T. ) ;
#123229 = VERTEX_POINT ( 'NONE', #96046 ) ;
#123230 = DIRECTION ( 'NONE',  ( 0.000000000000000000, 0.000000000000000000, 1.000000000000000000 ) ) ;
#123231 = ORIENTED_EDGE ( 'NONE', *, *, #67265, .T. ) ;
#123232 = ORIENTED_EDGE ( 'NONE', *, *, #14793, .T. ) ;
#123233 = VERTEX_POINT ( 'NONE', #87498 ) ;
#123234 = EDGE_CURVE ( 'NONE', #16723, #127948, #58410, .T. ) ;
#123235 = CIRCLE ( 'NONE', #129517, 0.1000000000000002554 ) ;
#123236 = DIRECTION ( 'NONE',  ( 0.000000000000000000, 1.000000000000000000, 0.000000000000000000 ) ) ;
#123237 = PLANE ( 'NONE',  #45893 ) ;
#123238 = CIRCLE ( 'NONE', #77257, 0.06509327318403745899 ) ;
#123239 = DIRECTION ( 'NONE',  ( 0.000000000000000000, -0.9999939076577903929, 0.003490651415223739937 ) ) ;
#123240 = DIRECTION ( 'NONE',  ( -0.000000000000000000, 1.000000000000000000, -0.000000000000000000 ) ) ;
#123241 = DIRECTION ( 'NONE',  ( 0.000000000000000000, 0.000000000000000000, 1.000000000000000000 ) ) ;
#123242 = LINE ( 'NONE', #35510, #44757 ) ;
#123243 = ORIENTED_EDGE ( 'NONE', *, *, #7436, .T. ) ;
#123244 = CARTESIAN_POINT ( 'NONE',  ( 15.83209681635555022, 2.500000000000000000, -5.404881881984143099 ) ) ;
#123245 = VERTEX_POINT ( 'NONE', #67192 ) ;
#123246 = CARTESIAN_POINT ( 'NONE',  ( 184.7916666666666572, 4.445597072760062218, -7.700000000000102318 ) ) ;
#123247 = AXIS2_PLACEMENT_3D ( 'NONE', #24303, #45237, #53758 ) ;
#123248 = ORIENTED_EDGE ( 'NONE', *, *, #70676, .F. ) ;
#123249 = ORIENTED_EDGE ( 'NONE', *, *, #101847, .F. ) ;
#123250 = DIRECTION ( 'NONE',  ( -4.274815082592931898E-19, -0.9999939076577903929, -0.003490651415223739937 ) ) ;
#123251 = DIRECTION ( 'NONE',  ( -0.000000000000000000, -1.000000000000000000, -0.000000000000000000 ) ) ;
#123252 = DIRECTION ( 'NONE',  ( -0.000000000000000000, 1.000000000000000000, -0.000000000000000000 ) ) ;
#123253 = VERTEX_POINT ( 'NONE', #15538 ) ;
#123254 = ORIENTED_EDGE ( 'NONE', *, *, #108417, .T. ) ;
#123255 = CARTESIAN_POINT ( 'NONE',  ( -15.59999999999998010, 12.50000000000000000, 0.4115034346978133639 ) ) ;
#123256 = CARTESIAN_POINT ( 'NONE',  ( -11.84999999999999787, 12.50000000000000000, -1.753560074763284460 ) ) ;
#123257 = CARTESIAN_POINT ( 'NONE',  ( 12.89999999999990266, 2.500000000000000000, 5.122947341949749323 ) ) ;
#123258 = CARTESIAN_POINT ( 'NONE',  ( 13.09999999999990195, 2.500000000000000000, 4.083716857408420609 ) ) ;
#123259 = DIRECTION ( 'NONE',  ( 0.000000000000000000, -0.9999939076577903929, 0.003490651415223739937 ) ) ;
#123260 = EDGE_CURVE ( 'NONE', #26010, #81531, #33285, .T. ) ;
#123261 = ORIENTED_EDGE ( 'NONE', *, *, #126420, .T. ) ;
#123262 = AXIS2_PLACEMENT_3D ( 'NONE', #59147, #96459, #118691 ) ;
#123263 = VERTEX_POINT ( 'NONE', #35844 ) ;
#123264 = CARTESIAN_POINT ( 'NONE',  ( 6.449999999999931788, 12.50000000000000000, 6.148780366869520009 ) ) ;
#123266 = ADVANCED_FACE ( 'NONE', ( #115679 ), #16177, .T. ) ;
#123265 = DIRECTION ( 'NONE',  ( 0.000000000000000000, -0.000000000000000000, 1.000000000000000000 ) ) ;
#123268 = CIRCLE ( 'NONE', #62737, 0.1000000000000000472 ) ;
#123267 = AXIS2_PLACEMENT_3D ( 'NONE', #82869, #95262, #52742 ) ;
#123269 = CIRCLE ( 'NONE', #33410, 0.06509327318403745899 ) ;
#123270 = ADVANCED_FACE ( 'NONE', ( #6347 ), #75120, .T. ) ;
#123271 = CARTESIAN_POINT ( 'NONE',  ( 186.9583333333333428, 4.445597072760117285, 7.699999999999999289 ) ) ;
#123272 = CARTESIAN_POINT ( 'NONE',  ( 8.749999999999923617, 2.500000000000000000, -7.288010851410854585 ) ) ;
#123273 = CARTESIAN_POINT ( 'NONE',  ( 4.149999999999941735, 12.50000000000000000, -2.857883832488653741 ) ) ;
#123274 = DIRECTION ( 'NONE',  ( -4.274815082592931898E-19, -0.9999939076577903929, -0.003490651415223739937 ) ) ;
#123275 = EDGE_CURVE ( 'NONE', #105827, #16102, #87629, .T. ) ;
#123276 = DIRECTION ( 'NONE',  ( -0.000000000000000000, 1.000000000000000000, -0.000000000000000000 ) ) ;
#123277 = VERTEX_POINT ( 'NONE', #88127 ) ;
#123278 = CIRCLE ( 'NONE', #27137, 0.06509327318403745899 ) ;
#123279 = DIRECTION ( 'NONE',  ( 0.000000000000000000, 0.000000000000000000, -1.000000000000000000 ) ) ;
#123280 = DIRECTION ( 'NONE',  ( -0.000000000000000000, -1.000000000000000000, -0.000000000000000000 ) ) ;
#123281 = DIRECTION ( 'NONE',  ( -0.000000000000000000, 1.000000000000000000, -0.000000000000000000 ) ) ;
#123282 = ADVANCED_FACE ( 'NONE', ( #90077 ), #58070, .T. ) ;
#123283 = EDGE_LOOP ( 'NONE', ( #66157, #22508, #6266, #40591 ) ) ;
#123284 = EDGE_CURVE ( 'NONE', #88991, #74504, #48238, .T. ) ;
#123285 = FACE_OUTER_BOUND ( 'NONE', #22998, .T. ) ;
#123286 = ORIENTED_EDGE ( 'NONE', *, *, #45608, .T. ) ;
#123287 = CARTESIAN_POINT ( 'NONE',  ( 2.699999999999944666, 12.50000000000000000, 4.676537180435972552 ) ) ;
#123288 = ORIENTED_EDGE ( 'NONE', *, *, #125777, .T. ) ;
#123289 = LINE ( 'NONE', #64992, #58499 ) ;
#123290 = FACE_OUTER_BOUND ( 'NONE', #82227, .T. ) ;
#123291 = DIRECTION ( 'NONE',  ( -0.000000000000000000, -1.000000000000000000, -0.000000000000000000 ) ) ;
#123292 = ORIENTED_EDGE ( 'NONE', *, *, #89888, .F. ) ;
#123293 = CIRCLE ( 'NONE', #45946, 0.06509327318403745899 ) ;
#123294 = DIRECTION ( 'NONE',  ( -0.000000000000000000, -1.000000000000000000, -0.000000000000000000 ) ) ;
#123295 = AXIS2_PLACEMENT_3D ( 'NONE', #74473, #33280, #3162 ) ;
#123296 = CARTESIAN_POINT ( 'NONE',  ( 3.549999999999942091, 12.50000000000000000, 2.446380397790835826 ) ) ;
#123297 = EDGE_LOOP ( 'NONE', ( #60545, #22343, #6278, #81444 ) ) ;
#123299 = AXIS2_PLACEMENT_3D ( 'NONE', #12597, #83916, #63657 ) ;
#123298 = AXIS2_PLACEMENT_3D ( 'NONE', #103762, #14705, #63839 ) ;
#123300 = EDGE_LOOP ( 'NONE', ( #102930, #54532 ) ) ;
#123301 = ORIENTED_EDGE ( 'NONE', *, *, #76024, .T. ) ;
#123302 = CARTESIAN_POINT ( 'NONE',  ( 1.249999999999953815, 2.500000000000000000, 1.472243186433545459 ) ) ;
#123303 = DIRECTION ( 'NONE',  ( 0.000000000000000000, -0.9999939076577903929, 0.003490651415223739937 ) ) ;
#123304 = DIRECTION ( 'NONE',  ( -4.274815082592931898E-19, -0.9999939076577903929, -0.003490651415223739937 ) ) ;
#123305 = VERTEX_POINT ( 'NONE', #19405 ) ;
#123306 = CIRCLE ( 'NONE', #66868, 0.06509327318403745899 ) ;
#123307 = DIRECTION ( 'NONE',  ( 0.000000000000000000, 0.000000000000000000, 1.000000000000000000 ) ) ;
#123308 = CARTESIAN_POINT ( 'NONE',  ( -7.500000000000015099, 2.500000000000000000, -5.022947341949754119 ) ) ;
#123309 = EDGE_LOOP ( 'NONE', ( #104623, #79545 ) ) ;
#123311 = CARTESIAN_POINT ( 'NONE',  ( -3.550000000000027356, 2.500000000000000000, -2.511473670974877948 ) ) ;
#123310 = AXIS2_PLACEMENT_3D ( 'NONE', #36830, #96361, #115350 ) ;
#123312 = CARTESIAN_POINT ( 'NONE',  ( 9.149999999999918643, 2.500000000000000000, -6.495190528383302464 ) ) ;
#123313 = AXIS2_PLACEMENT_3D ( 'NONE', #33481, #125690, #25559 ) ;
#123315 = ADVANCED_FACE ( 'NONE', ( #97975 ), #50014, .T. ) ;
#123314 = DIRECTION ( 'NONE',  ( 0.000000000000000000, 1.000000000000000000, 0.000000000000000000 ) ) ;
#123316 = PLANE ( 'NONE',  #28353 ) ;
#123317 = CARTESIAN_POINT ( 'NONE',  ( -0.8500000000000382805, 12.50000000000000000, -5.802370205355749988 ) ) ;
#123318 = EDGE_CURVE ( 'NONE', #53598, #82164, #31220, .T. ) ;
#123319 = AXIS2_PLACEMENT_3D ( 'NONE', #127067, #68121, #108053 ) ;
#123320 = DIRECTION ( 'NONE',  ( 0.000000000000000000, 1.000000000000000000, 0.000000000000000000 ) ) ;
#123321 = CARTESIAN_POINT ( 'NONE',  ( 2.299999999999947864, 12.50000000000000000, 3.983716857408420964 ) ) ;
#123322 = EDGE_CURVE ( 'NONE', #62381, #17095, #68512, .T. ) ;
#123324 = EDGE_CURVE ( 'NONE', #98051, #113165, #102320, .T. ) ;
#123323 = AXIS2_PLACEMENT_3D ( 'NONE', #5271, #57617, #105423 ) ;
#123325 = EDGE_LOOP ( 'NONE', ( #125031, #19448, #17166, #54297 ) ) ;
#123326 = ORIENTED_EDGE ( 'NONE', *, *, #113985, .T. ) ;
#123328 = VERTEX_POINT ( 'NONE', #39735 ) ;
#123327 = EDGE_CURVE ( 'NONE', #117845, #100514, #108435, .T. ) ;
#123329 = ORIENTED_EDGE ( 'NONE', *, *, #66979, .F. ) ;
#123330 = AXIS2_PLACEMENT_3D ( 'NONE', #98831, #9174, #49116 ) ;
#123331 = LINE ( 'NONE', #33664, #16048 ) ;
#123332 = DIRECTION ( 'NONE',  ( -0.000000000000000000, 1.000000000000000000, -0.000000000000000000 ) ) ;
#123333 = LINE ( 'NONE', #100467, #82306 ) ;
#123334 = VERTEX_POINT ( 'NONE', #118908 ) ;
#123335 = FACE_BOUND ( 'NONE', #105941, .T. ) ;
#123336 = DIRECTION ( 'NONE',  ( 0.000000000000000000, -0.000000000000000000, 1.000000000000000000 ) ) ;
#123337 = DIRECTION ( 'NONE',  ( 0.000000000000000000, 0.000000000000000000, -1.000000000000000000 ) ) ;
#123338 = ADVANCED_FACE ( 'NONE', ( #20074 ), #9600, .T. ) ;
#123339 = FACE_OUTER_BOUND ( 'NONE', #78518, .T. ) ;
#123340 = EDGE_CURVE ( 'NONE', #54140, #87803, #117590, .T. ) ;
#123341 = DIRECTION ( 'NONE',  ( -4.274815082592931898E-19, -0.9999939076577903929, -0.003490651415223739937 ) ) ;
#123342 = DIRECTION ( 'NONE',  ( -0.000000000000000000, 1.000000000000000000, -0.000000000000000000 ) ) ;
#123343 = FACE_OUTER_BOUND ( 'NONE', #40284, .T. ) ;
#123344 = DIRECTION ( 'NONE',  ( 0.000000000000000000, 0.000000000000000000, -1.000000000000000000 ) ) ;
#123345 = CARTESIAN_POINT ( 'NONE',  ( -4.250072516143177381E-14, 12.50000000000000000, -3.572213422710612374 ) ) ;
#123346 = LINE ( 'NONE', #14015, #33033 ) ;
#123347 = CARTESIAN_POINT ( 'NONE',  ( 4.549999999999939426, 2.500000000000000000, -2.065063509461102065 ) ) ;
#123348 = ORIENTED_EDGE ( 'NONE', *, *, #66837, .T. ) ;
#123349 = EDGE_LOOP ( 'NONE', ( #68739, #127047 ) ) ;
#123350 = ORIENTED_EDGE ( 'NONE', *, *, #108524, .T. ) ;
#123351 = ORIENTED_EDGE ( 'NONE', *, *, #81346, .T. ) ;
#123352 = ORIENTED_EDGE ( 'NONE', *, *, #45304, .T. ) ;
#123353 = EDGE_LOOP ( 'NONE', ( #114822, #90166 ) ) ;
#123354 = DIRECTION ( 'NONE',  ( -0.000000000000000000, 1.000000000000000000, -0.000000000000000000 ) ) ;
#123355 = CONICAL_SURFACE ( 'NONE', #98206, 0.09999999999999982514, 0.003490658503988666988 ) ;
#123356 = VERTEX_POINT ( 'NONE', #89450 ) ;
#123357 = VERTEX_POINT ( 'NONE', #129408 ) ;
#123359 = AXIS2_PLACEMENT_3D ( 'NONE', #50088, #99816, #81464 ) ;
#123358 = CONICAL_SURFACE ( 'NONE', #10473, 0.1000000000000002554, 0.003490658503988666988 ) ;
#123360 = CARTESIAN_POINT ( 'NONE',  ( 15.62882261213625235, -2.499999999999999556, 5.624357572923363691 ) ) ;
#123361 = DIRECTION ( 'NONE',  ( -0.000000000000000000, 1.000000000000000000, -0.000000000000000000 ) ) ;
#123362 = CARTESIAN_POINT ( 'NONE',  ( 9.799999999999917222, 2.500000000000000000, 0.3464101615137735735 ) ) ;
#123363 = VERTEX_POINT ( 'NONE', #39087 ) ;
#123364 = LINE ( 'NONE', #36776, #81945 ) ;
#123365 = AXIS2_PLACEMENT_3D ( 'NONE', #76731, #66255, #116647 ) ;
#123366 = ORIENTED_EDGE ( 'NONE', *, *, #124509, .F. ) ;
#123367 = ORIENTED_EDGE ( 'NONE', *, *, #53575, .F. ) ;
#123368 = DIRECTION ( 'NONE',  ( -0.000000000000000000, -1.000000000000000000, -0.000000000000000000 ) ) ;
#123369 = DIRECTION ( 'NONE',  ( 0.000000000000000000, 0.000000000000000000, 1.000000000000000000 ) ) ;
#123370 = ORIENTED_EDGE ( 'NONE', *, *, #6445, .F. ) ;
#123371 = ORIENTED_EDGE ( 'NONE', *, *, #76044, .T. ) ;
#123372 = CARTESIAN_POINT ( 'NONE',  ( -10.00000000000000533, 12.50000000000000000, -5.022947341949749678 ) ) ;
#123373 = ADVANCED_FACE ( 'NONE', ( #79008 ), #52140, .T. ) ;
#123374 = CARTESIAN_POINT ( 'NONE',  ( -1.250000000000035749, 12.50000000000000000, -2.857883832488653741 ) ) ;
#123375 = PLANE ( 'NONE',  #74958 ) ;
#123376 = DIRECTION ( 'NONE',  ( 0.000000000000000000, 0.000000000000000000, 1.000000000000000000 ) ) ;
#123377 = CARTESIAN_POINT ( 'NONE',  ( 1.658312395177699017, -2.500000000000000444, 6.000000000000005329 ) ) ;
#123378 = VERTEX_POINT ( 'NONE', #18121 ) ;
#123379 = CARTESIAN_POINT ( 'NONE',  ( 2.500000000000002220, -2.500000000000000000, 9.000000000000001776 ) ) ;
#123380 = CIRCLE ( 'NONE', #66929, 0.06509327318403743123 ) ;
#123381 = CIRCLE ( 'NONE', #6287, 0.06509327318403745899 ) ;
#123382 = ORIENTED_EDGE ( 'NONE', *, *, #51328, .T. ) ;
#123383 = CARTESIAN_POINT ( 'NONE',  ( 11.84999999999990727, 2.500000000000000000, 6.048780366869520364 ) ) ;
#123384 = ORIENTED_EDGE ( 'NONE', *, *, #73588, .F. ) ;
#123385 = CARTESIAN_POINT ( 'NONE',  ( 8.349999999999919709, 2.500000000000000000, 5.802370205355744659 ) ) ;
#123386 = DIRECTION ( 'NONE',  ( -4.274815082592931898E-19, -0.9999939076577903929, -0.003490651415223739937 ) ) ;
#123387 = DIRECTION ( 'NONE',  ( -1.000000000000000000, 0.000000000000000000, 0.000000000000000000 ) ) ;
#123388 = DIRECTION ( 'NONE',  ( 0.000000000000000000, 0.000000000000000000, 1.000000000000000000 ) ) ;
#123389 = VERTEX_POINT ( 'NONE', #69815 ) ;
#123390 = CONICAL_SURFACE ( 'NONE', #33528, 0.09999999999999982514, 0.003490658503988666988 ) ;
#123391 = DIRECTION ( 'NONE',  ( -4.274815082592931898E-19, -0.9999939076577903929, -0.003490651415223739937 ) ) ;
#123392 = EDGE_LOOP ( 'NONE', ( #122646, #54157, #37811, #117233 ) ) ;
#123393 = ORIENTED_EDGE ( 'NONE', *, *, #10807, .T. ) ;
#123394 = EDGE_LOOP ( 'NONE', ( #19975, #24485, #26428, #39629 ) ) ;
#123395 = CARTESIAN_POINT ( 'NONE',  ( 17.50000000000000000, 2.749999999999999556, 10.00000000000000178 ) ) ;
#123396 = DIRECTION ( 'NONE',  ( 0.000000000000000000, 1.000000000000000000, 0.000000000000000000 ) ) ;
#123397 = CARTESIAN_POINT ( 'NONE',  ( 185.6510416670080303, 4.367472073101518859, -7.564683531249999149 ) ) ;
#123398 = DIRECTION ( 'NONE',  ( 0.000000000000000000, 0.000000000000000000, 1.000000000000000000 ) ) ;
#123399 = AXIS2_PLACEMENT_3D ( 'NONE', #13785, #123112, #102188 ) ;
#123400 = AXIS2_PLACEMENT_3D ( 'NONE', #64691, #45072, #45711 ) ;
#123401 = DIRECTION ( 'NONE',  ( -0.000000000000000000, -1.000000000000000000, -0.000000000000000000 ) ) ;
#123402 = CARTESIAN_POINT ( 'NONE',  ( -1.900000000000034550, 12.50000000000000000, 4.676537180435972552 ) ) ;
#123403 = EDGE_CURVE ( 'NONE', #28777, #128265, #114818, .T. ) ;
#123404 = AXIS2_PLACEMENT_3D ( 'NONE', #39917, #60835, #59576 ) ;
#123405 = ORIENTED_EDGE ( 'NONE', *, *, #10814, .T. ) ;
#123406 = FACE_OUTER_BOUND ( 'NONE', #34022, .T. ) ;
#123407 = ADVANCED_FACE ( 'NONE', ( #50192 ), #116867, .T. ) ;
#123408 = ORIENTED_EDGE ( 'NONE', *, *, #69497, .F. ) ;
#123409 = AXIS2_PLACEMENT_3D ( 'NONE', #126705, #65831, #126039 ) ;
#123410 = DIRECTION ( 'NONE',  ( 0.000000000000000000, 0.000000000000000000, 1.000000000000000000 ) ) ;
#123411 = EDGE_CURVE ( 'NONE', #98982, #86533, #37569, .T. ) ;
#123412 = DIRECTION ( 'NONE',  ( 0.000000000000000000, -0.000000000000000000, 1.000000000000000000 ) ) ;
#123413 = DIRECTION ( 'NONE',  ( -0.000000000000000000, 1.000000000000000000, -0.000000000000000000 ) ) ;
#123414 = DIRECTION ( 'NONE',  ( 0.000000000000000000, -0.9999939076577903929, 0.003490651415223739937 ) ) ;
#123415 = EDGE_CURVE ( 'NONE', #46680, #102274, #77180, .T. ) ;
#123416 = VERTEX_POINT ( 'NONE', #104988 ) ;
#123417 = DIRECTION ( 'NONE',  ( 0.000000000000000000, 0.000000000000000000, 1.000000000000000000 ) ) ;
#123419 = ORIENTED_EDGE ( 'NONE', *, *, #106183, .T. ) ;
#123418 = DIRECTION ( 'NONE',  ( 0.000000000000000000, 0.000000000000000000, -1.000000000000000000 ) ) ;
#123420 = EDGE_CURVE ( 'NONE', #108043, #43147, #79340, .T. ) ;
#123421 = EDGE_CURVE ( 'NONE', #6735, #76595, #127863, .T. ) ;
#123422 = EDGE_CURVE ( 'NONE', #86459, #40320, #129436, .T. ) ;
#123423 = ADVANCED_FACE ( 'NONE', ( #96455 ), #24943, .T. ) ;
#123424 = EDGE_CURVE ( 'NONE', #86712, #67418, #72977, .T. ) ;
#123425 = ORIENTED_EDGE ( 'NONE', *, *, #110161, .F. ) ;
#123426 = CARTESIAN_POINT ( 'NONE',  ( 10.19999999999991225, 12.50000000000000000, -4.741630453620016006 ) ) ;
#123427 = EDGE_LOOP ( 'NONE', ( #108342, #107173, #48846, #73889 ) ) ;
#123428 = EDGE_LOOP ( 'NONE', ( #41258, #74305 ) ) ;
#123429 = CARTESIAN_POINT ( 'NONE',  ( 97.50000000000000000, 0.000000000000000000, 0.000000000000000000 ) ) ;
#123430 = AXIS2_PLACEMENT_3D ( 'NONE', #71064, #110964, #12126 ) ;
#123431 = AXIS2_PLACEMENT_3D ( 'NONE', #111789, #60752, #51587 ) ;
#123432 = ADVANCED_FACE ( 'NONE', ( #15314 ), #7438, .T. ) ;
#123433 = ORIENTED_EDGE ( 'NONE', *, *, #113546, .T. ) ;
#123434 = CARTESIAN_POINT ( 'NONE',  ( 16.84158739990415654, 0.4722467112503249131, -5.802037699230074175 ) ) ;
#123435 = CARTESIAN_POINT ( 'NONE',  ( 1.049999999999953637, 12.50000000000000000, -1.818653347947326138 ) ) ;
#123436 = DIRECTION ( 'NONE',  ( 0.000000000000000000, 0.000000000000000000, 1.000000000000000000 ) ) ;
#123437 = ORIENTED_EDGE ( 'NONE', *, *, #117831, .F. ) ;
#123438 = AXIS2_PLACEMENT_3D ( 'NONE', #94441, #95106, #4762 ) ;
#123439 = DIRECTION ( 'NONE',  ( 0.000000000000000000, -0.9999939076577903929, 0.003490651415223739937 ) ) ;
#123441 = VERTEX_POINT ( 'NONE', #118040 ) ;
#123440 = DIRECTION ( 'NONE',  ( 0.000000000000000000, 1.000000000000000000, 0.000000000000000000 ) ) ;
#123442 = LINE ( 'NONE', #114905, #50688 ) ;
#123443 = DIRECTION ( 'NONE',  ( 0.000000000000000000, -0.9999939076577903929, 0.003490651415223739937 ) ) ;
#123444 = VERTEX_POINT ( 'NONE', #76198 ) ;
#123445 = ORIENTED_EDGE ( 'NONE', *, *, #122447, .T. ) ;
#123446 = EDGE_LOOP ( 'NONE', ( #36950, #83543 ) ) ;
#123447 = VERTEX_POINT ( 'NONE', #6146 ) ;
#123448 = CARTESIAN_POINT ( 'NONE',  ( 11.04999999999990656, 2.500000000000000000, -6.148780366869526226 ) ) ;
#123449 = DIRECTION ( 'NONE',  ( 0.000000000000000000, 0.000000000000000000, 1.000000000000000000 ) ) ;
#123450 = CARTESIAN_POINT ( 'NONE',  ( 3.949999999999940670, 2.500000000000000000, 1.818653347947321475 ) ) ;
#123451 = FACE_BOUND ( 'NONE', #26955, .T. ) ;
#123452 = EDGE_LOOP ( 'NONE', ( #117505, #66781, #48542, #125368 ) ) ;
#123453 = CARTESIAN_POINT ( 'NONE',  ( 187.3593750003414016, 0.000000000000000000, 7.564683531250000925 ) ) ;
#123454 = CARTESIAN_POINT ( 'NONE',  ( 6.899999999999928413, 12.50000000000000000, 3.983716857408420964 ) ) ;
#123455 = DIRECTION ( 'NONE',  ( 0.000000000000000000, 0.000000000000000000, -1.000000000000000000 ) ) ;
#123456 = DIRECTION ( 'NONE',  ( 0.000000000000000000, 0.000000000000000000, 1.000000000000000000 ) ) ;
#123457 = CARTESIAN_POINT ( 'NONE',  ( 2.499999999999947153, 12.50000000000000000, 0.6277270498435120194 ) ) ;
#123458 = EDGE_CURVE ( 'NONE', #56145, #128265, #95190, .T. ) ;
#123459 = DIRECTION ( 'NONE',  ( -4.274815082592931898E-19, -0.9999939076577903929, -0.003490651415223739937 ) ) ;
#123460 = EDGE_CURVE ( 'NONE', #76430, #40877, #16513, .T. ) ;
#123461 = VECTOR ( 'NONE', #57737, 1000.000000000000000 ) ;
#123462 = CIRCLE ( 'NONE', #50324, 0.1000000000000002554 ) ;
#123463 = DIRECTION ( 'NONE',  ( -0.000000000000000000, -1.000000000000000000, -0.000000000000000000 ) ) ;
#123464 = EDGE_CURVE ( 'NONE', #72667, #66994, #35416, .T. ) ;
#123465 = ORIENTED_EDGE ( 'NONE', *, *, #97307, .T. ) ;
#123466 = ORIENTED_EDGE ( 'NONE', *, *, #86781, .F. ) ;
#123467 = EDGE_LOOP ( 'NONE', ( #59800, #11952, #4847, #108707 ) ) ;
#123468 = ORIENTED_EDGE ( 'NONE', *, *, #90089, .T. ) ;
#123469 = ORIENTED_EDGE ( 'NONE', *, *, #93707, .T. ) ;
#123470 = DIRECTION ( 'NONE',  ( -0.000000000000000000, 1.000000000000000000, -0.000000000000000000 ) ) ;
#123471 = DIRECTION ( 'NONE',  ( 0.000000000000000000, -0.000000000000000000, 1.000000000000000000 ) ) ;
#123473 = ADVANCED_FACE ( 'NONE', ( #125919 ), #66703, .T. ) ;
#123472 = ORIENTED_EDGE ( 'NONE', *, *, #30656, .T. ) ;
#123474 = FACE_BOUND ( 'NONE', #17904, .T. ) ;
#123475 = CIRCLE ( 'NONE', #104691, 0.06509327318403745899 ) ;
#123476 = CARTESIAN_POINT ( 'NONE',  ( -6.850000000000013856, 2.500000000000000000, 6.741600689897071952 ) ) ;
#123477 = EDGE_CURVE ( 'NONE', #95827, #126422, #66362, .T. ) ;
#123478 = EDGE_CURVE ( 'NONE', #53570, #61169, #89692, .T. ) ;
#123479 = ADVANCED_FACE ( 'NONE', ( #97762 ), #83455, .T. ) ;
#123480 = EDGE_LOOP ( 'NONE', ( #74790, #93304, #43959, #30461 ) ) ;
#123481 = DIRECTION ( 'NONE',  ( 0.000000000000000000, 0.000000000000000000, 1.000000000000000000 ) ) ;
#123482 = CARTESIAN_POINT ( 'NONE',  ( 4.599999999999935696, 2.500000000000000000, 5.122947341949749323 ) ) ;
#123483 = DIRECTION ( 'NONE',  ( -4.274815082592931898E-19, -0.9999939076577903929, -0.003490651415223739937 ) ) ;
#123484 = ORIENTED_EDGE ( 'NONE', *, *, #827, .F. ) ;
#123485 = DIRECTION ( 'NONE',  ( 1.000000000000000000, -0.000000000000000000, -0.000000000000000000 ) ) ;
#123486 = EDGE_CURVE ( 'NONE', #39021, #15192, #36922, .T. ) ;
#123487 = CIRCLE ( 'NONE', #67040, 0.06509327318403745899 ) ;
#123488 = VERTEX_POINT ( 'NONE', #78135 ) ;
#123489 = CONICAL_SURFACE ( 'NONE', #29510, 0.09999999999999982514, 0.003490658503988666988 ) ;
#123490 = EDGE_LOOP ( 'NONE', ( #74127, #111745 ) ) ;
#123491 = ORIENTED_EDGE ( 'NONE', *, *, #90622, .F. ) ;
#123492 = DIRECTION ( 'NONE',  ( -0.000000000000000000, -1.000000000000000000, -0.000000000000000000 ) ) ;
#123493 = DIRECTION ( 'NONE',  ( 0.000000000000000000, 0.000000000000000000, 1.000000000000000000 ) ) ;
#123494 = DIRECTION ( 'NONE',  ( 0.000000000000000000, 1.000000000000000000, 0.000000000000000000 ) ) ;
#123495 = EDGE_LOOP ( 'NONE', ( #29439, #57288, #62312, #99592 ) ) ;
#123496 = CARTESIAN_POINT ( 'NONE',  ( 10.39999999999991509, 2.500000000000000000, 0.7928203230275495672 ) ) ;
#123497 = AXIS2_PLACEMENT_3D ( 'NONE', #17515, #99963, #60058 ) ;
#123498 = DIRECTION ( 'NONE',  ( -0.000000000000000000, -1.000000000000000000, -0.000000000000000000 ) ) ;
#123499 = CARTESIAN_POINT ( 'NONE',  ( -10.85000000000000142, 12.50000000000000000, -6.560283801567336148 ) ) ;
#123500 = VECTOR ( 'NONE', #109643, 1000.000000000000000 ) ;
#123501 = CARTESIAN_POINT ( 'NONE',  ( 186.5729166673494603, 4.445597072760120838, -7.699999999999998401 ) ) ;
#123502 = ORIENTED_EDGE ( 'NONE', *, *, #9948, .F. ) ;
#123503 = LINE ( 'NONE', #64590, #87134 ) ;
#123504 = EDGE_CURVE ( 'NONE', #27665, #106728, #121086, .T. ) ;
#123505 = ORIENTED_EDGE ( 'NONE', *, *, #21427, .F. ) ;
#123506 = DIRECTION ( 'NONE',  ( 0.000000000000000000, -0.000000000000000000, 1.000000000000000000 ) ) ;
#123507 = ORIENTED_EDGE ( 'NONE', *, *, #18548, .T. ) ;
#123508 = EDGE_LOOP ( 'NONE', ( #100606, #24469 ) ) ;
#123509 = CARTESIAN_POINT ( 'NONE',  ( 8.549999999999922551, 12.50000000000000000, -6.148780366869526226 ) ) ;
#123510 = DIRECTION ( 'NONE',  ( 0.000000000000000000, 0.000000000000000000, -1.000000000000000000 ) ) ;
#123511 = DIRECTION ( 'NONE',  ( -0.000000000000000000, -1.000000000000000000, -0.000000000000000000 ) ) ;
#123512 = FACE_OUTER_BOUND ( 'NONE', #125711, .T. ) ;
#123513 = CARTESIAN_POINT ( 'NONE',  ( -14.54999999999998472, 2.500000000000000000, 2.265063509461101354 ) ) ;
#123514 = ORIENTED_EDGE ( 'NONE', *, *, #121583, .T. ) ;
#123515 = ORIENTED_EDGE ( 'NONE', *, *, #119492, .F. ) ;
#123516 = FACE_OUTER_BOUND ( 'NONE', #6326, .T. ) ;
#123517 = EDGE_CURVE ( 'NONE', #907, #63096, #37482, .T. ) ;
#123518 = FACE_BOUND ( 'NONE', #80157, .T. ) ;
#123520 = DIRECTION ( 'NONE',  ( -0.000000000000000000, -1.000000000000000000, -0.000000000000000000 ) ) ;
#123519 = CIRCLE ( 'NONE', #75405, 0.09999999999999999167 ) ;
#123521 = ORIENTED_EDGE ( 'NONE', *, *, #83085, .T. ) ;
#123522 = ORIENTED_EDGE ( 'NONE', *, *, #30963, .F. ) ;
#123523 = AXIS2_PLACEMENT_3D ( 'NONE', #74791, #114696, #55789 ) ;
#123524 = VECTOR ( 'NONE', #61246, 1000.000000000000000 ) ;
#123525 = DIRECTION ( 'NONE',  ( 0.000000000000000000, 1.000000000000000000, 0.000000000000000000 ) ) ;
#123526 = ORIENTED_EDGE ( 'NONE', *, *, #91780, .F. ) ;
#123527 = DIRECTION ( 'NONE',  ( 0.000000000000000000, 1.000000000000000000, 0.000000000000000000 ) ) ;
#123528 = CIRCLE ( 'NONE', #31512, 0.09999999999999982514 ) ;
#123529 = CARTESIAN_POINT ( 'NONE',  ( 187.5000000000000000, 0.000000000000000000, 0.000000000000000000 ) ) ;
#123530 = VERTEX_POINT ( 'NONE', #129192 ) ;
#123531 = DIRECTION ( 'NONE',  ( 0.000000000000000000, 0.000000000000000000, 1.000000000000000000 ) ) ;
#123532 = DIRECTION ( 'NONE',  ( 0.000000000000000000, 0.000000000000000000, -1.000000000000000000 ) ) ;
#123533 = DIRECTION ( 'NONE',  ( 0.000000000000000000, 1.000000000000000000, 0.000000000000000000 ) ) ;
#123534 = CIRCLE ( 'NONE', #58704, 0.1000000000000002554 ) ;
#123535 = EDGE_CURVE ( 'NONE', #19955, #68062, #110167, .T. ) ;
#123536 = DIRECTION ( 'NONE',  ( 0.000000000000000000, 0.000000000000000000, 1.000000000000000000 ) ) ;
#123537 = EDGE_LOOP ( 'NONE', ( #3227, #47578 ) ) ;
#123538 = DIRECTION ( 'NONE',  ( 0.000000000000000000, 0.000000000000000000, -1.000000000000000000 ) ) ;
#123539 = CARTESIAN_POINT ( 'NONE',  ( 21.15177371151419550, -2.593223176056363766, 4.151029080743462885 ) ) ;
#123540 = EDGE_LOOP ( 'NONE', ( #16820, #94731, #1101, #26837 ) ) ;
#123541 = ORIENTED_EDGE ( 'NONE', *, *, #88568, .F. ) ;
#123542 = CARTESIAN_POINT ( 'NONE',  ( 186.7552083336747444, 6.551208109652275624, -3.782341765624998686 ) ) ;
#123543 = CARTESIAN_POINT ( 'NONE',  ( -4.600000000000028955, 2.500000000000000000, -4.330127018922201643 ) ) ;
#123544 = DIRECTION ( 'NONE',  ( -0.000000000000000000, 1.000000000000000000, -0.000000000000000000 ) ) ;
#123545 = CARTESIAN_POINT ( 'NONE',  ( -3.750000000000026201, 2.500000000000000000, 5.702370205355745014 ) ) ;
#123546 = LINE ( 'NONE', #71901, #100825 ) ;
#123547 = LINE ( 'NONE', #14238, #88943 ) ;
#123548 = CARTESIAN_POINT ( 'NONE',  ( 14.59999999999989484, 12.50000000000000000, 0.6277270498435120194 ) ) ;
#123549 = CARTESIAN_POINT ( 'NONE',  ( -4.293440603042597559E-14, 12.50000000000000000, 5.088040615133786027 ) ) ;
#123550 = DIRECTION ( 'NONE',  ( 0.000000000000000000, -0.9999939076577903929, 0.003490651415223739937 ) ) ;
#123551 = DIRECTION ( 'NONE',  ( -0.000000000000000000, -1.000000000000000000, -0.000000000000000000 ) ) ;
#123552 = CARTESIAN_POINT ( 'NONE',  ( 3.349999999999941025, 2.500000000000000000, 7.288010851410849256 ) ) ;
#123553 = AXIS2_PLACEMENT_3D ( 'NONE', #66091, #16957, #67353 ) ;
#123554 = ORIENTED_EDGE ( 'NONE', *, *, #104392, .T. ) ;
#123556 = VERTEX_POINT ( 'NONE', #50588 ) ;
#123555 = AXIS2_PLACEMENT_3D ( 'NONE', #69124, #9575, #20686 ) ;
#123557 = EDGE_CURVE ( 'NONE', #16283, #99145, #31084, .T. ) ;
#123558 = ORIENTED_EDGE ( 'NONE', *, *, #96445, .T. ) ;
#123559 = ORIENTED_EDGE ( 'NONE', *, *, #18288, .T. ) ;
#123560 = DIRECTION ( 'NONE',  ( 0.000000000000000000, -0.000000000000000000, 1.000000000000000000 ) ) ;
#123561 = DIRECTION ( 'NONE',  ( 0.000000000000000000, 0.000000000000000000, 1.000000000000000000 ) ) ;
#123562 = VECTOR ( 'NONE', #103815, 1000.000000000000000 ) ;
#123563 = EDGE_CURVE ( 'NONE', #95146, #61052, #22989, .T. ) ;
#123564 = CIRCLE ( 'NONE', #77596, 0.1000000000000002554 ) ;
#123565 = ORIENTED_EDGE ( 'NONE', *, *, #46765, .T. ) ;
#123566 = DIRECTION ( 'NONE',  ( 0.000000000000000000, 0.000000000000000000, -1.000000000000000000 ) ) ;
#123567 = CARTESIAN_POINT ( 'NONE',  ( -6.700000000000016165, 2.500000000000000000, 4.430127018922196847 ) ) ;
#123569 = VERTEX_POINT ( 'NONE', #11315 ) ;
#123568 = DIRECTION ( 'NONE',  ( 0.000000000000000000, 0.000000000000000000, 1.000000000000000000 ) ) ;
#123570 = EDGE_CURVE ( 'NONE', #73695, #97932, #6229, .T. ) ;
#123571 = ADVANCED_FACE ( 'NONE', ( #19857 ), #58507, .T. ) ;
#123572 = EDGE_CURVE ( 'NONE', #20221, #72457, #10640, .T. ) ;
#123573 = FACE_OUTER_BOUND ( 'NONE', #14555, .T. ) ;
#123574 = EDGE_CURVE ( 'NONE', #51919, #54631, #108652, .T. ) ;
#123575 = DIRECTION ( 'NONE',  ( 0.000000000000000000, -0.000000000000000000, 1.000000000000000000 ) ) ;
#123576 = CONICAL_SURFACE ( 'NONE', #86002, 0.1000000000000000056, 0.003490658503988666988 ) ;
#123577 = EDGE_LOOP ( 'NONE', ( #28291, #94575 ) ) ;
#123578 = CONICAL_SURFACE ( 'NONE', #67120, 0.1000000000000000056, 0.003490658503988666988 ) ;
#123579 = ORIENTED_EDGE ( 'NONE', *, *, #16743, .T. ) ;
#123580 = ORIENTED_EDGE ( 'NONE', *, *, #44518, .T. ) ;
#123581 = ORIENTED_EDGE ( 'NONE', *, *, #50040, .T. ) ;
#123582 = LINE ( 'NONE', #63391, #67742 ) ;
#123583 = EDGE_CURVE ( 'NONE', #81003, #27779, #121177, .T. ) ;
#123584 = AXIS2_PLACEMENT_3D ( 'NONE', #41063, #33790, #52783 ) ;
#123585 = DIRECTION ( 'NONE',  ( 0.000000000000000000, 1.000000000000000000, 0.000000000000000000 ) ) ;
#123586 = CARTESIAN_POINT ( 'NONE',  ( 2.500000000000002220, -1.761799387799150018, -9.999999999999998224 ) ) ;
#123587 = ADVANCED_FACE ( 'NONE', ( #29041 ), #91938, .T. ) ;
#123588 = CARTESIAN_POINT ( 'NONE',  ( 184.5000000000000000, 0.000000000000000000, 0.000000000000000000 ) ) ;
#123590 = VERTEX_POINT ( 'NONE', #80716 ) ;
#123589 = EDGE_CURVE ( 'NONE', #33696, #7764, #35517, .T. ) ;
#123591 = AXIS2_PLACEMENT_3D ( 'NONE', #116711, #88543, #37532 ) ;
#123592 = CIRCLE ( 'NONE', #6490, 0.09999999999999982514 ) ;
#123593 = CARTESIAN_POINT ( 'NONE',  ( 8.549999999999920774, 12.50000000000000000, -2.511473670974877948 ) ) ;
#123594 = ORIENTED_EDGE ( 'NONE', *, *, #29629, .F. ) ;
#123595 = LINE ( 'NONE', #33314, #122768 ) ;
#123596 = DIRECTION ( 'NONE',  ( 0.000000000000000000, 0.000000000000000000, 1.000000000000000000 ) ) ;
#123597 = CARTESIAN_POINT ( 'NONE',  ( -14.79999999999998295, 2.500000000000000000, -0.3464101615137760715 ) ) ;
#123598 = ORIENTED_EDGE ( 'NONE', *, *, #109566, .F. ) ;
#123599 = ORIENTED_EDGE ( 'NONE', *, *, #121424, .T. ) ;
#123600 = ORIENTED_EDGE ( 'NONE', *, *, #116734, .F. ) ;
#123601 = DIRECTION ( 'NONE',  ( -0.000000000000000000, 1.000000000000000000, -0.000000000000000000 ) ) ;
#123602 = CARTESIAN_POINT ( 'NONE',  ( 12.89999999999989910, 2.500000000000000000, 0.6928203230275494784 ) ) ;
#123603 = DIRECTION ( 'NONE',  ( 0.000000000000000000, 0.000000000000000000, 1.000000000000000000 ) ) ;
#123604 = FACE_BOUND ( 'NONE', #3926, .T. ) ;
#123605 = CARTESIAN_POINT ( 'NONE',  ( -8.749999999999975131, 2.500000000000000000, 2.165063509461097713 ) ) ;
#123606 = PLANE ( 'NONE',  #44444 ) ;
#123607 = DIRECTION ( 'NONE',  ( 0.000000000000000000, 0.000000000000000000, 1.000000000000000000 ) ) ;
#123608 = CONICAL_SURFACE ( 'NONE', #102683, 0.09999999999999982514, 0.003490658503988666988 ) ;
#123609 = CIRCLE ( 'NONE', #96416, 0.06509327318403743123 ) ;
#123611 = VECTOR ( 'NONE', #32942, 1000.000000000000000 ) ;
#123610 = DIRECTION ( 'NONE',  ( 0.000000000000000000, 0.000000000000000000, 1.000000000000000000 ) ) ;
#123612 = CARTESIAN_POINT ( 'NONE',  ( 12.09999999999990550, 12.50000000000000000, 5.088040615133786027 ) ) ;
#123613 = CARTESIAN_POINT ( 'NONE',  ( 0.6499999999999543920, 2.500000000000000000, 6.841600689897072485 ) ) ;
#123614 = EDGE_LOOP ( 'NONE', ( #122282, #117305 ) ) ;
#123615 = CONICAL_SURFACE ( 'NONE', #42077, 0.1000000000000002554, 0.003490658503988666988 ) ;
#123616 = DIRECTION ( 'NONE',  ( -0.000000000000000000, -1.000000000000000000, -0.000000000000000000 ) ) ;
#123617 = ORIENTED_EDGE ( 'NONE', *, *, #12576, .T. ) ;
#123618 = ORIENTED_EDGE ( 'NONE', *, *, #102751, .F. ) ;
#123619 = EDGE_LOOP ( 'NONE', ( #86318, #80906, #108739, #19288 ) ) ;
#123620 = VERTEX_POINT ( 'NONE', #109522 ) ;
#123621 = AXIS2_PLACEMENT_3D ( 'NONE', #5510, #46103, #93918 ) ;
#123622 = DIRECTION ( 'NONE',  ( 0.000000000000000000, -0.9999939076577903929, 0.003490651415223739937 ) ) ;
#123623 = EDGE_CURVE ( 'NONE', #98683, #18231, #70244, .T. ) ;
#123624 = FACE_BOUND ( 'NONE', #25097, .T. ) ;
#123625 = DIRECTION ( 'NONE',  ( 0.000000000000000000, 0.000000000000000000, -1.000000000000000000 ) ) ;
#123626 = EDGE_CURVE ( 'NONE', #98794, #88843, #100351, .T. ) ;
#123627 = ADVANCED_FACE ( 'NONE', ( #30985 ), #18556, .T. ) ;
#123628 = EDGE_LOOP ( 'NONE', ( #103262, #30410 ) ) ;
#123629 = CARTESIAN_POINT ( 'NONE',  ( -12.89999999999999147, 2.500000000000000000, -5.022947341949751454 ) ) ;
#123630 = LINE ( 'NONE', #33982, #52012 ) ;
#123631 = ORIENTED_EDGE ( 'NONE', *, *, #98264, .F. ) ;
#123632 = FACE_OUTER_BOUND ( 'NONE', #85381, .T. ) ;
#123633 = DIRECTION ( 'NONE',  ( 0.000000000000000000, 0.000000000000000000, -1.000000000000000000 ) ) ;
#123634 = EDGE_CURVE ( 'NONE', #93851, #114560, #66784, .T. ) ;
#123635 = ORIENTED_EDGE ( 'NONE', *, *, #115816, .F. ) ;
#123636 = DIRECTION ( 'NONE',  ( 0.000000000000000000, -0.000000000000000000, 1.000000000000000000 ) ) ;
#123637 = DIRECTION ( 'NONE',  ( 0.000000000000000000, 0.000000000000000000, 1.000000000000000000 ) ) ;
#123638 = ORIENTED_EDGE ( 'NONE', *, *, #27649, .F. ) ;
#123639 = DIRECTION ( 'NONE',  ( -4.274815082592931898E-19, -0.9999939076577903929, -0.003490651415223739937 ) ) ;
#123640 = DIRECTION ( 'NONE',  ( -0.000000000000000000, 1.000000000000000000, -0.000000000000000000 ) ) ;
#123641 = CARTESIAN_POINT ( 'NONE',  ( -11.04999999999999893, 2.500000000000000000, 6.148780366869520009 ) ) ;
#123642 = ORIENTED_EDGE ( 'NONE', *, *, #59657, .F. ) ;
#123643 = EDGE_LOOP ( 'NONE', ( #10193, #111151 ) ) ;
#123644 = CARTESIAN_POINT ( 'NONE',  ( -1.050000000000037348, 2.500000000000000000, -2.611473670974877592 ) ) ;
#123645 = ADVANCED_FACE ( 'NONE', ( #68291 ), #41447, .T. ) ;
#123646 = CIRCLE ( 'NONE', #111126, 0.1000000000000002554 ) ;
#123647 = ORIENTED_EDGE ( 'NONE', *, *, #76299, .F. ) ;
#123648 = CARTESIAN_POINT ( 'NONE',  ( -1.700000000000035261, 2.500000000000000000, 4.430127018922196847 ) ) ;
#123649 = CIRCLE ( 'NONE', #56741, 0.06509327318403745899 ) ;
#123650 = CARTESIAN_POINT ( 'NONE',  ( 12.49999999999990408, 12.50000000000000000, 5.022947341949748790 ) ) ;
#123651 = ORIENTED_EDGE ( 'NONE', *, *, #82837, .T. ) ;
#123652 = CIRCLE ( 'NONE', #27803, 0.06509327318403745899 ) ;
#123653 = CARTESIAN_POINT ( 'NONE',  ( -6.900000000000019007, 2.500000000000000000, 0.4464101615137735513 ) ) ;
#123654 = CARTESIAN_POINT ( 'NONE',  ( -0.6500000000000394351, 12.50000000000000000, 6.841600689897072485 ) ) ;
#123655 = CARTESIAN_POINT ( 'NONE',  ( -4.800000000000026468, 12.50000000000000000, -4.611443907251940644 ) ) ;
#123656 = LINE ( 'NONE', #16277, #96663 ) ;
#123657 = FACE_OUTER_BOUND ( 'NONE', #94411, .T. ) ;
#123658 = VECTOR ( 'NONE', #126671, 1000.000000000000000 ) ;
#123659 = ORIENTED_EDGE ( 'NONE', *, *, #109624, .F. ) ;
#123660 = VERTEX_POINT ( 'NONE', #24365 ) ;
#123661 = LINE ( 'NONE', #116427, #114306 ) ;
#123662 = EDGE_CURVE ( 'NONE', #52089, #92128, #85668, .T. ) ;
#123663 = CARTESIAN_POINT ( 'NONE',  ( 103.6810955943362558, 7.274704100468963652, -2.539691767268741351 ) ) ;
#123665 = ORIENTED_EDGE ( 'NONE', *, *, #33148, .F. ) ;
#123664 = VERTEX_POINT ( 'NONE', #2784 ) ;
#123666 = ORIENTED_EDGE ( 'NONE', *, *, #12308, .T. ) ;
#123667 = DIRECTION ( 'NONE',  ( 0.000000000000000000, 0.000000000000000000, 1.000000000000000000 ) ) ;
#123668 = CIRCLE ( 'NONE', #63054, 0.1000000000000002554 ) ;
#123669 = DIRECTION ( 'NONE',  ( -0.000000000000000000, 1.000000000000000000, -0.000000000000000000 ) ) ;
#123670 = DIRECTION ( 'NONE',  ( 0.4999999999999471534, 0.000000000000000000, -0.8660254037844692387 ) ) ;
#123671 = DIRECTION ( 'NONE',  ( 1.000000000000000000, 0.000000000000000000, 0.000000000000000000 ) ) ;
#123672 = DIRECTION ( 'NONE',  ( -1.000000000000000000, -0.000000000000000000, -0.000000000000000000 ) ) ;
#123673 = AXIS2_PLACEMENT_3D ( 'NONE', #73410, #61686, #52482 ) ;
#123674 = AXIS2_PLACEMENT_3D ( 'NONE', #101178, #41638, #81537 ) ;
#123675 = CARTESIAN_POINT ( 'NONE',  ( 7.099999999999926814, 2.500000000000000000, -0.1000000000000022815 ) ) ;
#123676 = DIRECTION ( 'NONE',  ( 0.000000000000000000, 0.000000000000000000, -1.000000000000000000 ) ) ;
#123677 = DIRECTION ( 'NONE',  ( 0.000000000000000000, 0.000000000000000000, 1.000000000000000000 ) ) ;
#123678 = DIRECTION ( 'NONE',  ( 0.000000000000000000, 0.000000000000000000, 1.000000000000000000 ) ) ;
#123679 = ADVANCED_FACE ( 'NONE', ( #104205 ), #94377, .T. ) ;
#123680 = CARTESIAN_POINT ( 'NONE',  ( 2.299999999999948752, 2.500000000000000000, 0.3464101615137735735 ) ) ;
#123681 = VERTEX_POINT ( 'NONE', #42744 ) ;
#123682 = CARTESIAN_POINT ( 'NONE',  ( 4.799999999999935874, 12.50000000000000000, 3.983716857408420964 ) ) ;
#123683 = EDGE_LOOP ( 'NONE', ( #50201, #35805 ) ) ;
#123684 = EDGE_CURVE ( 'NONE', #63642, #105966, #52239, .T. ) ;
#123685 = EDGE_LOOP ( 'NONE', ( #88266, #30884 ) ) ;
#123686 = DIRECTION ( 'NONE',  ( 0.000000000000000000, 0.000000000000000000, -1.000000000000000000 ) ) ;
#123687 = LINE ( 'NONE', #95548, #23845 ) ;
#123688 = CARTESIAN_POINT ( 'NONE',  ( 12.69999999999989804, 12.50000000000000000, 0.2813168883297361700 ) ) ;
#123689 = DIRECTION ( 'NONE',  ( 0.000000000000000000, 0.000000000000000000, -1.000000000000000000 ) ) ;
#123690 = CARTESIAN_POINT ( 'NONE',  ( -1.850000000000033840, 12.50000000000000000, 6.906693963081109722 ) ) ;
#123691 = DIRECTION ( 'NONE',  ( 0.000000000000000000, 1.000000000000000000, 0.000000000000000000 ) ) ;
#123692 = VECTOR ( 'NONE', #3219, 1000.000000000000000 ) ;
#123693 = CARTESIAN_POINT ( 'NONE',  ( -7.900000000000011013, 12.50000000000000000, 4.330127018922196314 ) ) ;
#123694 = EDGE_LOOP ( 'NONE', ( #122743, #72873 ) ) ;
#123695 = DIRECTION ( 'NONE',  ( 0.000000000000000000, 0.000000000000000000, 1.000000000000000000 ) ) ;
#123696 = CIRCLE ( 'NONE', #44289, 0.06509327318403745899 ) ;
#123697 = AXIS2_PLACEMENT_3D ( 'NONE', #24388, #64303, #104233 ) ;
#123698 = DIRECTION ( 'NONE',  ( -0.000000000000000000, -1.000000000000000000, -0.000000000000000000 ) ) ;
#123699 = ORIENTED_EDGE ( 'NONE', *, *, #45471, .T. ) ;
#123700 = VECTOR ( 'NONE', #33317, 1000.000000000000000 ) ;
#123701 = VERTEX_POINT ( 'NONE', #2134 ) ;
#123702 = EDGE_CURVE ( 'NONE', #64648, #62406, #20841, .T. ) ;
#123703 = ORIENTED_EDGE ( 'NONE', *, *, #104388, .F. ) ;
#123704 = VECTOR ( 'NONE', #67125, 1000.000000000000000 ) ;
#123705 = CIRCLE ( 'NONE', #88193, 0.1000000000000002554 ) ;
#123706 = ORIENTED_EDGE ( 'NONE', *, *, #5425, .T. ) ;
#123707 = DIRECTION ( 'NONE',  ( -4.274815082592931898E-19, -0.9999939076577903929, -0.003490651415223739937 ) ) ;
#123708 = CARTESIAN_POINT ( 'NONE',  ( 8.099999999999923261, 2.500000000000000000, 3.983716857408420076 ) ) ;
#123709 = AXIS2_PLACEMENT_3D ( 'NONE', #75031, #4323, #73724 ) ;
#123710 = EDGE_CURVE ( 'NONE', #90525, #48509, #79436, .T. ) ;
#123711 = CARTESIAN_POINT ( 'NONE',  ( 11.64999999999990798, 12.50000000000000000, 5.802370205355744659 ) ) ;
#123712 = CARTESIAN_POINT ( 'NONE',  ( -1.650000000000034328, 2.500000000000000000, -2.165063509461101710 ) ) ;
#123713 = DIRECTION ( 'NONE',  ( 0.000000000000000000, -0.9999939076577903929, 0.003490651415223739937 ) ) ;
#123714 = ORIENTED_EDGE ( 'NONE', *, *, #21225, .T. ) ;
#123715 = CARTESIAN_POINT ( 'NONE',  ( -10.65000000000000213, 2.500000000000000000, 1.918653347947321564 ) ) ;
#123716 = ADVANCED_FACE ( 'NONE', ( #82649 ), #12504, .T. ) ;
#123717 = EDGE_CURVE ( 'NONE', #61997, #121356, #123214, .T. ) ;
#123718 = EDGE_CURVE ( 'NONE', #113976, #27106, #93992, .T. ) ;
#123719 = CARTESIAN_POINT ( 'NONE',  ( -5.850000000000022737, 2.500000000000000000, -2.165063509461101710 ) ) ;
#123720 = EDGE_CURVE ( 'NONE', #16557, #111056, #13232, .T. ) ;
#123721 = DIRECTION ( 'NONE',  ( 0.000000000000000000, 0.000000000000000000, 1.000000000000000000 ) ) ;
#123722 = ORIENTED_EDGE ( 'NONE', *, *, #103648, .F. ) ;
#123723 = ORIENTED_EDGE ( 'NONE', *, *, #19830, .T. ) ;
#123725 = EDGE_LOOP ( 'NONE', ( #56850, #19737 ) ) ;
#123724 = ADVANCED_FACE ( 'NONE', ( #54456 ), #51901, .T. ) ;
#123726 = DIRECTION ( 'NONE',  ( 0.000000000000000000, 0.000000000000000000, -1.000000000000000000 ) ) ;
#123727 = ADVANCED_FACE ( 'NONE', ( #122570 ), #12592, .T. ) ;
#123728 = CARTESIAN_POINT ( 'NONE',  ( -11.05000000000000249, 2.500000000000000000, -6.248780366869523206 ) ) ;
#123729 = CIRCLE ( 'NONE', #42284, 0.1000000000000002554 ) ;
#123730 = CARTESIAN_POINT ( 'NONE',  ( 154.1524742528378056, 2.500000000000000000, -1.703575533167231537 ) ) ;
#123732 = ADVANCED_FACE ( 'NONE', ( #11955 ), #45982, .T. ) ;
#123731 = VECTOR ( 'NONE', #91849, 1000.000000000000000 ) ;
#123733 = EDGE_CURVE ( 'NONE', #39644, #4240, #18767, .T. ) ;
#123734 = ORIENTED_EDGE ( 'NONE', *, *, #99248, .F. ) ;
#123735 = DIRECTION ( 'NONE',  ( -0.000000000000000000, -1.000000000000000000, -0.000000000000000000 ) ) ;
#123736 = CARTESIAN_POINT ( 'NONE',  ( 6.899999999999928413, 12.50000000000000000, 3.918623584224383727 ) ) ;
#123737 = DIRECTION ( 'NONE',  ( 0.000000000000000000, 1.000000000000000000, 0.000000000000000000 ) ) ;
#123738 = FACE_OUTER_BOUND ( 'NONE', #97733, .T. ) ;
#123740 = EDGE_CURVE ( 'NONE', #96862, #33099, #100259, .T. ) ;
#123739 = AXIS2_PLACEMENT_3D ( 'NONE', #61963, #13481, #92708 ) ;
#123741 = CONICAL_SURFACE ( 'NONE', #52654, 0.1000000000000000472, 0.003490658503988666988 ) ;
#123742 = AXIS2_PLACEMENT_3D ( 'NONE', #116636, #75421, #115324 ) ;
#123743 = CARTESIAN_POINT ( 'NONE',  ( 14.14999999999989555, 2.500000000000000000, 2.165063509461097713 ) ) ;
#123744 = CIRCLE ( 'NONE', #10866, 0.1000000000000000472 ) ;
#123745 = EDGE_LOOP ( 'NONE', ( #28781, #123469, #52387, #117109 ) ) ;
#123746 = ORIENTED_EDGE ( 'NONE', *, *, #62734, .F. ) ;
#123747 = LINE ( 'NONE', #74027, #81474 ) ;
#123748 = DIRECTION ( 'NONE',  ( 0.000000000000000000, 0.000000000000000000, 1.000000000000000000 ) ) ;
#123749 = DIRECTION ( 'NONE',  ( 0.000000000000000000, 0.000000000000000000, 1.000000000000000000 ) ) ;
#123751 = FACE_OUTER_BOUND ( 'NONE', #75319, .T. ) ;
#123750 = AXIS2_PLACEMENT_3D ( 'NONE', #24932, #70329, #4607 ) ;
#123753 = DIRECTION ( 'NONE',  ( -0.000000000000000000, -1.000000000000000000, -0.000000000000000000 ) ) ;
#123752 = AXIS2_PLACEMENT_3D ( 'NONE', #59084, #129135, #110111 ) ;
#123754 = VERTEX_POINT ( 'NONE', #62994 ) ;
#123755 = CIRCLE ( 'NONE', #10861, 0.06509327318403745899 ) ;
#123756 = CIRCLE ( 'NONE', #48471, 0.06509327318403743123 ) ;
#123757 = AXIS2_PLACEMENT_3D ( 'NONE', #4050, #53801, #71506 ) ;
#123758 = ORIENTED_EDGE ( 'NONE', *, *, #64492, .F. ) ;
#123759 = DIRECTION ( 'NONE',  ( 0.000000000000000000, 0.000000000000000000, 1.000000000000000000 ) ) ;
#123760 = CARTESIAN_POINT ( 'NONE',  ( 8.149999999999923972, 2.500000000000000000, 2.611473670974873151 ) ) ;
#123761 = CARTESIAN_POINT ( 'NONE',  ( 3.149999999999944400, 12.50000000000000000, 2.511473670974873507 ) ) ;
#123762 = CIRCLE ( 'NONE', #52684, 0.06509327318403745899 ) ;
#123763 = DIRECTION ( 'NONE',  ( 0.000000000000000000, 0.000000000000000000, -1.000000000000000000 ) ) ;
#123764 = ORIENTED_EDGE ( 'NONE', *, *, #23724, .F. ) ;
#123765 = DIRECTION ( 'NONE',  ( -0.000000000000000000, 1.000000000000000000, -0.000000000000000000 ) ) ;
#123766 = DIRECTION ( 'NONE',  ( 0.000000000000000000, 0.000000000000000000, 1.000000000000000000 ) ) ;
#123767 = AXIS2_PLACEMENT_3D ( 'NONE', #25590, #58945, #117832 ) ;
#123768 = ORIENTED_EDGE ( 'NONE', *, *, #41777, .T. ) ;
#123769 = CARTESIAN_POINT ( 'NONE',  ( -2.900000000000030109, 12.50000000000000000, 0.6928203230275494784 ) ) ;
#123770 = EDGE_LOOP ( 'NONE', ( #11590, #61601 ) ) ;
#123771 = DIRECTION ( 'NONE',  ( -0.000000000000000000, -1.000000000000000000, -0.000000000000000000 ) ) ;
#123772 = ADVANCED_FACE ( 'NONE', ( #112750 ), #102407, .T. ) ;
#123773 = ORIENTED_EDGE ( 'NONE', *, *, #74344, .T. ) ;
#123774 = DIRECTION ( 'NONE',  ( 0.000000000000000000, 1.000000000000000000, 0.000000000000000000 ) ) ;
#123775 = FACE_OUTER_BOUND ( 'NONE', #94573, .T. ) ;
#123776 = EDGE_CURVE ( 'NONE', #71314, #102506, #101642, .T. ) ;
#123777 = VERTEX_POINT ( 'NONE', #114034 ) ;
#123778 = ORIENTED_EDGE ( 'NONE', *, *, #40246, .T. ) ;
#123779 = CARTESIAN_POINT ( 'NONE',  ( 187.0468750003414300, -8.734944146203032389, -1.604583208406768146E-15 ) ) ;
#123780 = DIRECTION ( 'NONE',  ( 0.000000000000000000, 1.000000000000000000, 0.000000000000000000 ) ) ;
#123781 = CARTESIAN_POINT ( 'NONE',  ( 184.6302083336747444, -4.367472073101514418, -7.564683531250002702 ) ) ;
#123782 = CARTESIAN_POINT ( 'NONE',  ( -12.94999999999999218, 2.500000000000000000, -2.165063509461099489 ) ) ;
#123783 = EDGE_CURVE ( 'NONE', #103364, #104181, #25570, .T. ) ;
#123784 = AXIS2_PLACEMENT_3D ( 'NONE', #60065, #51520, #70499 ) ;
#123785 = DIRECTION ( 'NONE',  ( 0.000000000000000000, 0.000000000000000000, -1.000000000000000000 ) ) ;
#123786 = DIRECTION ( 'NONE',  ( -4.274815082592931898E-19, -0.9999939076577903929, -0.003490651415223739937 ) ) ;
#123787 = AXIS2_PLACEMENT_3D ( 'NONE', #36203, #115360, #56460 ) ;
#123788 = AXIS2_PLACEMENT_3D ( 'NONE', #47902, #98919, #68164 ) ;
#123789 = CARTESIAN_POINT ( 'NONE',  ( -1.650000000000034328, 12.50000000000000000, -2.165063509461101710 ) ) ;
#123790 = CARTESIAN_POINT ( 'NONE',  ( 9.549999999999915445, 2.500000000000000000, -2.265063509461101798 ) ) ;
#123791 = VECTOR ( 'NONE', #26057, 1000.000000000000000 ) ;
#123793 = VERTEX_POINT ( 'NONE', #34784 ) ;
#123792 = AXIS2_PLACEMENT_3D ( 'NONE', #5873, #97496, #87027 ) ;
#123795 = ORIENTED_EDGE ( 'NONE', *, *, #101946, .T. ) ;
#123794 = AXIS2_PLACEMENT_3D ( 'NONE', #9235, #89087, #69425 ) ;
#123796 = DIRECTION ( 'NONE',  ( -0.000000000000000000, 1.000000000000000000, -0.000000000000000000 ) ) ;
#123797 = ORIENTED_EDGE ( 'NONE', *, *, #48023, .T. ) ;
#123798 = DIRECTION ( 'NONE',  ( -0.000000000000000000, 1.000000000000000000, -0.000000000000000000 ) ) ;
#123799 = DIRECTION ( 'NONE',  ( 0.000000000000000000, 0.000000000000000000, 1.000000000000000000 ) ) ;
#123800 = AXIS2_PLACEMENT_3D ( 'NONE', #126583, #99056, #49331 ) ;
#123801 = DIRECTION ( 'NONE',  ( -4.274815082592931898E-19, -0.9999939076577903929, -0.003490651415223739937 ) ) ;
#123804 = EDGE_LOOP ( 'NONE', ( #63757, #126399, #116883, #43924 ) ) ;
#123803 = ORIENTED_EDGE ( 'NONE', *, *, #83244, .T. ) ;
#123802 = AXIS2_PLACEMENT_3D ( 'NONE', #75232, #125609, #18245 ) ;
#123805 = DIRECTION ( 'NONE',  ( 0.000000000000000000, 1.000000000000000000, 0.000000000000000000 ) ) ;
#123806 = ORIENTED_EDGE ( 'NONE', *, *, #18506, .F. ) ;
#123807 = DIRECTION ( 'NONE',  ( 0.000000000000000000, 0.000000000000000000, 1.000000000000000000 ) ) ;
#123808 = DIRECTION ( 'NONE',  ( 0.000000000000000000, 0.000000000000000000, 1.000000000000000000 ) ) ;
#123809 = VECTOR ( 'NONE', #24723, 1000.000000000000000 ) ;
#123810 = VERTEX_POINT ( 'NONE', #94981 ) ;
#123811 = CARTESIAN_POINT ( 'NONE',  ( 4.799999999999935874, 12.50000000000000000, 0.2813168883297361700 ) ) ;
#123812 = CARTESIAN_POINT ( 'NONE',  ( -9.600000000000008527, 2.500000000000000000, 0.09999999999999761857 ) ) ;
#123813 = CARTESIAN_POINT ( 'NONE',  ( -9.600000000000008527, 2.500000000000000000, -4.430127018922197735 ) ) ;
#123814 = DIRECTION ( 'NONE',  ( 0.000000000000000000, 0.000000000000000000, -1.000000000000000000 ) ) ;
#123815 = CARTESIAN_POINT ( 'NONE',  ( 184.5000000000000000, 0.000000000000000000, -7.699999999999999289 ) ) ;
#123816 = CARTESIAN_POINT ( 'NONE',  ( 11.89999999999990443, 2.500000000000000000, 0.2464101615137736789 ) ) ;
#123817 = CARTESIAN_POINT ( 'NONE',  ( 186.1093750003413732, 9.264065473108010111E-16, -7.564683531250000925 ) ) ;
#123818 = CARTESIAN_POINT ( 'NONE',  ( 4.799999999999935874, 12.50000000000000000, 3.918623584224383727 ) ) ;
#123819 = CARTESIAN_POINT ( 'NONE',  ( 1.649999999999951950, 2.500000000000000000, -7.188010851410854052 ) ) ;
#123820 = CIRCLE ( 'NONE', #124111, 0.06509327318403743123 ) ;
#123821 = EDGE_CURVE ( 'NONE', #35207, #54453, #87715, .T. ) ;
#123822 = ORIENTED_EDGE ( 'NONE', *, *, #15628, .F. ) ;
#123823 = ORIENTED_EDGE ( 'NONE', *, *, #38796, .T. ) ;
#123824 = ORIENTED_EDGE ( 'NONE', *, *, #45936, .T. ) ;
#123825 = FACE_OUTER_BOUND ( 'NONE', #6800, .T. ) ;
#123826 = ORIENTED_EDGE ( 'NONE', *, *, #126434, .T. ) ;
#123828 = VERTEX_POINT ( 'NONE', #45884 ) ;
#123827 = ORIENTED_EDGE ( 'NONE', *, *, #76362, .F. ) ;
#123829 = EDGE_LOOP ( 'NONE', ( #26817, #112143, #79215, #16536 ) ) ;
#123830 = CARTESIAN_POINT ( 'NONE',  ( -10.65000000000000213, 2.500000000000000000, 6.248780366869520542 ) ) ;
#123831 = AXIS2_PLACEMENT_3D ( 'NONE', #49396, #10709, #61130 ) ;
#123832 = AXIS2_PLACEMENT_3D ( 'NONE', #2986, #111652, #70433 ) ;
#123833 = FACE_OUTER_BOUND ( 'NONE', #17197, .T. ) ;
#123834 = CARTESIAN_POINT ( 'NONE',  ( 186.7500000000000000, 9.429780353434619030E-16, -7.700000000000000178 ) ) ;
#123835 = CARTESIAN_POINT ( 'NONE',  ( 185.5312500006828031, 9.429780353434619030E-16, -7.700000000000000178 ) ) ;
#123836 = EDGE_CURVE ( 'NONE', #10045, #121533, #112870, .T. ) ;
#123837 = DIRECTION ( 'NONE',  ( 0.000000000000000000, 0.000000000000000000, 1.000000000000000000 ) ) ;
#123838 = EDGE_CURVE ( 'NONE', #105977, #34711, #2038, .T. ) ;
#123839 = ORIENTED_EDGE ( 'NONE', *, *, #6121, .F. ) ;
#123840 = AXIS2_PLACEMENT_3D ( 'NONE', #34445, #35719, #83539 ) ;
#123841 = AXIS2_PLACEMENT_3D ( 'NONE', #120649, #19878, #99730 ) ;
#123842 = CARTESIAN_POINT ( 'NONE',  ( -12.94999999999999218, 2.500000000000000000, 2.165063509461101265 ) ) ;
#123843 = EDGE_LOOP ( 'NONE', ( #20435, #60359 ) ) ;
#123844 = ORIENTED_EDGE ( 'NONE', *, *, #105709, .T. ) ;
#123845 = AXIS2_PLACEMENT_3D ( 'NONE', #86714, #67046, #36975 ) ;
#123846 = VERTEX_POINT ( 'NONE', #66149 ) ;
#123847 = DIRECTION ( 'NONE',  ( 0.000000000000000000, 1.000000000000000000, 0.000000000000000000 ) ) ;
#123848 = VERTEX_POINT ( 'NONE', #106085 ) ;
#123849 = ADVANCED_FACE ( 'NONE', ( #26241 ), #56422, .T. ) ;
#123850 = ORIENTED_EDGE ( 'NONE', *, *, #77078, .T. ) ;
#123851 = ORIENTED_EDGE ( 'NONE', *, *, #11367, .F. ) ;
#123852 = AXIS2_PLACEMENT_3D ( 'NONE', #96230, #117147, #86411 ) ;
#123853 = CARTESIAN_POINT ( 'NONE',  ( -9.550000000000007816, 2.500000000000000000, -6.495190528383297135 ) ) ;
#123854 = AXIS2_PLACEMENT_3D ( 'NONE', #29469, #79847, #35858 ) ;
#123855 = DIRECTION ( 'NONE',  ( 0.000000000000000000, 0.000000000000000000, 1.000000000000000000 ) ) ;
#123856 = CARTESIAN_POINT ( 'NONE',  ( -0.8500000000000386136, 12.50000000000000000, 1.472243186433545459 ) ) ;
#123857 = DIRECTION ( 'NONE',  ( 0.000000000000000000, 1.000000000000000000, 0.000000000000000000 ) ) ;
#123858 = VECTOR ( 'NONE', #126932, 1000.000000000000000 ) ;
#123859 = CARTESIAN_POINT ( 'NONE',  ( 5.399999999999933742, 2.500000000000000000, -2.385244779468109755E-15 ) ) ;
#123860 = AXIS2_PLACEMENT_3D ( 'NONE', #34041, #15010, #63509 ) ;
#123861 = CIRCLE ( 'NONE', #126003, 0.06509327318403745899 ) ;
#123862 = CARTESIAN_POINT ( 'NONE',  ( 16.56576425165007649, 1.499999999999997113, 6.084390597445792359 ) ) ;
#123863 = AXIS2_PLACEMENT_3D ( 'NONE', #45733, #85643, #125559 ) ;
#123864 = CARTESIAN_POINT ( 'NONE',  ( -8.150000000000009237, 2.500000000000000000, 6.841600689897072485 ) ) ;
#123865 = EDGE_LOOP ( 'NONE', ( #41364, #52367 ) ) ;
#123866 = FACE_OUTER_BOUND ( 'NONE', #98219, .T. ) ;
#123867 = EDGE_LOOP ( 'NONE', ( #111010, #43589 ) ) ;
#123868 = AXIS2_PLACEMENT_3D ( 'NONE', #122379, #121715, #120437 ) ;
#123869 = DIRECTION ( 'NONE',  ( -0.000000000000000000, 1.000000000000000000, -0.000000000000000000 ) ) ;
#123870 = ORIENTED_EDGE ( 'NONE', *, *, #74001, .F. ) ;
#123871 = EDGE_LOOP ( 'NONE', ( #46979, #83955, #1854, #128107 ) ) ;
#123872 = CARTESIAN_POINT ( 'NONE',  ( -1.050000000000038236, 2.500000000000000000, -6.148780366869526226 ) ) ;
#123873 = CARTESIAN_POINT ( 'NONE',  ( 184.5677083336747444, -4.367472073101514418, -7.564683531250002702 ) ) ;
#123874 = ADVANCED_FACE ( 'NONE', ( #13820 ), #60650, .T. ) ;
#123875 = DIRECTION ( 'NONE',  ( 0.000000000000000000, 0.000000000000000000, -1.000000000000000000 ) ) ;
#123876 = ORIENTED_EDGE ( 'NONE', *, *, #103551, .F. ) ;
#123877 = DIRECTION ( 'NONE',  ( 0.000000000000000000, -0.9999939076577903929, 0.003490651415223739937 ) ) ;
#123878 = ORIENTED_EDGE ( 'NONE', *, *, #63218, .T. ) ;
#123879 = CARTESIAN_POINT ( 'NONE',  ( 3.949999999999942446, 2.500000000000000000, -2.511473670974877948 ) ) ;
#123880 = DIRECTION ( 'NONE',  ( 0.000000000000000000, 0.000000000000000000, -1.000000000000000000 ) ) ;
#123881 = AXIS2_PLACEMENT_3D ( 'NONE', #4571, #36010, #75920 ) ;
#123882 = EDGE_CURVE ( 'NONE', #41491, #116425, #56322, .T. ) ;
#123883 = DIRECTION ( 'NONE',  ( 0.000000000000000000, 0.000000000000000000, -1.000000000000000000 ) ) ;
#123884 = PLANE ( 'NONE',  #26251 ) ;
#123885 = ADVANCED_FACE ( 'NONE', ( #56324 ), #39819, .T. ) ;
#123886 = LINE ( 'NONE', #103626, #35489 ) ;
#123887 = ORIENTED_EDGE ( 'NONE', *, *, #6761, .T. ) ;
#123888 = CIRCLE ( 'NONE', #2604, 0.06509327318403743123 ) ;
#123889 = CIRCLE ( 'NONE', #21501, 0.09999999999999982514 ) ;
#123890 = EDGE_CURVE ( 'NONE', #23344, #30982, #10453, .T. ) ;
#123891 = AXIS2_PLACEMENT_3D ( 'NONE', #102770, #13097, #53051 ) ;
#123892 = EDGE_CURVE ( 'NONE', #34970, #118779, #6547, .T. ) ;
#123893 = EDGE_CURVE ( 'NONE', #5233, #19176, #106595, .T. ) ;
#123894 = VERTEX_POINT ( 'NONE', #84512 ) ;
#123895 = DIRECTION ( 'NONE',  ( -0.000000000000000000, -1.000000000000000000, -0.000000000000000000 ) ) ;
#123896 = DIRECTION ( 'NONE',  ( 0.000000000000000000, 1.000000000000000000, 0.000000000000000000 ) ) ;
#123897 = VECTOR ( 'NONE', #5214, 1000.000000000000000 ) ;
#123898 = CIRCLE ( 'NONE', #2614, 0.09999999999999982514 ) ;
#123899 = AXIS2_PLACEMENT_3D ( 'NONE', #126643, #27147, #67043 ) ;
#123900 = EDGE_CURVE ( 'NONE', #26093, #79044, #62793, .T. ) ;
#123901 = CONICAL_SURFACE ( 'NONE', #111367, 0.1000000000000002554, 0.003490658503988666988 ) ;
#123902 = VECTOR ( 'NONE', #98499, 1000.000000000000227 ) ;
#123903 = CIRCLE ( 'NONE', #50763, 0.06509327318403741736 ) ;
#123904 = CARTESIAN_POINT ( 'NONE',  ( 185.7135416670080588, 4.367472073101518859, -7.564683531249999149 ) ) ;
#123905 = LINE ( 'NONE', #94439, #111750 ) ;
#123906 = CARTESIAN_POINT ( 'NONE',  ( 3.549999999999944755, 12.50000000000000000, -2.576566944158915184 ) ) ;
#123907 = FACE_OUTER_BOUND ( 'NONE', #60204, .T. ) ;
#123908 = DIRECTION ( 'NONE',  ( -0.000000000000000000, 1.000000000000000000, -0.000000000000000000 ) ) ;
#123909 = ORIENTED_EDGE ( 'NONE', *, *, #114850, .F. ) ;
#123910 = ADVANCED_FACE ( 'NONE', ( #113970 ), #69030, .T. ) ;
#123911 = CIRCLE ( 'NONE', #2718, 0.06509327318403745899 ) ;
#123912 = CARTESIAN_POINT ( 'NONE',  ( 1.649999999999950617, 2.500000000000000000, 2.165063509461097713 ) ) ;
#123913 = FACE_OUTER_BOUND ( 'NONE', #30460, .T. ) ;
#123914 = CARTESIAN_POINT ( 'NONE',  ( -4.400000000000025224, 2.500000000000000000, 4.676537180435972552 ) ) ;
#123915 = ORIENTED_EDGE ( 'NONE', *, *, #103491, .T. ) ;
#123916 = CARTESIAN_POINT ( 'NONE',  ( 5.399999999999932854, 2.500000000000000000, 3.737306695894644371 ) ) ;
#123917 = AXIS2_PLACEMENT_3D ( 'NONE', #77552, #27812, #78224 ) ;
#123918 = ORIENTED_EDGE ( 'NONE', *, *, #13676, .T. ) ;
#123919 = CARTESIAN_POINT ( 'NONE',  ( 6.699999999999930012, 2.500000000000000000, -4.330127018922201643 ) ) ;
#123920 = ORIENTED_EDGE ( 'NONE', *, *, #16223, .T. ) ;
#123921 = CARTESIAN_POINT ( 'NONE',  ( -11.69999999999999929, 2.500000000000000000, 0.1000000000000017403 ) ) ;
#123922 = CARTESIAN_POINT ( 'NONE',  ( -8.950000000000008171, 12.50000000000000000, -2.511473670974877948 ) ) ;
#123923 = CARTESIAN_POINT ( 'NONE',  ( 4.549999999999935874, 2.500000000000000000, 6.495190528383297135 ) ) ;
#123924 = ORIENTED_EDGE ( 'NONE', *, *, #95730, .T. ) ;
#123925 = CIRCLE ( 'NONE', #80022, 0.06509327318403745899 ) ;
#123926 = AXIS2_PLACEMENT_3D ( 'NONE', #62330, #31573, #3395 ) ;
#123927 = CARTESIAN_POINT ( 'NONE',  ( 3.749999999999940492, 2.500000000000000000, 5.902370205355745192 ) ) ;
#123928 = CARTESIAN_POINT ( 'NONE',  ( 5.199999999999933564, 2.500000000000000000, 0.3464101615137735735 ) ) ;
#123929 = CONICAL_SURFACE ( 'NONE', #75816, 0.1000000000000002554, 0.003490658503988666988 ) ;
#123930 = ORIENTED_EDGE ( 'NONE', *, *, #16592, .T. ) ;
#123931 = CIRCLE ( 'NONE', #69561, 0.09999999999999982514 ) ;
#123932 = CARTESIAN_POINT ( 'NONE',  ( -5.450000000000019718, 2.500000000000000000, 6.495190528383297135 ) ) ;
#123933 = VECTOR ( 'NONE', #10559, 1000.000000000000000 ) ;
#123935 = ORIENTED_EDGE ( 'NONE', *, *, #47594, .F. ) ;
#123934 = EDGE_CURVE ( 'NONE', #25872, #37345, #92024, .T. ) ;
#123936 = ORIENTED_EDGE ( 'NONE', *, *, #120762, .T. ) ;
#123937 = DIRECTION ( 'NONE',  ( 0.000000000000000000, 0.000000000000000000, 1.000000000000000000 ) ) ;
#123938 = DIRECTION ( 'NONE',  ( 0.000000000000000000, 0.000000000000000000, -1.000000000000000000 ) ) ;
#123939 = PLANE ( 'NONE',  #82014 ) ;
#123940 = ORIENTED_EDGE ( 'NONE', *, *, #23131, .T. ) ;
#123941 = DIRECTION ( 'NONE',  ( 0.000000000000000000, 0.000000000000000000, -1.000000000000000000 ) ) ;
#123942 = CARTESIAN_POINT ( 'NONE',  ( -0.2000000000000412836, 2.500000000000000000, 4.676537180435972552 ) ) ;
#123943 = CONICAL_SURFACE ( 'NONE', #2768, 0.09999999999999999167, 0.003490658503988666988 ) ;
#123944 = ORIENTED_EDGE ( 'NONE', *, *, #95663, .F. ) ;
#123945 = EDGE_CURVE ( 'NONE', #99630, #12428, #12596, .T. ) ;
#123946 = DIRECTION ( 'NONE',  ( 0.000000000000000000, 0.000000000000000000, 1.000000000000000000 ) ) ;
#123947 = DIRECTION ( 'NONE',  ( 0.000000000000000000, 0.000000000000000000, -1.000000000000000000 ) ) ;
#123948 = AXIS2_PLACEMENT_3D ( 'NONE', #122911, #13577, #92144 ) ;
#123949 = AXIS2_PLACEMENT_3D ( 'NONE', #108580, #88268, #78499 ) ;
#123950 = AXIS2_PLACEMENT_3D ( 'NONE', #54927, #85030, #124972 ) ;
#123951 = LINE ( 'NONE', #114144, #52791 ) ;
#123952 = CYLINDRICAL_SURFACE ( 'NONE', #32577, 7.700000000000000178 ) ;
#123953 = DIRECTION ( 'NONE',  ( 0.000000000000000000, 1.000000000000000000, 0.000000000000000000 ) ) ;
#123954 = CARTESIAN_POINT ( 'NONE',  ( 6.699999999999930012, 2.500000000000000000, 4.330127018922196314 ) ) ;
#123955 = VECTOR ( 'NONE', #10311, 1000.000000000000000 ) ;
#123956 = DIRECTION ( 'NONE',  ( 0.000000000000000000, 1.000000000000000000, 0.000000000000000000 ) ) ;
#123957 = ORIENTED_EDGE ( 'NONE', *, *, #101850, .F. ) ;
#123958 = CONICAL_SURFACE ( 'NONE', #44554, 0.1000000000000002554, 0.003490658503988666988 ) ;
#123959 = VERTEX_POINT ( 'NONE', #85145 ) ;
#123960 = ORIENTED_EDGE ( 'NONE', *, *, #86057, .F. ) ;
#123961 = ORIENTED_EDGE ( 'NONE', *, *, #13004, .T. ) ;
#123962 = DIRECTION ( 'NONE',  ( 0.000000000000000000, 1.000000000000000000, 0.000000000000000000 ) ) ;
#123963 = LINE ( 'NONE', #13368, #123095 ) ;
#123964 = CARTESIAN_POINT ( 'NONE',  ( 3.349999999999945466, 12.50000000000000000, -6.560283801567339701 ) ) ;
#123965 = ORIENTED_EDGE ( 'NONE', *, *, #94959, .F. ) ;
#123966 = FACE_BOUND ( 'NONE', #73108, .T. ) ;
#123967 = DIRECTION ( 'NONE',  ( -0.000000000000000000, 1.000000000000000000, -0.000000000000000000 ) ) ;
#123968 = DIRECTION ( 'NONE',  ( 0.000000000000000000, 0.000000000000000000, -1.000000000000000000 ) ) ;
#123969 = CARTESIAN_POINT ( 'NONE',  ( -4.550000000000022915, 12.50000000000000000, 6.495190528383297135 ) ) ;
#123970 = DIRECTION ( 'NONE',  ( 0.000000000000000000, -0.000000000000000000, 1.000000000000000000 ) ) ;
#123971 = DIRECTION ( 'NONE',  ( 0.000000000000000000, -0.000000000000000000, 1.000000000000000000 ) ) ;
#123972 = CARTESIAN_POINT ( 'NONE',  ( 185.2500000000000000, 9.429780353434619030E-16, -7.700000000000000178 ) ) ;
#123973 = PLANE ( 'NONE',  #64289 ) ;
#123974 = DIRECTION ( 'NONE',  ( 0.000000000000000000, 0.000000000000000000, 1.000000000000000000 ) ) ;
#123975 = AXIS2_PLACEMENT_3D ( 'NONE', #41934, #81832, #82504 ) ;
#123976 = DIRECTION ( 'NONE',  ( -0.000000000000000000, -1.000000000000000000, -0.000000000000000000 ) ) ;
#123977 = CARTESIAN_POINT ( 'NONE',  ( 7.699999999999923794, 12.50000000000000000, -3.918623584224389056 ) ) ;
#123978 = ORIENTED_EDGE ( 'NONE', *, *, #92914, .T. ) ;
#123979 = ADVANCED_FACE ( 'NONE', ( #75325 ), #115220, .T. ) ;
#123980 = VECTOR ( 'NONE', #42981, 1000.000000000000000 ) ;
#123981 = ORIENTED_EDGE ( 'NONE', *, *, #82485, .F. ) ;
#123982 = EDGE_LOOP ( 'NONE', ( #6952, #76381, #36387, #10424 ) ) ;
#123983 = EDGE_LOOP ( 'NONE', ( #77819, #55103, #43254, #45335 ) ) ;
#123984 = AXIS2_PLACEMENT_3D ( 'NONE', #91608, #41240, #52327 ) ;
#123985 = EDGE_LOOP ( 'NONE', ( #30007, #90853, #66213, #47094 ) ) ;
#123986 = VECTOR ( 'NONE', #79733, 1000.000000000000000 ) ;
#123987 = ORIENTED_EDGE ( 'NONE', *, *, #86649, .F. ) ;
#123988 = CONICAL_SURFACE ( 'NONE', #29913, 0.1000000000000000472, 0.003490658503988666988 ) ;
#123989 = DIRECTION ( 'NONE',  ( 0.000000000000000000, 1.000000000000000000, 0.000000000000000000 ) ) ;
#123990 = ORIENTED_EDGE ( 'NONE', *, *, #118368, .T. ) ;
#123991 = EDGE_LOOP ( 'NONE', ( #5449, #88188, #49039, #104477 ) ) ;
#123992 = EDGE_CURVE ( 'NONE', #79185, #126997, #37662, .T. ) ;
#123993 = VECTOR ( 'NONE', #108124, 1000.000000000000000 ) ;
#123994 = VECTOR ( 'NONE', #5721, 1000.000000000000000 ) ;
#123995 = VECTOR ( 'NONE', #22506, 1000.000000000000000 ) ;
#123996 = CARTESIAN_POINT ( 'NONE',  ( 9.112263991918540640, -2.499999999999490630, 9.392448312006209221 ) ) ;
#123997 = CARTESIAN_POINT ( 'NONE',  ( -11.69999999999999929, 2.500000000000000000, -4.430127018922199511 ) ) ;
#123998 = DIRECTION ( 'NONE',  ( -4.274815082592931898E-19, -0.9999939076577903929, -0.003490651415223739937 ) ) ;
#123999 = AXIS2_PLACEMENT_3D ( 'NONE', #98712, #100026, #10347 ) ;
#124000 = DIRECTION ( 'NONE',  ( 0.000000000000000000, 0.000000000000000000, -1.000000000000000000 ) ) ;
#124001 = VECTOR ( 'NONE', #80583, 1000.000000000000000 ) ;
#124002 = EDGE_CURVE ( 'NONE', #907, #36869, #36713, .T. ) ;
#124003 = ADVANCED_FACE ( 'NONE', ( #69368 ), #126371, .T. ) ;
#124004 = ORIENTED_EDGE ( 'NONE', *, *, #119584, .F. ) ;
#124005 = DIRECTION ( 'NONE',  ( 0.000000000000000000, 0.000000000000000000, 1.000000000000000000 ) ) ;
#124006 = AXIS2_PLACEMENT_3D ( 'NONE', #79939, #90387, #89762 ) ;
#124007 = ORIENTED_EDGE ( 'NONE', *, *, #126536, .F. ) ;
#124008 = ORIENTED_EDGE ( 'NONE', *, *, #68212, .F. ) ;
#124010 = ORIENTED_EDGE ( 'NONE', *, *, #115399, .T. ) ;
#124009 = PLANE ( 'NONE',  #7080 ) ;
#124011 = ADVANCED_FACE ( 'NONE', ( #99499 ), #47821, .T. ) ;
#124012 = CARTESIAN_POINT ( 'NONE',  ( -6.450000000000019718, 12.50000000000000000, -6.083687093685488989 ) ) ;
#124013 = ORIENTED_EDGE ( 'NONE', *, *, #93303, .T. ) ;
#124014 = ADVANCED_FACE ( 'NONE', ( #46505 ), #96209, .T. ) ;
#124015 = ORIENTED_EDGE ( 'NONE', *, *, #14023, .F. ) ;
#124016 = AXIS2_PLACEMENT_3D ( 'NONE', #114748, #22537, #24447 ) ;
#124017 = DIRECTION ( 'NONE',  ( 0.000000000000000000, 0.000000000000000000, -1.000000000000000000 ) ) ;
#124018 = CARTESIAN_POINT ( 'NONE',  ( 3.349999999999945466, 2.500000000000000000, -2.165063509461101710 ) ) ;
#124019 = DIRECTION ( 'NONE',  ( 0.000000000000000000, 0.000000000000000000, -1.000000000000000000 ) ) ;
#124020 = DIRECTION ( 'NONE',  ( 0.000000000000000000, 0.000000000000000000, 1.000000000000000000 ) ) ;
#124021 = DIRECTION ( 'NONE',  ( 0.000000000000000000, 0.000000000000000000, 1.000000000000000000 ) ) ;
#124023 = EDGE_LOOP ( 'NONE', ( #119180, #91519 ) ) ;
#124022 = CONICAL_SURFACE ( 'NONE', #107389, 0.1000000000000002554, 0.003490658503988666988 ) ;
#124024 = DIRECTION ( 'NONE',  ( -4.274815082592931898E-19, -0.9999939076577903929, -0.003490651415223739937 ) ) ;
#124025 = AXIS2_PLACEMENT_3D ( 'NONE', #114146, #63763, #25759 ) ;
#124026 = STYLED_ITEM ( 'NONE', ( #129001 ), #58784 ) ;
#124027 = EDGE_LOOP ( 'NONE', ( #72195, #108243, #30559, #37535 ) ) ;
#124028 = CARTESIAN_POINT ( 'NONE',  ( 17.50000000000000000, 2.499999999999999556, -2.666666666666662522 ) ) ;
#124029 = EDGE_LOOP ( 'NONE', ( #18045, #106743 ) ) ;
#124030 = LINE ( 'NONE', #55300, #68222 ) ;
#124031 = EDGE_CURVE ( 'NONE', #46603, #26800, #38659, .T. ) ;
#124032 = DIRECTION ( 'NONE',  ( -0.000000000000000000, -1.000000000000000000, -0.000000000000000000 ) ) ;
#124033 = DIRECTION ( 'NONE',  ( 0.000000000000000000, 0.000000000000000000, -1.000000000000000000 ) ) ;
#124035 = AXIS2_PLACEMENT_3D ( 'NONE', #62148, #97384, #27337 ) ;
#124034 = LINE ( 'NONE', #105030, #35490 ) ;
#124036 = ORIENTED_EDGE ( 'NONE', *, *, #35102, .T. ) ;
#124037 = AXIS2_PLACEMENT_3D ( 'NONE', #95991, #64586, #12418 ) ;
#124038 = CIRCLE ( 'NONE', #67589, 0.09999999999999999167 ) ;
#124039 = EDGE_CURVE ( 'NONE', #103404, #36921, #121278, .T. ) ;
#124040 = DIRECTION ( 'NONE',  ( -0.000000000000000000, 1.000000000000000000, -0.000000000000000000 ) ) ;
#124041 = ORIENTED_EDGE ( 'NONE', *, *, #124956, .T. ) ;
#124042 = ORIENTED_EDGE ( 'NONE', *, *, #37034, .T. ) ;
#124043 = ORIENTED_EDGE ( 'NONE', *, *, #30251, .F. ) ;
#124044 = DIRECTION ( 'NONE',  ( 0.000000000000000000, 0.000000000000000000, 1.000000000000000000 ) ) ;
#124045 = DIRECTION ( 'NONE',  ( 0.000000000000000000, 0.000000000000000000, -1.000000000000000000 ) ) ;
#124046 = CARTESIAN_POINT ( 'NONE',  ( 185.3177083336747160, 4.367472073101515306, 7.564683531250000925 ) ) ;
#124047 = AXIS2_PLACEMENT_3D ( 'NONE', #43680, #30147, #99530 ) ;
#124048 = LINE ( 'NONE', #125972, #3174 ) ;
#124049 = ADVANCED_FACE ( 'NONE', ( #108655 ), #112955, .T. ) ;
#124050 = DIRECTION ( 'NONE',  ( 0.000000000000000000, -1.000000000000000000, 0.000000000000000000 ) ) ;
#124051 = AXIS2_PLACEMENT_3D ( 'NONE', #50684, #88005, #68387 ) ;
#124052 = CIRCLE ( 'NONE', #42506, 0.09999999999999982514 ) ;
#124053 = DIRECTION ( 'NONE',  ( 0.000000000000000000, 0.000000000000000000, 1.000000000000000000 ) ) ;
#124054 = ADVANCED_FACE ( 'NONE', ( #68731 ), #125474, .T. ) ;
#124055 = VECTOR ( 'NONE', #127996, 1000.000000000000000 ) ;
#124056 = EDGE_CURVE ( 'NONE', #97932, #73695, #89876, .T. ) ;
#124057 = EDGE_CURVE ( 'NONE', #110043, #128895, #2141, .T. ) ;
#124058 = EDGE_LOOP ( 'NONE', ( #42427, #97028 ) ) ;
#124059 = CARTESIAN_POINT ( 'NONE',  ( 7.099999999999927702, 12.50000000000000000, -3.637306695894650055 ) ) ;
#124060 = ORIENTED_EDGE ( 'NONE', *, *, #91887, .F. ) ;
#124061 = EDGE_CURVE ( 'NONE', #14140, #65023, #66884, .T. ) ;
#124062 = CARTESIAN_POINT ( 'NONE',  ( 183.7812500006828031, 0.000000000000000000, 7.700000000000000178 ) ) ;
#124063 = CARTESIAN_POINT ( 'NONE',  ( 7.899999999999924860, 12.50000000000000000, -3.572213422710612374 ) ) ;
#124064 = CARTESIAN_POINT ( 'NONE',  ( -9.999999999999969802, 2.500000000000000000, -0.1000000000000022815 ) ) ;
#124065 = VERTEX_POINT ( 'NONE', #106712 ) ;
#124066 = ADVANCED_FACE ( 'NONE', ( #8507 ), #33460, .T. ) ;
#124067 = EDGE_CURVE ( 'NONE', #37140, #36953, #58285, .T. ) ;
#124068 = FACE_OUTER_BOUND ( 'NONE', #69182, .T. ) ;
#124069 = DIRECTION ( 'NONE',  ( 0.000000000000000000, 0.000000000000000000, 1.000000000000000000 ) ) ;
#124070 = VECTOR ( 'NONE', #6464, 1000.000000000000000 ) ;
#124071 = CONICAL_SURFACE ( 'NONE', #67630, 0.1000000000000002554, 0.003490658503988666988 ) ;
#124072 = VERTEX_POINT ( 'NONE', #7870 ) ;
#124073 = LINE ( 'NONE', #12810, #90685 ) ;
#124074 = CIRCLE ( 'NONE', #25879, 0.09999999999999982514 ) ;
#124075 = CIRCLE ( 'NONE', #84371, 0.06509327318403745899 ) ;
#124076 = EDGE_LOOP ( 'NONE', ( #69339, #114134, #92610, #125638 ) ) ;
#124077 = AXIS2_PLACEMENT_3D ( 'NONE', #18191, #79072, #118334 ) ;
#124078 = ORIENTED_EDGE ( 'NONE', *, *, #57255, .F. ) ;
#124079 = CARTESIAN_POINT ( 'NONE',  ( -1.450000000000036371, 2.500000000000000000, 6.841600689897072485 ) ) ;
#124080 = CIRCLE ( 'NONE', #11207, 0.1000000000000002554 ) ;
#124081 = CONICAL_SURFACE ( 'NONE', #92695, 0.1000000000000002554, 0.003490658503988666988 ) ;
#124082 = ORIENTED_EDGE ( 'NONE', *, *, #109678, .F. ) ;
#124083 = CARTESIAN_POINT ( 'NONE',  ( -12.69999999999999041, 2.500000000000000000, 3.983716857408420964 ) ) ;
#124084 = DIRECTION ( 'NONE',  ( 0.000000000000000000, 1.000000000000000000, 0.000000000000000000 ) ) ;
#124085 = CARTESIAN_POINT ( 'NONE',  ( -9.150000000000009237, 2.500000000000000000, -7.188010851410848723 ) ) ;
#124086 = VERTEX_POINT ( 'NONE', #28825 ) ;
#124087 = CIRCLE ( 'NONE', #84378, 0.1000000000000002554 ) ;
#124088 = CIRCLE ( 'NONE', #101107, 0.06509327318403745899 ) ;
#124089 = CARTESIAN_POINT ( 'NONE',  ( 5.449999999999936229, 2.500000000000000000, -2.265063509461101798 ) ) ;
#124091 = ORIENTED_EDGE ( 'NONE', *, *, #113227, .F. ) ;
#124090 = CARTESIAN_POINT ( 'NONE',  ( -11.25000000000000000, 12.50000000000000000, -2.792790559304612508 ) ) ;
#124092 = CIRCLE ( 'NONE', #63464, 0.1000000000000002554 ) ;
#124093 = CARTESIAN_POINT ( 'NONE',  ( -6.850000000000017408, 2.500000000000000000, -1.918653347947325782 ) ) ;
#124094 = LINE ( 'NONE', #115543, #25834 ) ;
#124095 = ORIENTED_EDGE ( 'NONE', *, *, #83944, .F. ) ;
#124096 = ORIENTED_EDGE ( 'NONE', *, *, #129551, .T. ) ;
#124097 = EDGE_LOOP ( 'NONE', ( #27325, #126905 ) ) ;
#124098 = DIRECTION ( 'NONE',  ( 0.000000000000000000, -0.000000000000000000, 1.000000000000000000 ) ) ;
#124099 = DIRECTION ( 'NONE',  ( -4.274815082592931898E-19, -0.9999939076577903929, -0.003490651415223739937 ) ) ;
#124100 = DIRECTION ( 'NONE',  ( 0.000000000000000000, 0.000000000000000000, -1.000000000000000000 ) ) ;
#124101 = FACE_BOUND ( 'NONE', #18963, .T. ) ;
#124102 = ORIENTED_EDGE ( 'NONE', *, *, #75003, .T. ) ;
#124103 = CARTESIAN_POINT ( 'NONE',  ( 186.6510416670080303, 4.367472073101518859, -7.564683531249999149 ) ) ;
#124104 = DIRECTION ( 'NONE',  ( -4.274815082592931898E-19, -0.9999939076577903929, -0.003490651415223739937 ) ) ;
#124105 = CARTESIAN_POINT ( 'NONE',  ( -10.40000000000000213, 2.500000000000000000, 4.922947341949748257 ) ) ;
#124106 = AXIS2_PLACEMENT_3D ( 'NONE', #112678, #32202, #123140 ) ;
#124107 = ADVANCED_FACE ( 'NONE', ( #77898 ), #118472, .T. ) ;
#124108 = DIRECTION ( 'NONE',  ( -0.000000000000000000, -1.000000000000000000, -0.000000000000000000 ) ) ;
#124109 = CARTESIAN_POINT ( 'NONE',  ( -7.100000000000018296, 2.500000000000000000, -2.385244779468109755E-15 ) ) ;
#124110 = DIRECTION ( 'NONE',  ( -0.000000000000000000, -1.000000000000000000, -0.000000000000000000 ) ) ;
#124111 = AXIS2_PLACEMENT_3D ( 'NONE', #69834, #60035, #99942 ) ;
#124112 = AXIS2_PLACEMENT_3D ( 'NONE', #23034, #40765, #10606 ) ;
#124113 = AXIS2_PLACEMENT_3D ( 'NONE', #18646, #57296, #97850 ) ;
#124114 = FACE_OUTER_BOUND ( 'NONE', #54402, .T. ) ;
#124115 = EDGE_LOOP ( 'NONE', ( #7197, #47925 ) ) ;
#124116 = VERTEX_POINT ( 'NONE', #39313 ) ;
#124117 = ORIENTED_EDGE ( 'NONE', *, *, #119183, .F. ) ;
#124118 = ORIENTED_EDGE ( 'NONE', *, *, #120735, .T. ) ;
#124119 = ORIENTED_EDGE ( 'NONE', *, *, #26222, .T. ) ;
#124120 = CARTESIAN_POINT ( 'NONE',  ( 3.299999999999944755, 2.500000000000000000, -0.1000000000000023925 ) ) ;
#124121 = CARTESIAN_POINT ( 'NONE',  ( -11.44999999999999929, 2.500000000000000000, -6.048780366869523029 ) ) ;
#124122 = ORIENTED_EDGE ( 'NONE', *, *, #57550, .F. ) ;
#124123 = FACE_BOUND ( 'NONE', #116117, .T. ) ;
#124124 = CIRCLE ( 'NONE', #82382, 0.06509327318403745899 ) ;
#124125 = CIRCLE ( 'NONE', #113672, 0.1000000000000002554 ) ;
#124126 = CARTESIAN_POINT ( 'NONE',  ( 3.099999999999945022, 12.50000000000000000, -0.2813168883297409439 ) ) ;
#124127 = VECTOR ( 'NONE', #103076, 1000.000000000000000 ) ;
#124128 = CONICAL_SURFACE ( 'NONE', #78179, 0.1000000000000002554, 0.003490658503988666988 ) ;
#124129 = CARTESIAN_POINT ( 'NONE',  ( 1.849999999999950129, 2.500000000000000000, -6.741600689897078169 ) ) ;
#124130 = ORIENTED_EDGE ( 'NONE', *, *, #79815, .F. ) ;
#124131 = CARTESIAN_POINT ( 'NONE',  ( 7.949999999999922018, 2.500000000000000000, -2.165063509461101710 ) ) ;
#124132 = FACE_OUTER_BOUND ( 'NONE', #13329, .T. ) ;
#124133 = DIRECTION ( 'NONE',  ( 0.000000000000000000, 1.000000000000000000, 0.000000000000000000 ) ) ;
#124134 = CONICAL_SURFACE ( 'NONE', #96943, 0.1000000000000000472, 0.003490658503988666988 ) ;
#124135 = ORIENTED_EDGE ( 'NONE', *, *, #113836, .F. ) ;
#124136 = FACE_OUTER_BOUND ( 'NONE', #441, .T. ) ;
#124137 = ORIENTED_EDGE ( 'NONE', *, *, #68874, .F. ) ;
#124138 = CIRCLE ( 'NONE', #19595, 0.06509327318403745899 ) ;
#124139 = AXIS2_PLACEMENT_3D ( 'NONE', #28843, #60250, #18360 ) ;
#124140 = VECTOR ( 'NONE', #61234, 1000.000000000000000 ) ;
#124141 = ORIENTED_EDGE ( 'NONE', *, *, #5834, .T. ) ;
#124142 = EDGE_LOOP ( 'NONE', ( #46258, #97296, #6295, #47618 ) ) ;
#124143 = FACE_OUTER_BOUND ( 'NONE', #45991, .T. ) ;
#124144 = DIRECTION ( 'NONE',  ( 0.000000000000000000, 0.000000000000000000, -1.000000000000000000 ) ) ;
#124146 = CIRCLE ( 'NONE', #126307, 0.06509327318403745899 ) ;
#124145 = LINE ( 'NONE', #102564, #67595 ) ;
#124147 = ORIENTED_EDGE ( 'NONE', *, *, #118762, .F. ) ;
#124148 = DIRECTION ( 'NONE',  ( -4.274815082592931898E-19, -0.9999939076577903929, -0.003490651415223739937 ) ) ;
#124149 = VECTOR ( 'NONE', #94477, 1000.000000000000000 ) ;
#124150 = ADVANCED_FACE ( 'NONE', ( #18978 ), #79516, .T. ) ;
#124151 = CARTESIAN_POINT ( 'NONE',  ( 105.6184301395928031, 8.500000000000000000, 1.375000000000001110 ) ) ;
#124152 = DIRECTION ( 'NONE',  ( -4.274815082592931898E-19, -0.9999939076577903929, -0.003490651415223739937 ) ) ;
#124153 = CARTESIAN_POINT ( 'NONE',  ( 186.0729166673494319, 4.445597072760120838, -7.699999999999998401 ) ) ;
#124154 = ORIENTED_EDGE ( 'NONE', *, *, #103221, .T. ) ;
#124155 = ADVANCED_FACE ( 'NONE', ( #89028 ), #29464, .T. ) ;
#124156 = DIRECTION ( 'NONE',  ( -0.000000000000000000, -1.000000000000000000, -0.000000000000000000 ) ) ;
#124157 = EDGE_CURVE ( 'NONE', #68489, #99244, #77367, .T. ) ;
#124158 = ORIENTED_EDGE ( 'NONE', *, *, #91696, .F. ) ;
#124159 = DIRECTION ( 'NONE',  ( 1.000000000000000000, 0.000000000000000000, 0.000000000000000000 ) ) ;
#124160 = ORIENTED_EDGE ( 'NONE', *, *, #41313, .T. ) ;
#124161 = ORIENTED_EDGE ( 'NONE', *, *, #99975, .F. ) ;
#124162 = DIRECTION ( 'NONE',  ( 0.000000000000000000, 0.000000000000000000, -1.000000000000000000 ) ) ;
#124163 = DIRECTION ( 'NONE',  ( 0.000000000000000000, 0.000000000000000000, 1.000000000000000000 ) ) ;
#124164 = EDGE_CURVE ( 'NONE', #62242, #49122, #81562, .T. ) ;
#124165 = EDGE_CURVE ( 'NONE', #46262, #40507, #54366, .T. ) ;
#124166 = AXIS2_PLACEMENT_3D ( 'NONE', #62709, #102609, #71220 ) ;
#124167 = CARTESIAN_POINT ( 'NONE',  ( -5.600000000000023626, 2.500000000000000000, -4.576537180435977348 ) ) ;
#124168 = ADVANCED_FACE ( 'NONE', ( #50384 ), #71977, .T. ) ;
#124169 = LINE ( 'NONE', #54145, #13271 ) ;
#124170 = EDGE_CURVE ( 'NONE', #515, #120902, #87807, .T. ) ;
#124171 = DIRECTION ( 'NONE',  ( 0.000000000000000000, 0.000000000000000000, -1.000000000000000000 ) ) ;
#124172 = EDGE_LOOP ( 'NONE', ( #93418, #7293, #50724, #1289 ) ) ;
#124173 = VERTEX_POINT ( 'NONE', #70034 ) ;
#124174 = CARTESIAN_POINT ( 'NONE',  ( 11.64999999999990798, 2.500000000000000000, -1.572243186433550211 ) ) ;
#124175 = AXIS2_PLACEMENT_3D ( 'NONE', #123919, #64361, #44081 ) ;
#124176 = AXIS2_PLACEMENT_3D ( 'NONE', #94581, #123401, #42952 ) ;
#124177 = AXIS2_PLACEMENT_3D ( 'NONE', #28458, #109592, #126652 ) ;
#124178 = CARTESIAN_POINT ( 'NONE',  ( 8.749999999999923617, 2.500000000000000000, -7.088010851410853519 ) ) ;
#124179 = AXIS2_PLACEMENT_3D ( 'NONE', #105002, #74277, #85377 ) ;
#124180 = FACE_OUTER_BOUND ( 'NONE', #77995, .T. ) ;
#124181 = B_SPLINE_CURVE_WITH_KNOTS ( 'NONE', 3,
 ( #9226, #49173, #50433, #70720, #119175, #29514, #69419, #59646, #99551, #80553, #9871, #120465, #39984, #30820, #110641, #100805, #91648, #12431, #72024, #1967, #51735, #22288, #81818, #73289, #34019, #33394, #43858, #113208, #102743, #123663, #113872, #103409, #23546, #74587, #43216, #41918, #34683, #24203, #102120, #44476, #53657 ),
 .UNSPECIFIED., .F., .F.,
 ( 4, 2, 2, 2, 2, 2, 2, 2, 2, 2, 2, 1, 2, 2, 2, 2, 2, 2, 2, 2, 4 ),
 ( 0.01611678554250517079, 0.01712107061916237974, 0.01762321315749096687, 0.01812535569581955053, 0.01912964077247668315, 0.02013392584913381925, 0.02113821092579095187, 0.02164035346411951818, 0.02214249600244808103, 0.02314678107910519977, 0.02364892361743375915, 0.02415106615576231505, 0.02465320869409087443, 0.02515535123241943033, 0.02615963630907655602, 0.02716392138573368170, 0.02816820646239080739, 0.02917249153904793307, 0.03017677661570505876, 0.03118106169236218098, 0.03218534676901930319 ),
 .UNSPECIFIED. ) ;
#124182 = ORIENTED_EDGE ( 'NONE', *, *, #74992, .F. ) ;
#124183 = VERTEX_POINT ( 'NONE', #42523 ) ;
#124184 = PLANE ( 'NONE',  #72855 ) ;
#124185 = EDGE_CURVE ( 'NONE', #12221, #2395, #64825, .T. ) ;
#124186 = ORIENTED_EDGE ( 'NONE', *, *, #8047, .F. ) ;
#124187 = CARTESIAN_POINT ( 'NONE',  ( 8.949999999999915801, 2.500000000000000000, 6.841600689897072485 ) ) ;
#124188 = AXIS2_PLACEMENT_3D ( 'NONE', #28136, #88314, #97509 ) ;
#124189 = CONICAL_SURFACE ( 'NONE', #107459, 0.09999999999999982514, 0.003490658503988666988 ) ;
#124190 = VECTOR ( 'NONE', #128992, 1000.000000000000000 ) ;
#124191 = DIRECTION ( 'NONE',  ( 0.000000000000000000, 0.000000000000000000, -1.000000000000000000 ) ) ;
#124192 = VERTEX_POINT ( 'NONE', #20281 ) ;
#124193 = FACE_OUTER_BOUND ( 'NONE', #17185, .T. ) ;
#124194 = CARTESIAN_POINT ( 'NONE',  ( -7.300000000000016698, 2.500000000000000000, -0.3464101615137783474 ) ) ;
#124195 = LINE ( 'NONE', #126121, #99041 ) ;
#124196 = CARTESIAN_POINT ( 'NONE',  ( 7.099999999999928590, 2.500000000000000000, -4.330127018922201643 ) ) ;
#124197 = VERTEX_POINT ( 'NONE', #52321 ) ;
#124198 = DIRECTION ( 'NONE',  ( 0.000000000000000000, 1.000000000000000000, 0.000000000000000000 ) ) ;
#124199 = CARTESIAN_POINT ( 'NONE',  ( 1.699999999999950218, 2.500000000000000000, 4.330127018922196314 ) ) ;
#124200 = CONICAL_SURFACE ( 'NONE', #113445, 0.1000000000000002554, 0.003490658503988666988 ) ;
#124201 = EDGE_LOOP ( 'NONE', ( #12452, #77442 ) ) ;
#124202 = ORIENTED_EDGE ( 'NONE', *, *, #33783, .F. ) ;
#124203 = EDGE_CURVE ( 'NONE', #44929, #114153, #9818, .T. ) ;
#124204 = CARTESIAN_POINT ( 'NONE',  ( 3.749999999999942268, 12.50000000000000000, -5.737276932171712751 ) ) ;
#124205 = CARTESIAN_POINT ( 'NONE',  ( 6.849999999999927702, 2.500000000000000000, 1.818653347947321475 ) ) ;
#124206 = DIRECTION ( 'NONE',  ( 0.000000000000000000, 0.000000000000000000, 1.000000000000000000 ) ) ;
#124207 = CIRCLE ( 'NONE', #99082, 0.06509327318403745899 ) ;
#124208 = FACE_OUTER_BOUND ( 'NONE', #22228, .T. ) ;
#124209 = DIRECTION ( 'NONE',  ( 0.000000000000000000, 1.000000000000000000, 0.000000000000000000 ) ) ;
#124210 = DIRECTION ( 'NONE',  ( 0.000000000000000000, 0.000000000000000000, 1.000000000000000000 ) ) ;
#124211 = CARTESIAN_POINT ( 'NONE',  ( 4.399999999999940847, 2.500000000000000000, -4.676537180435977881 ) ) ;
#124212 = LINE ( 'NONE', #2485, #7286 ) ;
#124213 = DIRECTION ( 'NONE',  ( -4.274815082592931898E-19, -0.9999939076577903929, -0.003490651415223739937 ) ) ;
#124214 = CARTESIAN_POINT ( 'NONE',  ( -7.100000000000018296, 2.500000000000000000, -0.1000000000000023925 ) ) ;
#124215 = EDGE_CURVE ( 'NONE', #38646, #6835, #64919, .T. ) ;
#124216 = ADVANCED_FACE ( 'NONE', ( #41871 ), #31406, .T. ) ;
#124217 = ADVANCED_FACE ( 'NONE', ( #86004 ), #110591, .F. ) ;
#124219 = VECTOR ( 'NONE', #60717, 1000.000000000000000 ) ;
#124218 = CARTESIAN_POINT ( 'NONE',  ( 8.149999999999920419, 2.500000000000000000, 6.248780366869521430 ) ) ;
#124220 = ORIENTED_EDGE ( 'NONE', *, *, #113398, .T. ) ;
#124221 = CIRCLE ( 'NONE', #63583, 0.06509327318403745899 ) ;
#124222 = ORIENTED_EDGE ( 'NONE', *, *, #96394, .F. ) ;
#124223 = ORIENTED_EDGE ( 'NONE', *, *, #97394, .F. ) ;
#124224 = ADVANCED_FACE ( 'NONE', ( #101425 ), #6401, .T. ) ;
#124225 = ORIENTED_EDGE ( 'NONE', *, *, #6816, .T. ) ;
#124226 = ADVANCED_FACE ( 'NONE', ( #22233 ), #77446, .T. ) ;
#124227 = DIRECTION ( 'NONE',  ( 0.000000000000000000, 0.000000000000000000, 1.000000000000000000 ) ) ;
#124228 = CARTESIAN_POINT ( 'NONE',  ( 11.64999999999990443, 12.50000000000000000, -5.802370205355749988 ) ) ;
#124229 = DIRECTION ( 'NONE',  ( 0.000000000000000000, 1.000000000000000000, 0.000000000000000000 ) ) ;
#124230 = ADVANCED_FACE ( 'NONE', ( #11087 ), #100435, .T. ) ;
#124231 = ORIENTED_EDGE ( 'NONE', *, *, #13676, .F. ) ;
#124232 = EDGE_CURVE ( 'NONE', #45669, #92207, #2217, .T. ) ;
#124233 = DIRECTION ( 'NONE',  ( -0.000000000000000000, 1.000000000000000000, -0.000000000000000000 ) ) ;
#124234 = VECTOR ( 'NONE', #14596, 1000.000000000000000 ) ;
#124235 = ADVANCED_FACE ( 'NONE', ( #41233 ), #4263, .T. ) ;
#124236 = DIRECTION ( 'NONE',  ( 0.000000000000000000, 1.000000000000000000, 0.000000000000000000 ) ) ;
#124238 = VERTEX_POINT ( 'NONE', #51689 ) ;
#124237 = DIRECTION ( 'NONE',  ( 0.000000000000000000, 0.000000000000000000, -1.000000000000000000 ) ) ;
#124239 = DIRECTION ( 'NONE',  ( 0.000000000000000000, -0.000000000000000000, 1.000000000000000000 ) ) ;
#124240 = EDGE_CURVE ( 'NONE', #69133, #78664, #106682, .T. ) ;
#124241 = DIRECTION ( 'NONE',  ( -0.000000000000000000, 1.000000000000000000, -0.000000000000000000 ) ) ;
#124242 = ORIENTED_EDGE ( 'NONE', *, *, #94338, .F. ) ;
#124243 = CIRCLE ( 'NONE', #101251, 0.1000000000000002554 ) ;
#124244 = AXIS2_PLACEMENT_3D ( 'NONE', #36418, #114943, #94667 ) ;
#124245 = ORIENTED_EDGE ( 'NONE', *, *, #90608, .F. ) ;
#124246 = ORIENTED_EDGE ( 'NONE', *, *, #104320, .F. ) ;
#124247 = VERTEX_POINT ( 'NONE', #55383 ) ;
#124248 = CYLINDRICAL_SURFACE ( 'NONE', #96784, 3.000000000000000444 ) ;
#124249 = CIRCLE ( 'NONE', #9311, 0.1000000000000002554 ) ;
#124250 = CARTESIAN_POINT ( 'NONE',  ( -2.900000000000029221, 2.500000000000000000, -4.922947341949753586 ) ) ;
#124251 = DIRECTION ( 'NONE',  ( 0.000000000000000000, 0.000000000000000000, -1.000000000000000000 ) ) ;
#124252 = CIRCLE ( 'NONE', #115833, 0.09999999999999982514 ) ;
#124253 = DIRECTION ( 'NONE',  ( -4.274815082592931898E-19, -0.9999939076577903929, -0.003490651415223739937 ) ) ;
#124254 = VERTEX_POINT ( 'NONE', #85482 ) ;
#124255 = FACE_OUTER_BOUND ( 'NONE', #67129, .T. ) ;
#124256 = ORIENTED_EDGE ( 'NONE', *, *, #94769, .F. ) ;
#124257 = PLANE ( 'NONE',  #55852 ) ;
#124258 = CARTESIAN_POINT ( 'NONE',  ( -7.050000000000013145, 2.500000000000000000, 6.395190528383296602 ) ) ;
#124259 = FACE_OUTER_BOUND ( 'NONE', #72068, .T. ) ;
#124260 = LINE ( 'NONE', #14285, #92355 ) ;
#124261 = ORIENTED_EDGE ( 'NONE', *, *, #37368, .T. ) ;
#124262 = AXIS2_PLACEMENT_3D ( 'NONE', #34055, #123691, #64788 ) ;
#124263 = EDGE_LOOP ( 'NONE', ( #15063, #13701, #92606, #100438 ) ) ;
#124264 = CONICAL_SURFACE ( 'NONE', #40663, 0.1000000000000002554, 0.003490658503988666988 ) ;
#124265 = ORIENTED_EDGE ( 'NONE', *, *, #4401, .F. ) ;
#124266 = CARTESIAN_POINT ( 'NONE',  ( -11.64999999999999680, 2.500000000000000000, -2.857883832488649745 ) ) ;
#124268 = AXIS2_PLACEMENT_3D ( 'NONE', #374, #60625, #69780 ) ;
#124267 = CARTESIAN_POINT ( 'NONE',  ( 7.099999999999926814, 12.50000000000000000, -0.6277270498435166823 ) ) ;
#124269 = AXIS2_PLACEMENT_3D ( 'NONE', #16886, #127531, #128849 ) ;
#124270 = LINE ( 'NONE', #5751, #77527 ) ;
#124271 = FACE_BOUND ( 'NONE', #72943, .T. ) ;
#124272 = DIRECTION ( 'NONE',  ( 0.000000000000000000, -0.9999939076577903929, 0.003490651415223739937 ) ) ;
#124273 = CARTESIAN_POINT ( 'NONE',  ( 5.199999999999933564, 12.50000000000000000, 3.983716857408420076 ) ) ;
#124274 = CARTESIAN_POINT ( 'NONE',  ( -11.44999999999999929, 2.500000000000000000, -6.148780366869522673 ) ) ;
#124275 = AXIS2_PLACEMENT_3D ( 'NONE', #19540, #78486, #71216 ) ;
#124276 = EDGE_CURVE ( 'NONE', #89750, #77424, #119296, .T. ) ;
#124277 = AXIS2_PLACEMENT_3D ( 'NONE', #49794, #90320, #28857 ) ;
#124278 = AXIS2_PLACEMENT_3D ( 'NONE', #1033, #13420, #91345 ) ;
#124279 = CARTESIAN_POINT ( 'NONE',  ( 186.7552083336747444, 6.551208109652275624, -3.782341765624998686 ) ) ;
#124280 = CARTESIAN_POINT ( 'NONE',  ( -14.99999999999998224, 2.500000000000000000, -0.6928203230275519209 ) ) ;
#124281 = DIRECTION ( 'NONE',  ( -0.000000000000000000, 1.000000000000000000, -0.000000000000000000 ) ) ;
#124282 = EDGE_LOOP ( 'NONE', ( #74898, #18781 ) ) ;
#124283 = VECTOR ( 'NONE', #92824, 1000.000000000000000 ) ;
#124284 = CIRCLE ( 'NONE', #95042, 0.06509327318403745899 ) ;
#124285 = DIRECTION ( 'NONE',  ( 0.000000000000000000, 0.000000000000000000, 1.000000000000000000 ) ) ;
#124286 = ORIENTED_EDGE ( 'NONE', *, *, #118860, .F. ) ;
#124287 = VERTEX_POINT ( 'NONE', #43168 ) ;
#124288 = ORIENTED_EDGE ( 'NONE', *, *, #82710, .F. ) ;
#124289 = VERTEX_POINT ( 'NONE', #3229 ) ;
#124290 = AXIS2_PLACEMENT_3D ( 'NONE', #86195, #107793, #16801 ) ;
#124291 = ADVANCED_FACE ( 'NONE', ( #37037 ), #127355, .T. ) ;
#124292 = PLANE ( 'NONE',  #121717 ) ;
#124293 = FACE_BOUND ( 'NONE', #45480, .T. ) ;
#124294 = DIRECTION ( 'NONE',  ( 0.000000000000000000, 1.000000000000000000, 0.000000000000000000 ) ) ;
#124295 = ORIENTED_EDGE ( 'NONE', *, *, #49592, .F. ) ;
#124296 = DIRECTION ( 'NONE',  ( 0.000000000000000000, 0.000000000000000000, 1.000000000000000000 ) ) ;
#124297 = CARTESIAN_POINT ( 'NONE',  ( -8.550000000000014921, 12.50000000000000000, -6.148780366869520897 ) ) ;
#124299 = ORIENTED_EDGE ( 'NONE', *, *, #35094, .T. ) ;
#124298 = AXIS2_PLACEMENT_3D ( 'NONE', #23766, #6648, #34243 ) ;
#124300 = DIRECTION ( 'NONE',  ( 0.000000000000000000, 0.000000000000000000, -1.000000000000000000 ) ) ;
#124301 = CARTESIAN_POINT ( 'NONE',  ( -2.100000000000033396, 12.50000000000000000, -5.022947341949754119 ) ) ;
#124302 = VERTEX_POINT ( 'NONE', #87401 ) ;
#124303 = PLANE ( 'NONE',  #65282 ) ;
#124304 = DIRECTION ( 'NONE',  ( 0.000000000000000000, 0.000000000000000000, 1.000000000000000000 ) ) ;
#124305 = AXIS2_PLACEMENT_3D ( 'NONE', #80206, #97891, #78926 ) ;
#124306 = CIRCLE ( 'NONE', #88709, 0.06509327318403745899 ) ;
#124307 = VERTEX_POINT ( 'NONE', #76955 ) ;
#124308 = EDGE_CURVE ( 'NONE', #92862, #123556, #92107, .T. ) ;
#124309 = FACE_OUTER_BOUND ( 'NONE', #36506, .T. ) ;
#124310 = FACE_OUTER_BOUND ( 'NONE', #24652, .T. ) ;
#124311 = CARTESIAN_POINT ( 'NONE',  ( 12.09999999999990550, 2.500000000000000000, -4.330127018922201643 ) ) ;
#124312 = EDGE_LOOP ( 'NONE', ( #68537, #100038 ) ) ;
#124313 = ORIENTED_EDGE ( 'NONE', *, *, #12632, .T. ) ;
#124314 = DIRECTION ( 'NONE',  ( 0.000000000000000000, 1.000000000000000000, 0.000000000000000000 ) ) ;
#124315 = EDGE_CURVE ( 'NONE', #126002, #96634, #105109, .T. ) ;
#124316 = ORIENTED_EDGE ( 'NONE', *, *, #18494, .T. ) ;
#124317 = DIRECTION ( 'NONE',  ( 0.000000000000000000, -0.9999939076577903929, 0.003490651415223739937 ) ) ;
#124318 = DIRECTION ( 'NONE',  ( 0.000000000000000000, 1.000000000000000000, 0.000000000000000000 ) ) ;
#124319 = AXIS2_PLACEMENT_3D ( 'NONE', #97046, #97683, #47307 ) ;
#124320 = ORIENTED_EDGE ( 'NONE', *, *, #69128, .T. ) ;
#124322 = FACE_OUTER_BOUND ( 'NONE', #34608, .T. ) ;
#124321 = CIRCLE ( 'NONE', #109948, 0.06509327318403745899 ) ;
#124323 = DIRECTION ( 'NONE',  ( -0.000000000000000000, 1.000000000000000000, -0.000000000000000000 ) ) ;
#124324 = CARTESIAN_POINT ( 'NONE',  ( 3.549999999999943867, 2.500000000000000000, -1.718653347947326049 ) ) ;
#124325 = EDGE_CURVE ( 'NONE', #42109, #50667, #98361, .T. ) ;
#124326 = EDGE_CURVE ( 'NONE', #97364, #60150, #125555, .T. ) ;
#124327 = DIRECTION ( 'NONE',  ( -0.000000000000000000, -1.000000000000000000, -0.000000000000000000 ) ) ;
#124328 = EDGE_CURVE ( 'NONE', #21032, #84876, #56008, .T. ) ;
#124329 = EDGE_CURVE ( 'NONE', #66137, #41959, #110887, .T. ) ;
#124330 = EDGE_CURVE ( 'NONE', #80079, #48784, #10536, .T. ) ;
#124331 = FACE_OUTER_BOUND ( 'NONE', #2398, .T. ) ;
#124332 = VERTEX_POINT ( 'NONE', #114928 ) ;
#124333 = VERTEX_POINT ( 'NONE', #65174 ) ;
#124334 = DIRECTION ( 'NONE',  ( 0.000000000000000000, 0.000000000000000000, 1.000000000000000000 ) ) ;
#124335 = CIRCLE ( 'NONE', #105558, 0.1000000000000000472 ) ;
#124336 = CARTESIAN_POINT ( 'NONE',  ( 1.849999999999949019, 12.50000000000000000, 6.841600689897072485 ) ) ;
#124337 = FACE_OUTER_BOUND ( 'NONE', #23137, .T. ) ;
#124339 = ORIENTED_EDGE ( 'NONE', *, *, #35118, .T. ) ;
#124338 = ORIENTED_EDGE ( 'NONE', *, *, #20285, .T. ) ;
#124340 = ORIENTED_EDGE ( 'NONE', *, *, #56022, .T. ) ;
#124341 = CIRCLE ( 'NONE', #1003, 0.09999999999999982514 ) ;
#124342 = EDGE_CURVE ( 'NONE', #84404, #44343, #127620, .T. ) ;
#124343 = DIRECTION ( 'NONE',  ( 0.000000000000000000, 1.000000000000000000, 0.000000000000000000 ) ) ;
#124344 = AXIS2_PLACEMENT_3D ( 'NONE', #91273, #1590, #11421 ) ;
#124345 = EDGE_CURVE ( 'NONE', #82981, #72411, #71183, .T. ) ;
#124346 = DIRECTION ( 'NONE',  ( 0.000000000000000000, 0.000000000000000000, 1.000000000000000000 ) ) ;
#124347 = ADVANCED_FACE ( 'NONE', ( #86762 ), #16862, .T. ) ;
#124348 = CARTESIAN_POINT ( 'NONE',  ( 12.89999999999990088, 12.50000000000000000, 4.330127018922196314 ) ) ;
#124349 = DIRECTION ( 'NONE',  ( 0.000000000000000000, 0.000000000000000000, 1.000000000000000000 ) ) ;
#124350 = DIRECTION ( 'NONE',  ( 0.000000000000000000, 0.000000000000000000, 1.000000000000000000 ) ) ;
#124351 = CARTESIAN_POINT ( 'NONE',  ( 2.099999999999949463, 12.50000000000000000, -3.637306695894650055 ) ) ;
#124352 = CARTESIAN_POINT ( 'NONE',  ( 7.699999999999923794, 2.500000000000000000, 4.676537180435972552 ) ) ;
#124353 = CARTESIAN_POINT ( 'NONE',  ( 10.84999999999991260, 12.50000000000000000, 6.495190528383297135 ) ) ;
#124354 = DIRECTION ( 'NONE',  ( 0.000000000000000000, 0.000000000000000000, -1.000000000000000000 ) ) ;
#124355 = CARTESIAN_POINT ( 'NONE',  ( -5.400000000000019895, 12.50000000000000000, -2.276824562219559311E-15 ) ) ;
#124356 = EDGE_LOOP ( 'NONE', ( #95015, #78617, #72416, #108212 ) ) ;
#124357 = VECTOR ( 'NONE', #27434, 1000.000000000000000 ) ;
#124358 = CIRCLE ( 'NONE', #44939, 0.09999999999999982514 ) ;
#124359 = CARTESIAN_POINT ( 'NONE',  ( 10.44999999999991047, 12.50000000000000000, -6.560283801567339701 ) ) ;
#124360 = CIRCLE ( 'NONE', #113899, 0.06509327318403745899 ) ;
#124361 = AXIS2_PLACEMENT_3D ( 'NONE', #91805, #72818, #29824 ) ;
#124362 = VERTEX_POINT ( 'NONE', #5611 ) ;
#124363 =( BOUNDED_CURVE ( )  B_SPLINE_CURVE ( 2, ( #6784, #24531, #75544, #104375, #23898, #54617, #63818 ),
 .UNSPECIFIED., .F., .T. ) 
 B_SPLINE_CURVE_WITH_KNOTS ( ( 3, 2, 2, 3 ),
 ( 0.7857142857142862535, 0.8095238095238102005, 0.8333333333333340365, 0.8571428571428578724 ),
 .UNSPECIFIED. ) 
 CURVE ( )  GEOMETRIC_REPRESENTATION_ITEM ( )  RATIONAL_B_SPLINE_CURVE ( ( 0.9999999999999968914, 0.8660254037844418162, 1.000000000000000000, 0.8660254037844387076, 1.000000000000000000, 0.8660254037844343777, 1.000000000000004441 ) ) 
 REPRESENTATION_ITEM ( '' )  );
#124364 = EDGE_LOOP ( 'NONE', ( #29406, #29813, #23437, #42230 ) ) ;
#124365 = CARTESIAN_POINT ( 'NONE',  ( 6.449999999999930012, 2.500000000000000000, 1.818653347947321475 ) ) ;
#124366 = DIRECTION ( 'NONE',  ( 0.000000000000000000, 0.000000000000000000, 1.000000000000000000 ) ) ;
#124367 = FACE_OUTER_BOUND ( 'NONE', #98472, .T. ) ;
#124368 = AXIS2_PLACEMENT_3D ( 'NONE', #91193, #111467, #38408 ) ;
#124369 = CARTESIAN_POINT ( 'NONE',  ( -2.950000000000033484, 2.500000000000000000, -6.495190528383302464 ) ) ;
#124371 = CARTESIAN_POINT ( 'NONE',  ( 8.099999999999923261, 2.500000000000000000, 3.883716857408420431 ) ) ;
#124370 = AXIS2_PLACEMENT_3D ( 'NONE', #36948, #127900, #76869 ) ;
#124372 = FACE_OUTER_BOUND ( 'NONE', #53060, .T. ) ;
#124373 = DIRECTION ( 'NONE',  ( 0.000000000000000000, 1.000000000000000000, 0.000000000000000000 ) ) ;
#124374 = ORIENTED_EDGE ( 'NONE', *, *, #33067, .T. ) ;
#124375 = DIRECTION ( 'NONE',  ( 0.000000000000000000, 0.000000000000000000, -1.000000000000000000 ) ) ;
#124376 = AXIS2_PLACEMENT_3D ( 'NONE', #16816, #68522, #85588 ) ;
#124377 = DIRECTION ( 'NONE',  ( 0.000000000000000000, 0.000000000000000000, 1.000000000000000000 ) ) ;
#124379 = ORIENTED_EDGE ( 'NONE', *, *, #64884, .F. ) ;
#124378 = AXIS2_PLACEMENT_3D ( 'NONE', #127432, #59353, #66557 ) ;
#124380 = CIRCLE ( 'NONE', #82716, 0.06509327318403741736 ) ;
#124381 = ORIENTED_EDGE ( 'NONE', *, *, #89241, .T. ) ;
#124382 = VERTEX_POINT ( 'NONE', #45571 ) ;
#124383 = CIRCLE ( 'NONE', #76357, 0.06509327318403745899 ) ;
#124384 = ADVANCED_FACE ( 'NONE', ( #52969 ), #104627, .T. ) ;
#124385 = VERTEX_POINT ( 'NONE', #25925 ) ;
#124386 = DIRECTION ( 'NONE',  ( 0.000000000000000000, 0.000000000000000000, -1.000000000000000000 ) ) ;
#124387 = FACE_OUTER_BOUND ( 'NONE', #126528, .T. ) ;
#124388 = ADVANCED_FACE ( 'NONE', ( #75648 ), #69126, .T. ) ;
#124389 = CARTESIAN_POINT ( 'NONE',  ( -1.250000000000001554, 12.50000000000000000, 6.560283801567334372 ) ) ;
#124390 = CARTESIAN_POINT ( 'NONE',  ( -4.350000000000023626, 2.500000000000000000, 2.611473670974873151 ) ) ;
#124391 = ADVANCED_FACE ( 'NONE', ( #67095 ), #102570, .T. ) ;
#124392 = CARTESIAN_POINT ( 'NONE',  ( 10.44999999999991402, 2.500000000000000000, 6.495190528383297135 ) ) ;
#124393 = ORIENTED_EDGE ( 'NONE', *, *, #129595, .F. ) ;
#124394 = DIRECTION ( 'NONE',  ( 0.000000000000000000, 0.000000000000000000, 1.000000000000000000 ) ) ;
#124395 = CARTESIAN_POINT ( 'NONE',  ( 7.099999999999928590, 2.500000000000000000, 3.537306695894645081 ) ) ;
#124396 = CIRCLE ( 'NONE', #126457, 0.06509327318403745899 ) ;
#124397 = EDGE_CURVE ( 'NONE', #98726, #85814, #46145, .T. ) ;
#124398 = CARTESIAN_POINT ( 'NONE',  ( 6.449999999999931788, 2.500000000000000000, -6.048780366869526581 ) ) ;
#124399 = ORIENTED_EDGE ( 'NONE', *, *, #48750, .F. ) ;
#124400 = ORIENTED_EDGE ( 'NONE', *, *, #46942, .T. ) ;
#124401 = EDGE_LOOP ( 'NONE', ( #119089, #97579 ) ) ;
#124402 = DIRECTION ( 'NONE',  ( 0.000000000000000000, -0.9999939076577903929, 0.003490651415223739937 ) ) ;
#124403 = CIRCLE ( 'NONE', #38751, 0.06509327318403745899 ) ;
#124404 = DIRECTION ( 'NONE',  ( -4.274815082592931898E-19, -0.9999939076577903929, -0.003490651415223739937 ) ) ;
#124405 = DIRECTION ( 'NONE',  ( 0.000000000000000000, 0.000000000000000000, 1.000000000000000000 ) ) ;
#124406 = ORIENTED_EDGE ( 'NONE', *, *, #72327, .F. ) ;
#124407 = DIRECTION ( 'NONE',  ( 0.000000000000000000, -0.9999939076577903929, 0.003490651415223739937 ) ) ;
#124408 = CARTESIAN_POINT ( 'NONE',  ( 8.349999999999923261, 2.500000000000000000, -5.802370205355749988 ) ) ;
#124409 = CARTESIAN_POINT ( 'NONE',  ( 13.54999999999989768, 2.500000000000000000, -2.611473670974877592 ) ) ;
#124410 = FACE_OUTER_BOUND ( 'NONE', #123394, .T. ) ;
#124411 = EDGE_CURVE ( 'NONE', #65296, #100903, #66962, .T. ) ;
#124412 = DIRECTION ( 'NONE',  ( 0.000000000000000000, 0.000000000000000000, 1.000000000000000000 ) ) ;
#124413 = CONICAL_SURFACE ( 'NONE', #57518, 0.1000000000000002554, 0.003490658503988666988 ) ;
#124414 = ORIENTED_EDGE ( 'NONE', *, *, #122875, .F. ) ;
#124415 = DIRECTION ( 'NONE',  ( 0.000000000000000000, 0.000000000000000000, -1.000000000000000000 ) ) ;
#124416 = CONICAL_SURFACE ( 'NONE', #122280, 0.09999999999999982514, 0.003490658503988666988 ) ;
#124417 = ORIENTED_EDGE ( 'NONE', *, *, #110304, .T. ) ;
#124418 = ORIENTED_EDGE ( 'NONE', *, *, #107530, .F. ) ;
#124419 = DIRECTION ( 'NONE',  ( 0.000000000000000000, 0.000000000000000000, 1.000000000000000000 ) ) ;
#124420 = DIRECTION ( 'NONE',  ( -0.000000000000000000, -1.000000000000000000, -0.000000000000000000 ) ) ;
#124421 = CARTESIAN_POINT ( 'NONE',  ( 10.84999999999991260, 2.500000000000000000, -1.472243186433550122 ) ) ;
#124422 = DIRECTION ( 'NONE',  ( 0.000000000000000000, 0.000000000000000000, -1.000000000000000000 ) ) ;
#124423 = CARTESIAN_POINT ( 'NONE',  ( -11.24999999999996447, 2.500000000000000000, -2.165063509461097713 ) ) ;
#124424 = ORIENTED_EDGE ( 'NONE', *, *, #38194, .F. ) ;
#124425 = AXIS2_PLACEMENT_3D ( 'NONE', #25920, #126700, #75019 ) ;
#124426 = EDGE_CURVE ( 'NONE', #120893, #36089, #23157, .T. ) ;
#124427 = ORIENTED_EDGE ( 'NONE', *, *, #73835, .F. ) ;
#124428 = DIRECTION ( 'NONE',  ( 0.000000000000000000, 0.000000000000000000, -1.000000000000000000 ) ) ;
#124429 = DIRECTION ( 'NONE',  ( -0.000000000000000000, 1.000000000000000000, -0.000000000000000000 ) ) ;
#124430 = DIRECTION ( 'NONE',  ( 0.000000000000000000, 0.000000000000000000, 1.000000000000000000 ) ) ;
#124431 = DIRECTION ( 'NONE',  ( -0.000000000000000000, -1.000000000000000000, -0.000000000000000000 ) ) ;
#124432 = EDGE_LOOP ( 'NONE', ( #52871, #116690, #17630, #38906 ) ) ;
#124433 = CARTESIAN_POINT ( 'NONE',  ( -0.4000000000000331624, 12.50000000000000000, 0.06509327318403743123 ) ) ;
#124434 = DIRECTION ( 'NONE',  ( -4.274815082592931898E-19, -0.9999939076577903929, -0.003490651415223739937 ) ) ;
#124435 = ORIENTED_EDGE ( 'NONE', *, *, #85496, .F. ) ;
#124436 = DIRECTION ( 'NONE',  ( -0.000000000000000000, 1.000000000000000000, -0.000000000000000000 ) ) ;
#124437 = EDGE_CURVE ( 'NONE', #67445, #126716, #50715, .T. ) ;
#124438 = AXIS2_PLACEMENT_3D ( 'NONE', #92965, #66061, #43872 ) ;
#124439 = EDGE_LOOP ( 'NONE', ( #87982, #44022 ) ) ;
#124440 = FACE_BOUND ( 'NONE', #6997, .T. ) ;
#124441 = PLANE ( 'NONE',  #116163 ) ;
#124442 = ORIENTED_EDGE ( 'NONE', *, *, #68950, .T. ) ;
#124443 = CARTESIAN_POINT ( 'NONE',  ( 12.49999999999993960, 12.50000000000000000, 4.265033745738159077 ) ) ;
#124444 = CARTESIAN_POINT ( 'NONE',  ( 1.849999999999948130, 2.500000000000000000, 6.048780366869520364 ) ) ;
#124445 = VECTOR ( 'NONE', #89286, 1000.000000000000000 ) ;
#124446 = AXIS2_PLACEMENT_3D ( 'NONE', #98883, #10495, #30165 ) ;
#124447 = ORIENTED_EDGE ( 'NONE', *, *, #48952, .F. ) ;
#124448 = ORIENTED_EDGE ( 'NONE', *, *, #120851, .F. ) ;
#124449 = CARTESIAN_POINT ( 'NONE',  ( 186.2552083336747444, 6.551208109652275624, -3.782341765624998686 ) ) ;
#124450 = CARTESIAN_POINT ( 'NONE',  ( 12.69999999999990159, 12.50000000000000000, -3.918623584224389056 ) ) ;
#124451 = CARTESIAN_POINT ( 'NONE',  ( 3.949999999999942446, 12.50000000000000000, -2.576566944158915184 ) ) ;
#124452 = CIRCLE ( 'NONE', #22065, 0.1000000000000002554 ) ;
#124453 = AXIS2_PLACEMENT_3D ( 'NONE', #77771, #89542, #129502 ) ;
#124454 = AXIS2_PLACEMENT_3D ( 'NONE', #45332, #84601, #83935 ) ;
#124455 = DIRECTION ( 'NONE',  ( 0.000000000000000000, 0.000000000000000000, 1.000000000000000000 ) ) ;
#124456 = DIRECTION ( 'NONE',  ( -0.000000000000000000, 1.000000000000000000, -0.000000000000000000 ) ) ;
#124457 = AXIS2_PLACEMENT_3D ( 'NONE', #32502, #72408, #33133 ) ;
#124458 = DIRECTION ( 'NONE',  ( 0.000000000000000000, 0.000000000000000000, -1.000000000000000000 ) ) ;
#124459 = FACE_OUTER_BOUND ( 'NONE', #115221, .T. ) ;
#124460 = CONICAL_SURFACE ( 'NONE', #11585, 0.09999999999999982514, 0.003490658503988666988 ) ;
#124461 = ORIENTED_EDGE ( 'NONE', *, *, #64475, .F. ) ;
#124464 = ORIENTED_EDGE ( 'NONE', *, *, #107376, .F. ) ;
#124463 = EDGE_CURVE ( 'NONE', #112979, #43211, #96310, .T. ) ;
#124462 = VECTOR ( 'NONE', #127243, 1000.000000000000000 ) ;
#124465 = DIRECTION ( 'NONE',  ( -0.000000000000000000, -1.000000000000000000, -0.000000000000000000 ) ) ;
#124466 = CARTESIAN_POINT ( 'NONE',  ( 187.2916666666666572, 4.445597072760113733, -7.700000000000009948 ) ) ;
#124467 = DIRECTION ( 'NONE',  ( -0.000000000000000000, 1.000000000000000000, -0.000000000000000000 ) ) ;
#124468 = AXIS2_PLACEMENT_3D ( 'NONE', #25519, #104100, #14413 ) ;
#124469 = DIRECTION ( 'NONE',  ( 0.000000000000000000, -0.000000000000000000, 1.000000000000000000 ) ) ;
#124471 = VERTEX_POINT ( 'NONE', #59918 ) ;
#124470 = VERTEX_POINT ( 'NONE', #38332 ) ;
#124472 = DIRECTION ( 'NONE',  ( 0.000000000000000000, 0.000000000000000000, 1.000000000000000000 ) ) ;
#124473 = VERTEX_POINT ( 'NONE', #39639 ) ;
#124474 = LINE ( 'NONE', #34824, #30421 ) ;
#124475 = CARTESIAN_POINT ( 'NONE',  ( 187.5000000000000000, 5.510910596163088569E-16, 4.000000000000000000 ) ) ;
#124476 = VERTEX_POINT ( 'NONE', #129304 ) ;
#124478 = EDGE_CURVE ( 'NONE', #117938, #107, #301, .T. ) ;
#124477 = DIRECTION ( 'NONE',  ( 0.000000000000000000, -0.000000000000000000, 1.000000000000000000 ) ) ;
#124479 = DIRECTION ( 'NONE',  ( 0.000000000000000000, -0.9999939076577903929, 0.003490651415223739937 ) ) ;
#124480 = CARTESIAN_POINT ( 'NONE',  ( 7.899999999999924860, 2.500000000000000000, -4.922947341949753586 ) ) ;
#124481 = DIRECTION ( 'NONE',  ( 0.000000000000000000, 0.000000000000000000, 1.000000000000000000 ) ) ;
#124482 = CARTESIAN_POINT ( 'NONE',  ( -10.00000000000000533, 12.50000000000000000, -5.022947341949749678 ) ) ;
#124483 = CARTESIAN_POINT ( 'NONE',  ( 10.84999999999990905, 2.500000000000000000, 2.265063509461097357 ) ) ;
#124484 = EDGE_CURVE ( 'NONE', #93441, #7770, #33636, .T. ) ;
#124485 = EDGE_CURVE ( 'NONE', #11640, #96489, #69712, .T. ) ;
#124486 = FACE_OUTER_BOUND ( 'NONE', #9904, .T. ) ;
#124487 = CARTESIAN_POINT ( 'NONE',  ( 14.19999999999989626, 2.500000000000000000, -2.276824562219559311E-15 ) ) ;
#124488 = ADVANCED_FACE ( 'NONE', ( #18020 ), #48795, .T. ) ;
#124489 = ADVANCED_FACE ( 'NONE', ( #100460 ), #10612, .T. ) ;
#124490 = VECTOR ( 'NONE', #32242, 1000.000000000000000 ) ;
#124491 = CARTESIAN_POINT ( 'NONE',  ( -3.300000000000027800, 12.50000000000000000, -2.276824562219559311E-15 ) ) ;
#124492 = ORIENTED_EDGE ( 'NONE', *, *, #21384, .T. ) ;
#124493 = ORIENTED_EDGE ( 'NONE', *, *, #26549, .F. ) ;
#124494 = VERTEX_POINT ( 'NONE', #68413 ) ;
#124495 = DIRECTION ( 'NONE',  ( 0.000000000000000000, 0.000000000000000000, -1.000000000000000000 ) ) ;
#124496 = VERTEX_POINT ( 'NONE', #78908 ) ;
#124497 = EDGE_CURVE ( 'NONE', #70390, #122264, #4349, .T. ) ;
#124498 = CARTESIAN_POINT ( 'NONE',  ( 9.149999999999920419, 2.500000000000000000, -7.188010851410854052 ) ) ;
#124501 = EDGE_LOOP ( 'NONE', ( #95761, #121588, #33754, #67832 ) ) ;
#124500 = ORIENTED_EDGE ( 'NONE', *, *, #17602, .T. ) ;
#124499 = EDGE_CURVE ( 'NONE', #35145, #18946, #104714, .T. ) ;
#124502 = AXIS2_PLACEMENT_3D ( 'NONE', #43348, #53789, #93722 ) ;
#124503 = ORIENTED_EDGE ( 'NONE', *, *, #103114, .T. ) ;
#124504 = EDGE_CURVE ( 'NONE', #127509, #104821, #37830, .T. ) ;
#124505 = CARTESIAN_POINT ( 'NONE',  ( 5.599999999999933031, 12.50000000000000000, 0.3464101615137735735 ) ) ;
#124506 = AXIS2_PLACEMENT_3D ( 'NONE', #29657, #127850, #97743 ) ;
#124507 = CONICAL_SURFACE ( 'NONE', #13665, 0.1000000000000000472, 0.003490658503988666988 ) ;
#124508 = EDGE_CURVE ( 'NONE', #102844, #11437, #52489, .T. ) ;
#124509 = EDGE_CURVE ( 'NONE', #32011, #26682, #115166, .T. ) ;
#124510 = DIRECTION ( 'NONE',  ( -0.000000000000000000, 1.000000000000000000, -0.000000000000000000 ) ) ;
#124511 = DIRECTION ( 'NONE',  ( 0.000000000000000000, 1.000000000000000000, 0.000000000000000000 ) ) ;
#124512 = LINE ( 'NONE', #56390, #112843 ) ;
#124513 = DIRECTION ( 'NONE',  ( -4.274815082592931898E-19, -0.9999939076577903929, -0.003490651415223739937 ) ) ;
#124514 = ORIENTED_EDGE ( 'NONE', *, *, #9392, .T. ) ;
#124515 = EDGE_CURVE ( 'NONE', #39039, #36386, #48145, .T. ) ;
#124516 = LINE ( 'NONE', #36129, #30918 ) ;
#124517 = ORIENTED_EDGE ( 'NONE', *, *, #51846, .F. ) ;
#124518 = VERTEX_POINT ( 'NONE', #88030 ) ;
#124519 = ORIENTED_EDGE ( 'NONE', *, *, #38638, .T. ) ;
#124520 = AXIS2_PLACEMENT_3D ( 'NONE', #48976, #117026, #19490 ) ;
#124521 = DIRECTION ( 'NONE',  ( 0.000000000000000000, -0.9999939076577903929, 0.003490651415223739937 ) ) ;
#124522 = ORIENTED_EDGE ( 'NONE', *, *, #45747, .F. ) ;
#124523 = ORIENTED_EDGE ( 'NONE', *, *, #105424, .F. ) ;
#124524 = VERTEX_POINT ( 'NONE', #127987 ) ;
#124525 =( NAMED_UNIT ( * ) PLANE_ANGLE_UNIT ( ) SI_UNIT ( $, .RADIAN. ) );
#124527 = VECTOR ( 'NONE', #52009, 1000.000000000000000 ) ;
#124526 = CARTESIAN_POINT ( 'NONE',  ( -12.89999999999999147, 2.500000000000000000, -5.122947341949751987 ) ) ;
#124528 = CARTESIAN_POINT ( 'NONE',  ( 10.39999999999991154, 12.50000000000000000, -3.572213422710612374 ) ) ;
#124529 = AXIS2_PLACEMENT_3D ( 'NONE', #49961, #116727, #17215 ) ;
#124530 = DIRECTION ( 'NONE',  ( 0.000000000000000000, 1.000000000000000000, 0.000000000000000000 ) ) ;
#124531 = DIRECTION ( 'NONE',  ( -0.000000000000000000, -1.000000000000000000, -0.000000000000000000 ) ) ;
#124532 = CARTESIAN_POINT ( 'NONE',  ( -10.65000000000000391, 12.50000000000000000, -1.753560074763284682 ) ) ;
#124533 = EDGE_LOOP ( 'NONE', ( #17697, #44662, #84730, #80981 ) ) ;
#124534 = DIRECTION ( 'NONE',  ( -4.274815082592931898E-19, -0.9999939076577903929, -0.003490651415223739937 ) ) ;
#124535 = ORIENTED_EDGE ( 'NONE', *, *, #64225, .F. ) ;
#124536 = CARTESIAN_POINT ( 'NONE',  ( -0.8500000000000382805, 12.50000000000000000, -1.537336459617587581 ) ) ;
#124537 = ORIENTED_EDGE ( 'NONE', *, *, #54147, .F. ) ;
#124538 = CARTESIAN_POINT ( 'NONE',  ( -9.400000000000007461, 2.500000000000000000, 4.083716857408420609 ) ) ;
#124539 = VERTEX_POINT ( 'NONE', #29161 ) ;
#124540 = EDGE_LOOP ( 'NONE', ( #126632, #106544, #16552, #126501 ) ) ;
#124541 = DIRECTION ( 'NONE',  ( 0.000000000000000000, 1.000000000000000000, 0.000000000000000000 ) ) ;
#124542 = DIRECTION ( 'NONE',  ( -0.000000000000000000, -1.000000000000000000, -0.000000000000000000 ) ) ;
#124543 = EDGE_CURVE ( 'NONE', #122392, #94085, #6489, .T. ) ;
#124544 = AXIS2_PLACEMENT_3D ( 'NONE', #57171, #127847, #125276 ) ;
#124546 = DIRECTION ( 'NONE',  ( 0.000000000000000000, 0.000000000000000000, -1.000000000000000000 ) ) ;
#124545 = AXIS2_PLACEMENT_3D ( 'NONE', #15204, #14573, #25053 ) ;
#124547 = ADVANCED_FACE ( 'NONE', ( #99180 ), #49449, .T. ) ;
#124548 = ORIENTED_EDGE ( 'NONE', *, *, #94666, .F. ) ;
#124549 = DIRECTION ( 'NONE',  ( -0.000000000000000000, -1.000000000000000000, -0.000000000000000000 ) ) ;
#124550 = EDGE_LOOP ( 'NONE', ( #96555, #73309, #7709, #95129 ) ) ;
#124551 = CARTESIAN_POINT ( 'NONE',  ( 1.449999999999951772, 12.50000000000000000, -6.148780366869526226 ) ) ;
#124552 = DIRECTION ( 'NONE',  ( 1.000000000000000000, 0.000000000000000000, 0.000000000000000000 ) ) ;
#124553 = CARTESIAN_POINT ( 'NONE',  ( 8.949999999999919353, 12.50000000000000000, -6.148780366869526226 ) ) ;
#124554 = CARTESIAN_POINT ( 'NONE',  ( -11.64999999999999858, 12.50000000000000000, -1.472243186433546125 ) ) ;
#124555 = ADVANCED_FACE ( 'NONE', ( #42190 ), #19034, .T. ) ;
#124556 = CARTESIAN_POINT ( 'NONE',  ( 7.499999999999961808, 12.50000000000000000, -4.265033745738164406 ) ) ;
#124557 = EDGE_LOOP ( 'NONE', ( #83218, #120019 ) ) ;
#124558 = VERTEX_POINT ( 'NONE', #101755 ) ;
#124559 = AXIS2_PLACEMENT_3D ( 'NONE', #20572, #18628, #78864 ) ;
#124560 = EDGE_LOOP ( 'NONE', ( #109489, #41462 ) ) ;
#124561 = CONICAL_SURFACE ( 'NONE', #116135, 0.09999999999999982514, 0.003490658503988666988 ) ;
#124562 = LINE ( 'NONE', #83352, #113391 ) ;
#124564 = CIRCLE ( 'NONE', #11391, 0.1000000000000000056 ) ;
#124563 = CARTESIAN_POINT ( 'NONE',  ( 8.749999999999957367, 2.500000000000000000, -6.495190528383302464 ) ) ;
#124565 = AXIS2_PLACEMENT_3D ( 'NONE', #118532, #78641, #20984 ) ;
#124566 = AXIS2_PLACEMENT_3D ( 'NONE', #117760, #56278, #78531 ) ;
#124567 = CARTESIAN_POINT ( 'NONE',  ( 184.9635416670080872, -4.367472073101519747, 7.564683531249999149 ) ) ;
#124568 = DIRECTION ( 'NONE',  ( 0.000000000000000000, 1.000000000000000000, 0.000000000000000000 ) ) ;
#124569 = CARTESIAN_POINT ( 'NONE',  ( 1.699999999999951994, 2.500000000000000000, -4.330127018922201643 ) ) ;
#124570 = FACE_OUTER_BOUND ( 'NONE', #118913, .T. ) ;
#124571 = DIRECTION ( 'NONE',  ( 0.000000000000000000, 0.000000000000000000, 1.000000000000000000 ) ) ;
#124572 = ORIENTED_EDGE ( 'NONE', *, *, #40530, .F. ) ;
#124573 = DIRECTION ( 'NONE',  ( -0.000000000000000000, 1.000000000000000000, -0.000000000000000000 ) ) ;
#124574 = DIRECTION ( 'NONE',  ( 0.000000000000000000, 1.000000000000000000, 0.000000000000000000 ) ) ;
#124575 = EDGE_LOOP ( 'NONE', ( #64324, #93353 ) ) ;
#124576 = AXIS2_PLACEMENT_3D ( 'NONE', #99528, #9842, #90314 ) ;
#124577 = CARTESIAN_POINT ( 'NONE',  ( -7.500000000000013323, 2.500000000000000000, 5.022947341949748790 ) ) ;
#124578 = EDGE_CURVE ( 'NONE', #57241, #15129, #44090, .T. ) ;
#124579 = ORIENTED_EDGE ( 'NONE', *, *, #100698, .F. ) ;
#124580 = PRODUCT_DEFINITION_SHAPE ( 'NONE', 'NONE',  #129621 ) ;
#124581 = DIRECTION ( 'NONE',  ( 0.000000000000000000, -0.9999939076577903929, 0.003490651415223739937 ) ) ;
#124582 = CONICAL_SURFACE ( 'NONE', #68133, 0.1000000000000002554, 0.003490658503988666988 ) ;
#124583 = EDGE_LOOP ( 'NONE', ( #8558, #102492, #78522, #24406 ) ) ;
#124584 = DIRECTION ( 'NONE',  ( 0.000000000000000000, -0.000000000000000000, 1.000000000000000000 ) ) ;
#124585 = LINE ( 'NONE', #23811, #38357 ) ;
#124586 = CARTESIAN_POINT ( 'NONE',  ( 5.799999999999931433, 2.500000000000000000, 4.230127018922196669 ) ) ;
#124587 = AXIS2_PLACEMENT_3D ( 'NONE', #46057, #95790, #116068 ) ;
#124588 = AXIS2_PLACEMENT_3D ( 'NONE', #6105, #45415, #46059 ) ;
#124589 = ORIENTED_EDGE ( 'NONE', *, *, #58409, .T. ) ;
#124590 = CARTESIAN_POINT ( 'NONE',  ( 4.399999999999937295, 12.50000000000000000, 3.983716857408420964 ) ) ;
#124591 = VECTOR ( 'NONE', #22236, 1000.000000000000000 ) ;
#124592 = FACE_OUTER_BOUND ( 'NONE', #23523, .T. ) ;
#124593 = EDGE_CURVE ( 'NONE', #120092, #82094, #77532, .T. ) ;
#124594 = EDGE_CURVE ( 'NONE', #113477, #101366, #69209, .T. ) ;
#124595 = ORIENTED_EDGE ( 'NONE', *, *, #61524, .F. ) ;
#124597 = VECTOR ( 'NONE', #79672, 1000.000000000000000 ) ;
#124596 = DIRECTION ( 'NONE',  ( -4.274815082592931898E-19, -0.9999939076577903929, -0.003490651415223739937 ) ) ;
#124598 = VERTEX_POINT ( 'NONE', #122675 ) ;
#124600 = CONICAL_SURFACE ( 'NONE', #68154, 0.09999999999999982514, 0.003490658503988666988 ) ;
#124599 = VECTOR ( 'NONE', #73943, 1000.000000000000000 ) ;
#124601 = ORIENTED_EDGE ( 'NONE', *, *, #41057, .F. ) ;
#124602 = DIRECTION ( 'NONE',  ( 0.000000000000000000, 1.000000000000000000, 0.000000000000000000 ) ) ;
#124603 = CARTESIAN_POINT ( 'NONE',  ( 10.64999999999990976, 2.500000000000000000, 1.818653347947321475 ) ) ;
#124604 = ADVANCED_FACE ( 'NONE', ( #1603 ), #54536, .T. ) ;
#124605 = ORIENTED_EDGE ( 'NONE', *, *, #20621, .F. ) ;
#124606 = DIRECTION ( 'NONE',  ( 0.000000000000000000, -0.000000000000000000, 1.000000000000000000 ) ) ;
#124607 = CARTESIAN_POINT ( 'NONE',  ( -13.94999999999998685, 2.500000000000000000, 1.918653347947325338 ) ) ;
#124608 = VERTEX_POINT ( 'NONE', #83411 ) ;
#124609 = CARTESIAN_POINT ( 'NONE',  ( -6.650000000000018119, 2.500000000000000000, -6.495190528383302464 ) ) ;
#124610 = DIRECTION ( 'NONE',  ( 0.000000000000000000, 0.000000000000000000, -1.000000000000000000 ) ) ;
#124611 = DIRECTION ( 'NONE',  ( 0.000000000000000000, 0.000000000000000000, 1.000000000000000000 ) ) ;
#124612 = CARTESIAN_POINT ( 'NONE',  ( -11.05000000000000249, 2.500000000000000000, -1.818653347947322141 ) ) ;
#124613 = FACE_OUTER_BOUND ( 'NONE', #87756, .T. ) ;
#124614 = FACE_OUTER_BOUND ( 'NONE', #40186, .T. ) ;
#124615 = DIRECTION ( 'NONE',  ( -0.000000000000000000, 1.000000000000000000, -0.000000000000000000 ) ) ;
#124616 = ORIENTED_EDGE ( 'NONE', *, *, #129357, .F. ) ;
#124617 = ORIENTED_EDGE ( 'NONE', *, *, #37917, .F. ) ;
#124618 = EDGE_LOOP ( 'NONE', ( #90909, #57480, #52887, #98425 ) ) ;
#124619 = ORIENTED_EDGE ( 'NONE', *, *, #13107, .T. ) ;
#124620 = CARTESIAN_POINT ( 'NONE',  ( -8.550000000000009592, 2.500000000000000000, 6.941600689897073018 ) ) ;
#124621 = DIRECTION ( 'NONE',  ( 0.000000000000000000, 0.000000000000000000, 1.000000000000000000 ) ) ;
#124622 = FACE_OUTER_BOUND ( 'NONE', #33971, .T. ) ;
#124623 = ORIENTED_EDGE ( 'NONE', *, *, #95409, .T. ) ;
#124624 = FACE_BOUND ( 'NONE', #127748, .T. ) ;
#124625 = DIRECTION ( 'NONE',  ( 0.000000000000000000, -0.9999939076577903929, 0.003490651415223739937 ) ) ;
#124626 = CARTESIAN_POINT ( 'NONE',  ( 12.89999999999990088, 12.50000000000000000, -4.330127018922201643 ) ) ;
#124628 = EDGE_CURVE ( 'NONE', #56748, #90263, #27343, .T. ) ;
#124627 = FACE_OUTER_BOUND ( 'NONE', #88982, .T. ) ;
#124629 = AXIS2_PLACEMENT_3D ( 'NONE', #64264, #33539, #125130 ) ;
#124630 = DIRECTION ( 'NONE',  ( 0.000000000000000000, -0.000000000000000000, 1.000000000000000000 ) ) ;
#124631 = CONICAL_SURFACE ( 'NONE', #43091, 0.1000000000000000056, 0.003490658503988666988 ) ;
#124632 = CARTESIAN_POINT ( 'NONE',  ( 10.44999999999991402, 2.500000000000000000, -2.065063509461102065 ) ) ;
#124633 = DIRECTION ( 'NONE',  ( 0.000000000000000000, -0.9999939076577903929, 0.003490651415223739937 ) ) ;
#124634 = DIRECTION ( 'NONE',  ( 0.000000000000000000, -0.000000000000000000, 1.000000000000000000 ) ) ;
#124635 = PLANE ( 'NONE',  #45086 ) ;
#124636 = EDGE_CURVE ( 'NONE', #14824, #62384, #16952, .T. ) ;
#124637 = DIRECTION ( 'NONE',  ( 0.000000000000000000, 0.000000000000000000, 1.000000000000000000 ) ) ;
#124638 = ADVANCED_FACE ( 'NONE', ( #91283 ), #84026, .T. ) ;
#124639 = EDGE_CURVE ( 'NONE', #72184, #60686, #110910, .T. ) ;
#124640 = FACE_OUTER_BOUND ( 'NONE', #120117, .T. ) ;
#124642 = CIRCLE ( 'NONE', #15948, 0.1000000000000002554 ) ;
#124641 = CONICAL_SURFACE ( 'NONE', #45223, 0.1000000000000002554, 0.003490658503988666988 ) ;
#124643 = ORIENTED_EDGE ( 'NONE', *, *, #82395, .F. ) ;
#124644 = ORIENTED_EDGE ( 'NONE', *, *, #101931, .F. ) ;
#124645 = ORIENTED_EDGE ( 'NONE', *, *, #44060, .T. ) ;
#124646 = VERTEX_POINT ( 'NONE', #93228 ) ;
#124647 = CARTESIAN_POINT ( 'NONE',  ( 11.04999999999991189, 2.500000000000000000, 6.248780366869521430 ) ) ;
#124648 = EDGE_CURVE ( 'NONE', #95927, #32380, #92198, .T. ) ;
#124649 = ORIENTED_EDGE ( 'NONE', *, *, #94508, .F. ) ;
#124651 = EDGE_CURVE ( 'NONE', #92128, #52089, #58765, .T. ) ;
#124650 = FACE_OUTER_BOUND ( 'NONE', #35093, .T. ) ;
#124653 = EDGE_LOOP ( 'NONE', ( #55238, #19130 ) ) ;
#124652 = EDGE_CURVE ( 'NONE', #110742, #33188, #33032, .T. ) ;
#124654 = ORIENTED_EDGE ( 'NONE', *, *, #119489, .F. ) ;
#124656 = AXIS2_PLACEMENT_3D ( 'NONE', #10586, #81918, #40742 ) ;
#124655 = CIRCLE ( 'NONE', #101670, 0.06509327318403745899 ) ;
#124657 = AXIS2_PLACEMENT_3D ( 'NONE', #65411, #124986, #6460 ) ;
#124658 = EDGE_CURVE ( 'NONE', #39091, #115638, #72934, .T. ) ;
#124659 = CARTESIAN_POINT ( 'NONE',  ( 10.64999999999991331, 2.500000000000000000, -1.918653347947325782 ) ) ;
#124660 = CARTESIAN_POINT ( 'NONE',  ( -8.150000000000012790, 2.500000000000000000, 1.818653347947321475 ) ) ;
#124661 = FACE_OUTER_BOUND ( 'NONE', #51648, .T. ) ;
#124662 = DIRECTION ( 'NONE',  ( 0.000000000000000000, 0.000000000000000000, 1.000000000000000000 ) ) ;
#124663 = EDGE_CURVE ( 'NONE', #121393, #123488, #14814, .T. ) ;
#124664 = ORIENTED_EDGE ( 'NONE', *, *, #28810, .T. ) ;
#124665 = ADVANCED_FACE ( 'NONE', ( #112220 ), #121446, .T. ) ;
#124666 = VERTEX_POINT ( 'NONE', #103029 ) ;
#124667 = ORIENTED_EDGE ( 'NONE', *, *, #116547, .F. ) ;
#124669 = ORIENTED_EDGE ( 'NONE', *, *, #118706, .T. ) ;
#124668 = DIRECTION ( 'NONE',  ( -0.000000000000000000, 1.000000000000000000, -0.000000000000000000 ) ) ;
#124670 = CARTESIAN_POINT ( 'NONE',  ( 21.34481565588170326, -0.7053969147713214927, -2.184679923000713231 ) ) ;
#124671 = ORIENTED_EDGE ( 'NONE', *, *, #76465, .T. ) ;
#124672 = CIRCLE ( 'NONE', #68216, 0.09999999999999982514 ) ;
#124673 = ORIENTED_EDGE ( 'NONE', *, *, #48864, .F. ) ;
#124674 = CARTESIAN_POINT ( 'NONE',  ( -6.850000000000013856, 2.500000000000000000, 1.818653347947321475 ) ) ;
#124675 = FACE_OUTER_BOUND ( 'NONE', #69923, .T. ) ;
#124677 = AXIS2_PLACEMENT_3D ( 'NONE', #48121, #127957, #99156 ) ;
#124676 = DIRECTION ( 'NONE',  ( 0.000000000000000000, 0.000000000000000000, 1.000000000000000000 ) ) ;
#124678 = AXIS2_PLACEMENT_3D ( 'NONE', #18593, #107620, #87318 ) ;
#124679 = DIRECTION ( 'NONE',  ( 0.000000000000000000, 0.000000000000000000, -1.000000000000000000 ) ) ;
#124680 = CARTESIAN_POINT ( 'NONE',  ( -7.950000000000009059, 2.500000000000000000, 6.395190528383296602 ) ) ;
#124681 = AXIS2_PLACEMENT_3D ( 'NONE', #106598, #26759, #37860 ) ;
#124682 = CIRCLE ( 'NONE', #97566, 0.06509327318403745899 ) ;
#124683 = ORIENTED_EDGE ( 'NONE', *, *, #86694, .T. ) ;
#124684 = DIRECTION ( 'NONE',  ( -0.000000000000000000, 1.000000000000000000, -0.000000000000000000 ) ) ;
#124685 = ORIENTED_EDGE ( 'NONE', *, *, #17978, .T. ) ;
#124686 = AXIS2_PLACEMENT_3D ( 'NONE', #116664, #17813, #18468 ) ;
#124687 = CARTESIAN_POINT ( 'NONE',  ( 6.849999999999930367, 12.50000000000000000, -6.213873640053564351 ) ) ;
#124688 = ORIENTED_EDGE ( 'NONE', *, *, #92897, .F. ) ;
#124689 = CARTESIAN_POINT ( 'NONE',  ( 11.64999999999990266, 2.500000000000000000, 2.165063509461097713 ) ) ;
#124690 = CARTESIAN_POINT ( 'NONE',  ( 10.39999999999990976, 2.500000000000000000, -4.330127018922201643 ) ) ;
#124691 = CARTESIAN_POINT ( 'NONE',  ( -7.499999999999980460, 2.500000000000000000, -2.276824562219559311E-15 ) ) ;
#124692 = DIRECTION ( 'NONE',  ( 0.000000000000000000, 0.000000000000000000, -1.000000000000000000 ) ) ;
#124693 = ORIENTED_EDGE ( 'NONE', *, *, #15711, .F. ) ;
#124694 = AXIS2_PLACEMENT_3D ( 'NONE', #41065, #104929, #104307 ) ;
#124695 = ADVANCED_FACE ( 'NONE', ( #52639 ), #92575, .T. ) ;
#124696 = AXIS2_PLACEMENT_3D ( 'NONE', #31309, #13565, #71204 ) ;
#124697 = DIRECTION ( 'NONE',  ( 0.000000000000000000, 0.000000000000000000, 1.000000000000000000 ) ) ;
#124698 = EDGE_CURVE ( 'NONE', #9617, #106262, #62959, .T. ) ;
#124699 = VERTEX_POINT ( 'NONE', #106887 ) ;
#124700 = VERTEX_POINT ( 'NONE', #6106 ) ;
#124701 = EDGE_LOOP ( 'NONE', ( #114299, #107814 ) ) ;
#124702 = DIRECTION ( 'NONE',  ( -0.000000000000000000, -1.000000000000000000, -0.000000000000000000 ) ) ;
#124703 = DIRECTION ( 'NONE',  ( -0.000000000000000000, 1.000000000000000000, -0.000000000000000000 ) ) ;
#124704 = CARTESIAN_POINT ( 'NONE',  ( 184.3593750003413732, 0.000000000000000000, 7.564683531250000925 ) ) ;
#124705 = DIRECTION ( 'NONE',  ( -0.000000000000000000, -1.000000000000000000, -0.000000000000000000 ) ) ;
#124706 = DIRECTION ( 'NONE',  ( -0.000000000000000000, -1.000000000000000000, -0.000000000000000000 ) ) ;
#124707 = LINE ( 'NONE', #46139, #98855 ) ;
#124708 = ORIENTED_EDGE ( 'NONE', *, *, #95400, .T. ) ;
#124709 = CARTESIAN_POINT ( 'NONE',  ( -12.29999999999999538, 2.500000000000000000, -4.676537180435976104 ) ) ;
#124710 = ORIENTED_EDGE ( 'NONE', *, *, #39050, .F. ) ;
#124711 = DIRECTION ( 'NONE',  ( 0.000000000000000000, 0.000000000000000000, -1.000000000000000000 ) ) ;
#124712 = LINE ( 'NONE', #64498, #75613 ) ;
#124713 = LINE ( 'NONE', #104425, #46006 ) ;
#124714 = EDGE_LOOP ( 'NONE', ( #129425, #4854, #15021, #2332 ) ) ;
#124715 = CIRCLE ( 'NONE', #68271, 0.1000000000000000056 ) ;
#124716 = CIRCLE ( 'NONE', #105844, 0.1000000000000002554 ) ;
#124717 = DIRECTION ( 'NONE',  ( -0.000000000000000000, -1.000000000000000000, -0.000000000000000000 ) ) ;
#124718 = DIRECTION ( 'NONE',  ( 0.000000000000000000, 0.000000000000000000, -1.000000000000000000 ) ) ;
#124719 = ORIENTED_EDGE ( 'NONE', *, *, #57897, .F. ) ;
#124721 = AXIS2_PLACEMENT_3D ( 'NONE', #36404, #8668, #39477 ) ;
#124720 = CIRCLE ( 'NONE', #47368, 0.06509327318403745899 ) ;
#124722 = DIRECTION ( 'NONE',  ( 0.000000000000000000, 0.000000000000000000, 1.000000000000000000 ) ) ;
#124723 = EDGE_CURVE ( 'NONE', #21305, #46048, #56502, .T. ) ;
#124724 = ORIENTED_EDGE ( 'NONE', *, *, #127470, .F. ) ;
#124725 = EDGE_LOOP ( 'NONE', ( #32273, #128729 ) ) ;
#124726 = DIRECTION ( 'NONE',  ( 0.000000000000000000, 0.000000000000000000, -1.000000000000000000 ) ) ;
#124727 = EDGE_LOOP ( 'NONE', ( #28959, #38448, #110541, #7657, #27741, #123100, #36931, #115364, #104668, #7427, #117444, #80057, #128536 ) ) ;
#124728 = CARTESIAN_POINT ( 'NONE',  ( 18.27284318114930883, 0.4998542452743989783, -4.791717918552158118 ) ) ;
#124729 = DIRECTION ( 'NONE',  ( -0.000000000000000000, 1.000000000000000000, -0.000000000000000000 ) ) ;
#124731 = VECTOR ( 'NONE', #45235, 1000.000000000000000 ) ;
#124730 = CIRCLE ( 'NONE', #66236, 0.06509327318403745899 ) ;
#124732 = CARTESIAN_POINT ( 'NONE',  ( -11.84999999999999609, 2.500000000000000000, 6.941600689897073018 ) ) ;
#124733 = EDGE_CURVE ( 'NONE', #56716, #69025, #98452, .T. ) ;
#124734 = ORIENTED_EDGE ( 'NONE', *, *, #36983, .F. ) ;
#124735 = CIRCLE ( 'NONE', #53634, 0.1000000000000002554 ) ;
#124736 = FACE_BOUND ( 'NONE', #10558, .T. ) ;
#124737 = CARTESIAN_POINT ( 'NONE',  ( -6.071532165918824830E-15, 12.50000000000000000, -4.330127018922201643 ) ) ;
#124739 = ORIENTED_EDGE ( 'NONE', *, *, #119584, .T. ) ;
#124738 = DIRECTION ( 'NONE',  ( 0.000000000000000000, 0.000000000000000000, -1.000000000000000000 ) ) ;
#124740 = EDGE_CURVE ( 'NONE', #30745, #70927, #113133, .T. ) ;
#124741 = CARTESIAN_POINT ( 'NONE',  ( -11.24999999999996447, 12.50000000000000000, -6.495190528383298911 ) ) ;
#124742 = DIRECTION ( 'NONE',  ( -0.000000000000000000, 1.000000000000000000, -0.000000000000000000 ) ) ;
#124743 = ADVANCED_FACE ( 'NONE', ( #66955 ), #90129, .T. ) ;
#124744 = ORIENTED_EDGE ( 'NONE', *, *, #94762, .F. ) ;
#124745 = ORIENTED_EDGE ( 'NONE', *, *, #55792, .T. ) ;
#124746 = ADVANCED_FACE ( 'NONE', ( #76160 ), #106859, .T. ) ;
#124747 = ORIENTED_EDGE ( 'NONE', *, *, #44060, .F. ) ;
#124748 = CARTESIAN_POINT ( 'NONE',  ( -3.550000000000028244, 2.500000000000000000, 2.611473670974873151 ) ) ;
#124749 = DIRECTION ( 'NONE',  ( -0.000000000000000000, 1.000000000000000000, -0.000000000000000000 ) ) ;
#124750 = CARTESIAN_POINT ( 'NONE',  ( 7.099999999999928590, 2.500000000000000000, 3.637306695894644726 ) ) ;
#124751 = EDGE_CURVE ( 'NONE', #62839, #101653, #33720, .T. ) ;
#124752 = FACE_BOUND ( 'NONE', #2748, .T. ) ;
#124753 = VERTEX_POINT ( 'NONE', #35596 ) ;
#124754 = AXIS2_PLACEMENT_3D ( 'NONE', #109680, #20014, #49486 ) ;
#124755 = CARTESIAN_POINT ( 'NONE',  ( 185.2343750003414016, 8.734944146203032389, 5.348610694689227483E-16 ) ) ;
#124756 = CONICAL_SURFACE ( 'NONE', #68316, 0.09999999999999982514, 0.003490658503988666988 ) ;
#124757 = CARTESIAN_POINT ( 'NONE',  ( -0.4500000000000397571, 2.500000000000000000, -6.595190528383302109 ) ) ;
#124758 = CARTESIAN_POINT ( 'NONE',  ( -11.64999999999999680, 2.500000000000000000, 2.165063509461097713 ) ) ;
#124759 = CARTESIAN_POINT ( 'NONE',  ( -11.05000000000000071, 2.500000000000000000, 2.511473670974873507 ) ) ;
#124760 = AXIS2_PLACEMENT_3D ( 'NONE', #68234, #67581, #97059 ) ;
#124761 = CARTESIAN_POINT ( 'NONE',  ( -1.450000000000035927, 2.500000000000000000, -1.818653347947326138 ) ) ;
#124762 = PLANE ( 'NONE',  #8905 ) ;
#124763 = DIRECTION ( 'NONE',  ( -0.000000000000000000, 1.000000000000000000, -0.000000000000000000 ) ) ;
#124764 = VECTOR ( 'NONE', #62654, 1000.000000000000000 ) ;
#124765 = CARTESIAN_POINT ( 'NONE',  ( 7.699999999999923794, 2.500000000000000000, -3.983716857408426293 ) ) ;
#124766 = CIRCLE ( 'NONE', #7673, 0.1000000000000002554 ) ;
#124767 = CARTESIAN_POINT ( 'NONE',  ( -10.00000000000000355, 2.500000000000000000, -0.5928203230275541635 ) ) ;
#124768 = AXIS2_PLACEMENT_3D ( 'NONE', #113943, #34098, #72731 ) ;
#124769 = EDGE_LOOP ( 'NONE', ( #70907, #57895 ) ) ;
#124770 = ORIENTED_EDGE ( 'NONE', *, *, #75697, .F. ) ;
#124771 = EDGE_LOOP ( 'NONE', ( #55348, #20749 ) ) ;
#124772 = ORIENTED_EDGE ( 'NONE', *, *, #123572, .T. ) ;
#124773 = ORIENTED_EDGE ( 'NONE', *, *, #114163, .F. ) ;
#124774 = DIRECTION ( 'NONE',  ( 0.000000000000000000, 0.000000000000000000, -1.000000000000000000 ) ) ;
#124775 = DIRECTION ( 'NONE',  ( -4.274815082592931898E-19, -0.9999939076577903929, -0.003490651415223739937 ) ) ;
#124776 = AXIS2_PLACEMENT_3D ( 'NONE', #112589, #21623, #92279 ) ;
#124777 = ORIENTED_EDGE ( 'NONE', *, *, #61415, .F. ) ;
#124778 = FACE_BOUND ( 'NONE', #36523, .T. ) ;
#124780 = CARTESIAN_POINT ( 'NONE',  ( 1.049999999999954525, 12.50000000000000000, 1.883746621131358934 ) ) ;
#124779 = VECTOR ( 'NONE', #89177, 1000.000000000000000 ) ;
#124781 = ADVANCED_FACE ( 'NONE', ( #86608 ), #86019, .T. ) ;
#124783 = CIRCLE ( 'NONE', #22391, 0.1000000000000000472 ) ;
#124782 = AXIS2_PLACEMENT_3D ( 'NONE', #95368, #67153, #106465 ) ;
#124784 = LINE ( 'NONE', #75662, #36519 ) ;
#124785 = ORIENTED_EDGE ( 'NONE', *, *, #124651, .F. ) ;
#124786 = LINE ( 'NONE', #42364, #47412 ) ;
#124787 = CARTESIAN_POINT ( 'NONE',  ( 186.8750000000000000, 8.891194145520236347, 5.444286225454521982E-16 ) ) ;
#124788 = EDGE_CURVE ( 'NONE', #27686, #118657, #344, .T. ) ;
#124789 = DIRECTION ( 'NONE',  ( 0.000000000000000000, -0.000000000000000000, 1.000000000000000000 ) ) ;
#124790 = ORIENTED_EDGE ( 'NONE', *, *, #124002, .T. ) ;
#124791 = FACE_OUTER_BOUND ( 'NONE', #84488, .T. ) ;
#124792 = EDGE_CURVE ( 'NONE', #6072, #50160, #117302, .T. ) ;
#124793 = ORIENTED_EDGE ( 'NONE', *, *, #86183, .T. ) ;
#124794 = ORIENTED_EDGE ( 'NONE', *, *, #118587, .F. ) ;
#124795 = EDGE_LOOP ( 'NONE', ( #49335, #52145, #115191, #17086 ) ) ;
#124796 = EDGE_CURVE ( 'NONE', #115621, #41467, #94343, .T. ) ;
#124797 = PLANE ( 'NONE',  #2786 ) ;
#124799 = EDGE_CURVE ( 'NONE', #125318, #46605, #81827, .T. ) ;
#124798 = DIRECTION ( 'NONE',  ( -4.274815082592931898E-19, -0.9999939076577903929, -0.003490651415223739937 ) ) ;
#124800 = FACE_OUTER_BOUND ( 'NONE', #45142, .T. ) ;
#124802 = ORIENTED_EDGE ( 'NONE', *, *, #77336, .T. ) ;
#124801 = ADVANCED_FACE ( 'NONE', ( #66325 ), #54635, .T. ) ;
#124803 = CIRCLE ( 'NONE', #76684, 0.06509327318403745899 ) ;
#124804 = CARTESIAN_POINT ( 'NONE',  ( 4.912722231824622199, 1.499999999999620082, -9.942384337864433874 ) ) ;
#124805 = EDGE_CURVE ( 'NONE', #126729, #69733, #54563, .T. ) ;
#124806 = CARTESIAN_POINT ( 'NONE',  ( -8.150000000000009237, 2.500000000000000000, 6.248780366869520542 ) ) ;
#124808 = EDGE_CURVE ( 'NONE', #54095, #8279, #41030, .T. ) ;
#124807 = CARTESIAN_POINT ( 'NONE',  ( -7.300000000000013145, 2.500000000000000000, 4.083716857408420609 ) ) ;
#124809 = CARTESIAN_POINT ( 'NONE',  ( 184.1562500006828316, 8.891194145520236347, 5.444286225454521982E-16 ) ) ;
#124810 = DIRECTION ( 'NONE',  ( 1.000000000000000000, -0.000000000000000000, -0.000000000000000000 ) ) ;
#124811 = DIRECTION ( 'NONE',  ( 0.000000000000000000, -0.000000000000000000, 1.000000000000000000 ) ) ;
#124812 = ORIENTED_EDGE ( 'NONE', *, *, #16190, .T. ) ;
#124813 = DIRECTION ( 'NONE',  ( 0.000000000000000000, 0.000000000000000000, -1.000000000000000000 ) ) ;
#124814 = EDGE_CURVE ( 'NONE', #49458, #96815, #29602, .T. ) ;
#124815 = EDGE_CURVE ( 'NONE', #10654, #57940, #19116, .T. ) ;
#124816 = AXIS2_PLACEMENT_3D ( 'NONE', #81663, #11637, #19520 ) ;
#124817 = ORIENTED_EDGE ( 'NONE', *, *, #125113, .F. ) ;
#124818 = AXIS2_PLACEMENT_3D ( 'NONE', #30071, #89619, #69987 ) ;
#124819 = VERTEX_POINT ( 'NONE', #95154 ) ;
#124820 = FACE_OUTER_BOUND ( 'NONE', #120379, .T. ) ;
#124821 = DIRECTION ( 'NONE',  ( 1.000000000000000000, 0.000000000000000000, 0.000000000000000000 ) ) ;
#124822 = FACE_OUTER_BOUND ( 'NONE', #116877, .T. ) ;
#124823 = CARTESIAN_POINT ( 'NONE',  ( 10.64999999999990976, 2.500000000000000000, 1.918653347947321564 ) ) ;
#124824 = CARTESIAN_POINT ( 'NONE',  ( 184.4999999999999432, -5.532705916124244894, -5.308109601923121090 ) ) ;
#124825 = ORIENTED_EDGE ( 'NONE', *, *, #33906, .F. ) ;
#124827 = ORIENTED_EDGE ( 'NONE', *, *, #55054, .F. ) ;
#124826 = AXIS2_PLACEMENT_3D ( 'NONE', #11039, #19589, #69983 ) ;
#124828 = LINE ( 'NONE', #3755, #20411 ) ;
#124829 = DIRECTION ( 'NONE',  ( 0.000000000000000000, 0.000000000000000000, -1.000000000000000000 ) ) ;
#124830 = CARTESIAN_POINT ( 'NONE',  ( -11.24999999999996447, 2.500000000000000000, -2.165063509461097713 ) ) ;
#124831 = ORIENTED_EDGE ( 'NONE', *, *, #78851, .F. ) ;
#124832 = ORIENTED_EDGE ( 'NONE', *, *, #12389, .F. ) ;
#124833 = CARTESIAN_POINT ( 'NONE',  ( 8.949999999999917577, 2.500000000000000000, -2.511473670974877948 ) ) ;
#124834 = AXIS2_PLACEMENT_3D ( 'NONE', #29889, #54993, #58706 ) ;
#124835 = ORIENTED_EDGE ( 'NONE', *, *, #42959, .T. ) ;
#124836 = CARTESIAN_POINT ( 'NONE',  ( -8.950000000000009948, 12.50000000000000000, -6.906693963081109722 ) ) ;
#124837 = VECTOR ( 'NONE', #53314, 1000.000000000000000 ) ;
#124838 = DIRECTION ( 'NONE',  ( -0.000000000000000000, -1.000000000000000000, -0.000000000000000000 ) ) ;
#124839 = VERTEX_POINT ( 'NONE', #76804 ) ;
#124840 = DIRECTION ( 'NONE',  ( -4.274815082592931898E-19, -0.9999939076577903929, -0.003490651415223739937 ) ) ;
#124841 = FACE_OUTER_BOUND ( 'NONE', #89338, .T. ) ;
#124842 = DIRECTION ( 'NONE',  ( 0.000000000000000000, 1.000000000000000000, 0.000000000000000000 ) ) ;
#124843 = DIRECTION ( 'NONE',  ( -0.000000000000000000, 1.000000000000000000, -0.000000000000000000 ) ) ;
#124844 = ORIENTED_EDGE ( 'NONE', *, *, #89676, .F. ) ;
#124845 = CARTESIAN_POINT ( 'NONE',  ( 1.649999999999951061, 2.500000000000000000, -6.495190528383302464 ) ) ;
#124846 = EDGE_CURVE ( 'NONE', #41921, #64447, #113220, .T. ) ;
#124847 = CARTESIAN_POINT ( 'NONE',  ( 179.5000000000000000, 0.000000000000000000, -6.000000000000000000 ) ) ;
#124848 = ORIENTED_EDGE ( 'NONE', *, *, #117971, .T. ) ;
#124849 = ORIENTED_EDGE ( 'NONE', *, *, #50894, .T. ) ;
#124850 = DIRECTION ( 'NONE',  ( 0.000000000000000000, -0.9999939076577903929, 0.003490651415223739937 ) ) ;
#124851 = FACE_OUTER_BOUND ( 'NONE', #50745, .T. ) ;
#124852 = DIRECTION ( 'NONE',  ( 0.000000000000000000, 0.000000000000000000, 1.000000000000000000 ) ) ;
#124853 = AXIS2_PLACEMENT_3D ( 'NONE', #18380, #19013, #127692 ) ;
#124855 = CIRCLE ( 'NONE', #99729, 0.1000000000000000472 ) ;
#124854 = DIRECTION ( 'NONE',  ( -0.000000000000000000, 1.000000000000000000, -0.000000000000000000 ) ) ;
#124856 = DIRECTION ( 'NONE',  ( 0.000000000000000000, 0.000000000000000000, 1.000000000000000000 ) ) ;
#124857 = EDGE_CURVE ( 'NONE', #4381, #79978, #46323, .T. ) ;
#124858 = DIRECTION ( 'NONE',  ( 0.000000000000000000, 0.000000000000000000, -1.000000000000000000 ) ) ;
#124859 = FACE_OUTER_BOUND ( 'NONE', #46642, .T. ) ;
#124860 = CARTESIAN_POINT ( 'NONE',  ( -10.20000000000000284, 12.50000000000000000, 3.983716857408420964 ) ) ;
#124861 = CARTESIAN_POINT ( 'NONE',  ( -12.69999999999999396, 12.50000000000000000, -3.918623584224386391 ) ) ;
#124862 = CIRCLE ( 'NONE', #20402, 0.09999999999999982514 ) ;
#124863 = VECTOR ( 'NONE', #53478, 1000.000000000000000 ) ;
#124864 = DIRECTION ( 'NONE',  ( -0.000000000000000000, 1.000000000000000000, -0.000000000000000000 ) ) ;
#124865 = ORIENTED_EDGE ( 'NONE', *, *, #69303, .T. ) ;
#124866 = VERTEX_POINT ( 'NONE', #8045 ) ;
#124867 = CIRCLE ( 'NONE', #122806, 0.1000000000000000472 ) ;
#124868 = CIRCLE ( 'NONE', #101880, 0.09999999999999982514 ) ;
#124869 = VERTEX_POINT ( 'NONE', #28999 ) ;
#124870 = ORIENTED_EDGE ( 'NONE', *, *, #53385, .F. ) ;
#124871 = CIRCLE ( 'NONE', #39222, 0.09999999999999982514 ) ;
#124872 = LINE ( 'NONE', #14875, #39459 ) ;
#124873 = DIRECTION ( 'NONE',  ( 0.000000000000000000, 0.000000000000000000, -1.000000000000000000 ) ) ;
#124874 = DIRECTION ( 'NONE',  ( 0.000000000000000000, 1.000000000000000000, 0.000000000000000000 ) ) ;
#124875 = VERTEX_POINT ( 'NONE', #119291 ) ;
#124876 = CARTESIAN_POINT ( 'NONE',  ( -0.2000000000000404232, 2.500000000000000000, 3.983716857408420964 ) ) ;
#124878 = AXIS2_PLACEMENT_3D ( 'NONE', #71840, #113695, #44295 ) ;
#124877 = CIRCLE ( 'NONE', #122816, 0.06509327318403745899 ) ;
#124879 = DIRECTION ( 'NONE',  ( 0.000000000000000000, -0.9999939076577903929, 0.003490651415223739937 ) ) ;
#124881 = EDGE_LOOP ( 'NONE', ( #90664, #102078 ) ) ;
#124880 = CARTESIAN_POINT ( 'NONE',  ( -10.00000000000000711, 2.500000000000000000, -3.637306695894645614 ) ) ;
#124882 = DIRECTION ( 'NONE',  ( 0.000000000000000000, 1.000000000000000000, 0.000000000000000000 ) ) ;
#124883 = ORIENTED_EDGE ( 'NONE', *, *, #124892, .F. ) ;
#124884 = VERTEX_POINT ( 'NONE', #17868 ) ;
#124885 = ORIENTED_EDGE ( 'NONE', *, *, #22829, .F. ) ;
#124886 = VERTEX_POINT ( 'NONE', #119950 ) ;
#124887 = LINE ( 'NONE', #125519, #103265 ) ;
#124888 = AXIS2_PLACEMENT_3D ( 'NONE', #36213, #128468, #96392 ) ;
#124889 = CARTESIAN_POINT ( 'NONE',  ( -14.99999999999998401, 2.500000000000000000, 0.6928203230275518099 ) ) ;
#124890 = PLANE ( 'NONE',  #56666 ) ;
#124891 = CARTESIAN_POINT ( 'NONE',  ( 5.849999999999933920, 2.500000000000000000, -2.857883832488653741 ) ) ;
#124892 = EDGE_CURVE ( 'NONE', #2147, #84545, #4437, .T. ) ;
#124893 = VERTEX_POINT ( 'NONE', #128506 ) ;
#124894 = DIRECTION ( 'NONE',  ( 0.000000000000000000, 0.000000000000000000, 1.000000000000000000 ) ) ;
#124895 = ORIENTED_EDGE ( 'NONE', *, *, #20445, .F. ) ;
#124896 = CARTESIAN_POINT ( 'NONE',  ( 81.97620568616159176, -3.937821671072774699, -6.124242985517362570 ) ) ;
#124898 = EDGE_CURVE ( 'NONE', #77184, #61867, #49940, .T. ) ;
#124897 = CARTESIAN_POINT ( 'NONE',  ( 3.710216157319379260, -2.499999999999999556, -9.999999999879436885 ) ) ;
#124899 = EDGE_CURVE ( 'NONE', #67339, #60096, #121531, .T. ) ;
#124900 = CARTESIAN_POINT ( 'NONE',  ( -8.350000000000013856, 2.500000000000000000, -5.902370205355745192 ) ) ;
#124901 = FACE_OUTER_BOUND ( 'NONE', #70607, .T. ) ;
#124902 = EDGE_CURVE ( 'NONE', #97917, #76656, #108819, .T. ) ;
#124903 = ORIENTED_EDGE ( 'NONE', *, *, #20870, .T. ) ;
#124904 = AXIS2_PLACEMENT_3D ( 'NONE', #121929, #93123, #91177 ) ;
#124905 = ORIENTED_EDGE ( 'NONE', *, *, #128652, .T. ) ;
#124906 = ADVANCED_FACE ( 'NONE', ( #38841 ), #23328, .T. ) ;
#124907 = ORIENTED_EDGE ( 'NONE', *, *, #54934, .T. ) ;
#124908 = DIRECTION ( 'NONE',  ( 0.000000000000000000, 1.000000000000000000, 0.000000000000000000 ) ) ;
#124909 = CARTESIAN_POINT ( 'NONE',  ( -8.150000000000009237, 12.50000000000000000, 6.906693963081109722 ) ) ;
#124910 = FACE_OUTER_BOUND ( 'NONE', #16305, .T. ) ;
#124911 = EDGE_CURVE ( 'NONE', #84876, #86058, #17038, .T. ) ;
#124912 = FACE_BOUND ( 'NONE', #9354, .T. ) ;
#124913 = CARTESIAN_POINT ( 'NONE',  ( 5.199999999999937117, 2.500000000000000000, -4.676537180435978769 ) ) ;
#124914 = DIRECTION ( 'NONE',  ( 0.000000000000000000, 0.000000000000000000, 1.000000000000000000 ) ) ;
#124916 = AXIS2_PLACEMENT_3D ( 'NONE', #126163, #75761, #124237 ) ;
#124915 = VECTOR ( 'NONE', #6372, 1000.000000000000000 ) ;
#124917 = FACE_OUTER_BOUND ( 'NONE', #89275, .T. ) ;
#124918 = CONICAL_SURFACE ( 'NONE', #20367, 0.1000000000000000472, 0.003490658503988666988 ) ;
#124919 = PLANE ( 'NONE',  #111171 ) ;
#124920 = DIRECTION ( 'NONE',  ( -0.000000000000000000, -1.000000000000000000, -0.000000000000000000 ) ) ;
#124921 = DIRECTION ( 'NONE',  ( 0.000000000000000000, 0.000000000000000000, 1.000000000000000000 ) ) ;
#124922 = ORIENTED_EDGE ( 'NONE', *, *, #129542, .F. ) ;
#124923 = CIRCLE ( 'NONE', #5684, 0.1000000000000002554 ) ;
#124924 = FACE_OUTER_BOUND ( 'NONE', #106939, .T. ) ;
#124925 = ORIENTED_EDGE ( 'NONE', *, *, #46150, .T. ) ;
#124926 = EDGE_LOOP ( 'NONE', ( #59770, #8389, #119491, #11917 ) ) ;
#124927 = EDGE_LOOP ( 'NONE', ( #74068, #87749, #103069, #93415 ) ) ;
#124928 = ORIENTED_EDGE ( 'NONE', *, *, #71669, .F. ) ;
#124929 = LINE ( 'NONE', #15602, #63233 ) ;
#124930 = FACE_BOUND ( 'NONE', #27863, .T. ) ;
#124931 = DIRECTION ( 'NONE',  ( 0.000000000000000000, 1.000000000000000000, 0.000000000000000000 ) ) ;
#124932 = CIRCLE ( 'NONE', #16147, 0.06509327318403745899 ) ;
#124933 = VECTOR ( 'NONE', #26459, 1000.000000000000000 ) ;
#124934 = ORIENTED_EDGE ( 'NONE', *, *, #50456, .T. ) ;
#124935 = CARTESIAN_POINT ( 'NONE',  ( 34.93074629416359755, 2.900242961790199026, 4.640733549230978916 ) ) ;
#124936 = CARTESIAN_POINT ( 'NONE',  ( 0.1999999999999636513, 2.500000000000000000, -0.3464101615137760715 ) ) ;
#124937 = AXIS2_PLACEMENT_3D ( 'NONE', #120305, #110476, #31295 ) ;
#124938 = ORIENTED_EDGE ( 'NONE', *, *, #8869, .F. ) ;
#124939 = DIRECTION ( 'NONE',  ( 0.000000000000000000, 0.000000000000000000, -1.000000000000000000 ) ) ;
#124940 = VECTOR ( 'NONE', #436, 1000.000000000000000 ) ;
#124941 = CARTESIAN_POINT ( 'NONE',  ( 3.099999999999945022, 2.500000000000000000, -0.2464101615137783419 ) ) ;
#124942 = AXIS2_PLACEMENT_3D ( 'NONE', #48752, #47454, #88660 ) ;
#124943 = EDGE_CURVE ( 'NONE', #72947, #37042, #127804, .T. ) ;
#124944 = EDGE_LOOP ( 'NONE', ( #57634, #50119, #88946, #93300 ) ) ;
#124945 = ADVANCED_FACE ( 'NONE', ( #80018 ), #21195, .T. ) ;
#124946 = DIRECTION ( 'NONE',  ( -0.000000000000000000, 1.000000000000000000, -0.000000000000000000 ) ) ;
#124947 = DIRECTION ( 'NONE',  ( -4.274815082592931898E-19, -0.9999939076577903929, -0.003490651415223739937 ) ) ;
#124948 = CONICAL_SURFACE ( 'NONE', #116624, 0.09999999999999982514, 0.003490658503988666988 ) ;
#124949 = ADVANCED_FACE ( 'NONE', ( #117327 ), #27441, .T. ) ;
#124950 = VECTOR ( 'NONE', #10173, 1000.000000000000000 ) ;
#124951 = ORIENTED_EDGE ( 'NONE', *, *, #71618, .F. ) ;
#124952 = CONICAL_SURFACE ( 'NONE', #129193, 0.1000000000000002554, 0.003490658503988666988 ) ;
#124953 = CARTESIAN_POINT ( 'NONE',  ( 9.149999999999915090, 12.50000000000000000, -2.165063509461101710 ) ) ;
#124954 = CARTESIAN_POINT ( 'NONE',  ( 186.8645833340161175, -6.668395609140180369, 3.849999999999994760 ) ) ;
#124956 = EDGE_CURVE ( 'NONE', #48671, #74924, #58855, .T. ) ;
#124955 = CARTESIAN_POINT ( 'NONE',  ( -1.450000000000035483, 2.500000000000000000, 1.818653347947321475 ) ) ;
#124957 = EDGE_LOOP ( 'NONE', ( #36890, #29723, #50720, #24404 ) ) ;
#124958 = ORIENTED_EDGE ( 'NONE', *, *, #51074, .T. ) ;
#124959 = AXIS2_PLACEMENT_3D ( 'NONE', #77007, #116916, #27252 ) ;
#124960 = CARTESIAN_POINT ( 'NONE',  ( -0.4000000000000404898, 2.500000000000000000, 4.922947341949748257 ) ) ;
#124961 = EDGE_LOOP ( 'NONE', ( #90087, #29666, #67665, #27731 ) ) ;
#124962 = FACE_OUTER_BOUND ( 'NONE', #21715, .T. ) ;
#124963 = LINE ( 'NONE', #105324, #87118 ) ;
#124964 = EDGE_CURVE ( 'NONE', #11186, #53658, #119480, .T. ) ;
#124967 = EDGE_CURVE ( 'NONE', #67282, #88347, #83878, .T. ) ;
#124966 = CIRCLE ( 'NONE', #93573, 0.1000000000000002554 ) ;
#124965 = AXIS2_PLACEMENT_3D ( 'NONE', #110817, #101004, #13254 ) ;
#124968 = ORIENTED_EDGE ( 'NONE', *, *, #13458, .T. ) ;
#124969 = CARTESIAN_POINT ( 'NONE',  ( 109.3256943381949071, 5.995380816577922545, -4.832476092287897096 ) ) ;
#124970 = CARTESIAN_POINT ( 'NONE',  ( -5.600000000000023626, 2.500000000000000000, -3.883716857408426648 ) ) ;
#124971 = CARTESIAN_POINT ( 'NONE',  ( -11.64999999999999680, 2.500000000000000000, 1.472243186433545459 ) ) ;
#124972 = DIRECTION ( 'NONE',  ( 0.000000000000000000, 0.000000000000000000, 1.000000000000000000 ) ) ;
#124974 = EDGE_CURVE ( 'NONE', #59702, #41439, #69298, .T. ) ;
#124973 = DIRECTION ( 'NONE',  ( -0.000000000000000000, -1.000000000000000000, -0.000000000000000000 ) ) ;
#124975 = EDGE_LOOP ( 'NONE', ( #112288, #124141, #6525, #65746 ) ) ;
#124976 = ORIENTED_EDGE ( 'NONE', *, *, #61463, .T. ) ;
#124977 = CARTESIAN_POINT ( 'NONE',  ( -9.200000000000006395, 2.500000000000000000, 4.330127018922196314 ) ) ;
#124978 = DIRECTION ( 'NONE',  ( 0.000000000000000000, 1.000000000000000000, 0.000000000000000000 ) ) ;
#124979 = DIRECTION ( 'NONE',  ( -0.000000000000000000, 1.000000000000000000, -0.000000000000000000 ) ) ;
#124981 = ORIENTED_EDGE ( 'NONE', *, *, #120603, .F. ) ;
#124980 = VERTEX_POINT ( 'NONE', #48631 ) ;
#124982 = ORIENTED_EDGE ( 'NONE', *, *, #53322, .F. ) ;
#124983 = CARTESIAN_POINT ( 'NONE',  ( -1.450000000000035483, 2.500000000000000000, 6.148780366869520897 ) ) ;
#124984 = CARTESIAN_POINT ( 'NONE',  ( -8.350000000000012079, 12.50000000000000000, -1.407149913249512663 ) ) ;
#124985 = PLANE ( 'NONE',  #66439 ) ;
#124986 = DIRECTION ( 'NONE',  ( -0.000000000000000000, 1.000000000000000000, -0.000000000000000000 ) ) ;
#124987 = DIRECTION ( 'NONE',  ( -0.000000000000000000, -1.000000000000000000, -0.000000000000000000 ) ) ;
#124988 = CARTESIAN_POINT ( 'NONE',  ( 5.849999999999933920, 2.500000000000000000, -2.065063509461102065 ) ) ;
#124989 = DIRECTION ( 'NONE',  ( -0.000000000000000000, 1.000000000000000000, -0.000000000000000000 ) ) ;
#124990 = DIRECTION ( 'NONE',  ( 0.000000000000000000, 0.000000000000000000, -1.000000000000000000 ) ) ;
#124991 = VECTOR ( 'NONE', #65207, 1000.000000000000000 ) ;
#124992 = CARTESIAN_POINT ( 'NONE',  ( -3.950000000000026379, 2.500000000000000000, -1.718653347947326049 ) ) ;
#124994 = ORIENTED_EDGE ( 'NONE', *, *, #66425, .T. ) ;
#124993 = CONICAL_SURFACE ( 'NONE', #93689, 0.09999999999999982514, 0.003490658503988666988 ) ;
#124995 = VECTOR ( 'NONE', #29579, 1000.000000000000000 ) ;
#124996 = DIRECTION ( 'NONE',  ( 0.000000000000000000, 1.000000000000000000, 0.000000000000000000 ) ) ;
#124997 = ORIENTED_EDGE ( 'NONE', *, *, #20448, .T. ) ;
#124998 = EDGE_LOOP ( 'NONE', ( #65320, #42041 ) ) ;
#124999 = FACE_OUTER_BOUND ( 'NONE', #43606, .T. ) ;
#125000 = DIRECTION ( 'NONE',  ( 0.000000000000000000, 0.000000000000000000, -1.000000000000000000 ) ) ;
#125001 = FACE_OUTER_BOUND ( 'NONE', #114821, .T. ) ;
#125002 = CIRCLE ( 'NONE', #70622, 0.06509327318403745899 ) ;
#125003 = DIRECTION ( 'NONE',  ( 0.000000000000000000, 0.000000000000000000, -1.000000000000000000 ) ) ;
#125004 = EDGE_CURVE ( 'NONE', #22231, #56350, #89195, .T. ) ;
#125005 = CIRCLE ( 'NONE', #14269, 0.09999999999999982514 ) ;
#125006 = CARTESIAN_POINT ( 'NONE',  ( 2.099999999999950351, 2.500000000000000000, -4.230127018922201998 ) ) ;
#125007 = DIRECTION ( 'NONE',  ( 0.000000000000000000, -0.000000000000000000, 1.000000000000000000 ) ) ;
#125008 = CARTESIAN_POINT ( 'NONE',  ( -5.400000000000019895, 12.50000000000000000, 3.637306695894644726 ) ) ;
#125009 = EDGE_LOOP ( 'NONE', ( #93900, #61589 ) ) ;
#125010 = DIRECTION ( 'NONE',  ( -0.000000000000000000, -1.000000000000000000, -0.000000000000000000 ) ) ;
#125011 = LINE ( 'NONE', #94911, #70786 ) ;
#125012 = ORIENTED_EDGE ( 'NONE', *, *, #107595, .F. ) ;
#125013 = AXIS2_PLACEMENT_3D ( 'NONE', #70694, #10475, #31426 ) ;
#125014 = ORIENTED_EDGE ( 'NONE', *, *, #9778, .F. ) ;
#125015 = EDGE_LOOP ( 'NONE', ( #128916, #73688 ) ) ;
#125016 = VECTOR ( 'NONE', #80110, 1000.000000000000000 ) ;
#125017 = VERTEX_POINT ( 'NONE', #109484 ) ;
#125018 = FACE_OUTER_BOUND ( 'NONE', #24935, .T. ) ;
#125019 = PLANE ( 'NONE',  #60370 ) ;
#125020 = AXIS2_PLACEMENT_3D ( 'NONE', #88852, #29942, #69196 ) ;
#125021 = DIRECTION ( 'NONE',  ( -0.000000000000000000, -1.000000000000000000, -0.000000000000000000 ) ) ;
#125022 = CARTESIAN_POINT ( 'NONE',  ( 5.399999999999936406, 12.50000000000000000, -5.088040615133791356 ) ) ;
#125023 = AXIS2_PLACEMENT_3D ( 'NONE', #88594, #127240, #58510 ) ;
#125024 = LINE ( 'NONE', #75273, #70183 ) ;
#125025 = ORIENTED_EDGE ( 'NONE', *, *, #38919, .T. ) ;
#125026 = DIRECTION ( 'NONE',  ( -0.000000000000000000, 1.000000000000000000, -0.000000000000000000 ) ) ;
#125027 = FACE_OUTER_BOUND ( 'NONE', #77226, .T. ) ;
#125028 = LINE ( 'NONE', #27454, #8085 ) ;
#125029 = EDGE_LOOP ( 'NONE', ( #61271, #17108, #129173, #98486 ) ) ;
#125030 = AXIS2_PLACEMENT_3D ( 'NONE', #96374, #66917, #78043 ) ;
#125031 = ORIENTED_EDGE ( 'NONE', *, *, #40572, .F. ) ;
#125032 = EDGE_LOOP ( 'NONE', ( #49728, #10133 ) ) ;
#125033 = CARTESIAN_POINT ( 'NONE',  ( 5.849999999999933920, 12.50000000000000000, 6.430097255199259010 ) ) ;
#125034 = CIRCLE ( 'NONE', #70657, 0.1000000000000002554 ) ;
#125035 = DIRECTION ( 'NONE',  ( -0.000000000000000000, -1.000000000000000000, -0.000000000000000000 ) ) ;
#125036 = CARTESIAN_POINT ( 'NONE',  ( -6.650000000000014566, 2.500000000000000000, 1.572243186433545548 ) ) ;
#125037 = ADVANCED_FACE ( 'NONE', ( #59763 ), #100312, .T. ) ;
#125038 = EDGE_LOOP ( 'NONE', ( #120620, #114321, #44803, #91857 ) ) ;
#125039 = LINE ( 'NONE', #72095, #5486 ) ;
#125041 = CIRCLE ( 'NONE', #16352, 7.541925104783893552 ) ;
#125040 = CARTESIAN_POINT ( 'NONE',  ( 0.8499999999999550138, 12.50000000000000000, -5.737276932171712751 ) ) ;
#125042 = ADVANCED_FACE ( 'NONE', ( #67607 ), #42704, .T. ) ;
#125043 = CARTESIAN_POINT ( 'NONE',  ( -11.64999999999999858, 12.50000000000000000, -5.802370205355746435 ) ) ;
#125044 = DIRECTION ( 'NONE',  ( 0.000000000000000000, 0.000000000000000000, -1.000000000000000000 ) ) ;
#125045 = DIRECTION ( 'NONE',  ( 0.000000000000000000, 0.000000000000000000, 1.000000000000000000 ) ) ;
#125046 = EDGE_CURVE ( 'NONE', #98907, #22161, #44179, .T. ) ;
#125047 = EDGE_LOOP ( 'NONE', ( #82526, #51393, #52678, #6912 ) ) ;
#125049 = AXIS2_PLACEMENT_3D ( 'NONE', #41367, #81275, #19096 ) ;
#125048 = CIRCLE ( 'NONE', #49857, 0.06509327318403745899 ) ;
#125050 = DIRECTION ( 'NONE',  ( 0.000000000000000000, -0.9999939076577903929, 0.003490651415223739937 ) ) ;
#125051 = ORIENTED_EDGE ( 'NONE', *, *, #30883, .F. ) ;
#125052 = ADVANCED_FACE ( 'NONE', ( #21753 ), #82612, .T. ) ;
#125054 = ORIENTED_EDGE ( 'NONE', *, *, #29238, .T. ) ;
#125053 = EDGE_CURVE ( 'NONE', #79044, #34557, #23675, .T. ) ;
#125055 = ORIENTED_EDGE ( 'NONE', *, *, #82389, .F. ) ;
#125056 = EDGE_CURVE ( 'NONE', #107604, #62036, #1450, .T. ) ;
#125058 = EDGE_CURVE ( 'NONE', #26135, #101886, #2389, .T. ) ;
#125057 = DIRECTION ( 'NONE',  ( -0.000000000000000000, -1.000000000000000000, -0.000000000000000000 ) ) ;
#125059 = EDGE_CURVE ( 'NONE', #105966, #10113, #102863, .T. ) ;
#125060 = FACE_BOUND ( 'NONE', #80489, .T. ) ;
#125061 = CARTESIAN_POINT ( 'NONE',  ( -9.400000000000009237, 2.500000000000000000, -4.676537180435974328 ) ) ;
#125062 = DIRECTION ( 'NONE',  ( 0.000000000000000000, -0.9999939076577903929, 0.003490651415223739937 ) ) ;
#125063 = CARTESIAN_POINT ( 'NONE',  ( 11.44999999999990870, 2.500000000000000000, 6.841600689897072485 ) ) ;
#125064 = VECTOR ( 'NONE', #81928, 1000.000000000000000 ) ;
#125065 = EDGE_LOOP ( 'NONE', ( #96249, #89912 ) ) ;
#125066 = DIRECTION ( 'NONE',  ( 0.000000000000000000, 0.000000000000000000, 1.000000000000000000 ) ) ;
#125067 = DIRECTION ( 'NONE',  ( 0.000000000000000000, 0.000000000000000000, -1.000000000000000000 ) ) ;
#125068 = EDGE_CURVE ( 'NONE', #11893, #28179, #6577, .T. ) ;
#125069 = FACE_OUTER_BOUND ( 'NONE', #105379, .T. ) ;
#125070 = CARTESIAN_POINT ( 'NONE',  ( -7.700000000000012612, 12.50000000000000000, 4.676537180435972552 ) ) ;
#125071 = ORIENTED_EDGE ( 'NONE', *, *, #123327, .T. ) ;
#125072 = CARTESIAN_POINT ( 'NONE',  ( -1.658312395177699017, -2.500000000000000444, -5.000000000000004441 ) ) ;
#125073 = AXIS2_PLACEMENT_3D ( 'NONE', #83811, #102798, #123721 ) ;
#125074 = LINE ( 'NONE', #43312, #116401 ) ;
#125075 = AXIS2_PLACEMENT_3D ( 'NONE', #21629, #101483, #42577 ) ;
#125076 = VERTEX_POINT ( 'NONE', #2734 ) ;
#125077 = DIRECTION ( 'NONE',  ( 0.000000000000000000, 0.000000000000000000, 1.000000000000000000 ) ) ;
#125078 = ORIENTED_EDGE ( 'NONE', *, *, #109264, .T. ) ;
#125079 = FACE_BOUND ( 'NONE', #65710, .T. ) ;
#125080 = DIRECTION ( 'NONE',  ( -0.000000000000000000, -1.000000000000000000, -0.000000000000000000 ) ) ;
#125081 = AXIS2_PLACEMENT_3D ( 'NONE', #50757, #41600, #14514 ) ;
#125082 = CONICAL_SURFACE ( 'NONE', #68649, 0.1000000000000002554, 0.003490658503988666988 ) ;
#125083 = ORIENTED_EDGE ( 'NONE', *, *, #46571, .T. ) ;
#125084 = DIRECTION ( 'NONE',  ( 0.000000000000000000, 1.000000000000000000, 0.000000000000000000 ) ) ;
#125085 = DIRECTION ( 'NONE',  ( 0.000000000000000000, 0.000000000000000000, 1.000000000000000000 ) ) ;
#125086 = ORIENTED_EDGE ( 'NONE', *, *, #1637, .F. ) ;
#125087 = ORIENTED_EDGE ( 'NONE', *, *, #4456, .T. ) ;
#125088 = CARTESIAN_POINT ( 'NONE',  ( 185.6718750003414016, 9.264065473108010111E-16, -7.564683531250000925 ) ) ;
#125089 = VERTEX_POINT ( 'NONE', #13190 ) ;
#125090 = CARTESIAN_POINT ( 'NONE',  ( 185.6302083336747444, -4.367472073101514418, -7.564683531250002702 ) ) ;
#125091 = CARTESIAN_POINT ( 'NONE',  ( 8.949999999999915801, 2.500000000000000000, 6.841600689897072485 ) ) ;
#125092 = CIRCLE ( 'NONE', #68661, 0.1000000000000002554 ) ;
#125093 = DIRECTION ( 'NONE',  ( -0.000000000000000000, -1.000000000000000000, -0.000000000000000000 ) ) ;
#125094 = DIRECTION ( 'NONE',  ( 0.000000000000000000, 1.000000000000000000, 0.000000000000000000 ) ) ;
#125095 = FACE_OUTER_BOUND ( 'NONE', #6866, .T. ) ;
#125096 = EDGE_CURVE ( 'NONE', #98747, #123356, #40077, .T. ) ;
#125097 = FACE_OUTER_BOUND ( 'NONE', #83780, .T. ) ;
#125098 = EDGE_CURVE ( 'NONE', #31027, #121877, #33512, .T. ) ;
#125099 = CONICAL_SURFACE ( 'NONE', #51963, 0.1000000000000002554, 0.003490658503988666988 ) ;
#125100 = VERTEX_POINT ( 'NONE', #71478 ) ;
#125101 = EDGE_CURVE ( 'NONE', #25385, #3617, #58950, .T. ) ;
#125102 = ORIENTED_EDGE ( 'NONE', *, *, #83433, .T. ) ;
#125103 = PLANE ( 'NONE',  #103100 ) ;
#125104 = CARTESIAN_POINT ( 'NONE',  ( 10.64999999999991331, 2.500000000000000000, 6.148780366869520897 ) ) ;
#125105 = CIRCLE ( 'NONE', #39458, 0.06509327318403745899 ) ;
#125106 = CARTESIAN_POINT ( 'NONE',  ( -12.89999999999999147, 12.50000000000000000, 5.022947341949748790 ) ) ;
#125107 = VECTOR ( 'NONE', #28932, 1000.000000000000000 ) ;
#125108 = CARTESIAN_POINT ( 'NONE',  ( -4.600000000000025402, 2.500000000000000000, 4.330127018922196314 ) ) ;
#125110 = EDGE_LOOP ( 'NONE', ( #35089, #124442, #113840, #100447 ) ) ;
#125109 = ORIENTED_EDGE ( 'NONE', *, *, #21427, .T. ) ;
#125111 = FACE_BOUND ( 'NONE', #66914, .T. ) ;
#125112 = EDGE_LOOP ( 'NONE', ( #25049, #54528 ) ) ;
#125113 = EDGE_CURVE ( 'NONE', #94097, #9132, #430, .T. ) ;
#125114 = CARTESIAN_POINT ( 'NONE',  ( 11.64999999999990621, 2.500000000000000000, -2.165063509461101710 ) ) ;
#125115 = CARTESIAN_POINT ( 'NONE',  ( -7.050000000000016698, 12.50000000000000000, -6.495190528383302464 ) ) ;
#125117 = ORIENTED_EDGE ( 'NONE', *, *, #79108, .T. ) ;
#125116 = ADVANCED_FACE ( 'NONE', ( #12552 ), #71450, .T. ) ;
#125118 = FACE_OUTER_BOUND ( 'NONE', #129435, .T. ) ;
#125119 = AXIS2_PLACEMENT_3D ( 'NONE', #24726, #45018, #113098 ) ;
#125120 = DIRECTION ( 'NONE',  ( -0.000000000000000000, -1.000000000000000000, -0.000000000000000000 ) ) ;
#125121 = ADVANCED_FACE ( 'NONE', ( #810 ), #10793, .T. ) ;
#125122 = DIRECTION ( 'NONE',  ( -4.274815082592931898E-19, -0.9999939076577903929, -0.003490651415223739937 ) ) ;
#125123 = EDGE_CURVE ( 'NONE', #35030, #106850, #8751, .T. ) ;
#125124 = CARTESIAN_POINT ( 'NONE',  ( 6.899999999999928413, 2.500000000000000000, 4.676537180435972552 ) ) ;
#125125 = DIRECTION ( 'NONE',  ( 0.000000000000000000, 0.000000000000000000, 1.000000000000000000 ) ) ;
#125126 = CARTESIAN_POINT ( 'NONE',  ( -4.150000000000028777, 2.500000000000000000, -5.902370205355750521 ) ) ;
#125127 = DIRECTION ( 'NONE',  ( -0.000000000000000000, -1.000000000000000000, -0.000000000000000000 ) ) ;
#125128 = DIRECTION ( 'NONE',  ( -0.000000000000000000, 1.000000000000000000, -0.000000000000000000 ) ) ;
#125129 = AXIS2_PLACEMENT_3D ( 'NONE', #56863, #64764, #64126 ) ;
#125131 = ADVANCED_FACE ( 'NONE', ( #100933 ), #51224, .T. ) ;
#125130 = DIRECTION ( 'NONE',  ( 0.000000000000000000, 0.000000000000000000, -1.000000000000000000 ) ) ;
#125133 = ORIENTED_EDGE ( 'NONE', *, *, #205, .F. ) ;
#125132 = AXIS2_PLACEMENT_3D ( 'NONE', #13792, #35392, #113291 ) ;
#125134 = VERTEX_POINT ( 'NONE', #91129 ) ;
#125135 = CARTESIAN_POINT ( 'NONE',  ( 6.849999999999930367, 2.500000000000000000, -6.841600689897078702 ) ) ;
#125136 = ORIENTED_EDGE ( 'NONE', *, *, #10650, .T. ) ;
#125137 = FACE_OUTER_BOUND ( 'NONE', #20631, .T. ) ;
#125139 = VERTEX_POINT ( 'NONE', #30938 ) ;
#125138 = VERTEX_POINT ( 'NONE', #22409 ) ;
#125140 = ORIENTED_EDGE ( 'NONE', *, *, #47535, .F. ) ;
#125141 = AXIS2_PLACEMENT_3D ( 'NONE', #115933, #55724, #76659 ) ;
#125142 = DIRECTION ( 'NONE',  ( 0.000000000000000000, 1.000000000000000000, 0.000000000000000000 ) ) ;
#125143 = CARTESIAN_POINT ( 'NONE',  ( 3.749999999999944045, 2.500000000000000000, -7.288010851410854585 ) ) ;
#125144 = CIRCLE ( 'NONE', #85424, 0.1000000000000002554 ) ;
#125145 = CARTESIAN_POINT ( 'NONE',  ( 65.39894234709436205, -3.129862333804463326, -5.811320850207112088 ) ) ;
#125146 = DIRECTION ( 'NONE',  ( 0.000000000000000000, 0.000000000000000000, 1.000000000000000000 ) ) ;
#125147 = LINE ( 'NONE', #16457, #1567 ) ;
#125148 = AXIS2_PLACEMENT_3D ( 'NONE', #111735, #22085, #4328 ) ;
#125149 = EDGE_CURVE ( 'NONE', #16388, #114720, #53146, .T. ) ;
#125150 = ORIENTED_EDGE ( 'NONE', *, *, #39793, .F. ) ;
#125151 = CARTESIAN_POINT ( 'NONE',  ( 0.8499999999999536815, 2.500000000000000000, 6.495190528383297135 ) ) ;
#125152 = VERTEX_POINT ( 'NONE', #95639 ) ;
#125154 = AXIS2_PLACEMENT_3D ( 'NONE', #96066, #78384, #126177 ) ;
#125153 = AXIS2_PLACEMENT_3D ( 'NONE', #72945, #123332, #52647 ) ;
#125155 = ORIENTED_EDGE ( 'NONE', *, *, #19982, .F. ) ;
#125156 = EDGE_LOOP ( 'NONE', ( #118681, #60975, #61053, #114182 ) ) ;
#125157 = CARTESIAN_POINT ( 'NONE',  ( -7.100000000000018296, 2.500000000000000000, -4.230127018922201998 ) ) ;
#125158 = ORIENTED_EDGE ( 'NONE', *, *, #73106, .F. ) ;
#125159 = VERTEX_POINT ( 'NONE', #4022 ) ;
#125160 = ORIENTED_EDGE ( 'NONE', *, *, #82509, .T. ) ;
#125161 = DIRECTION ( 'NONE',  ( 0.000000000000000000, 0.000000000000000000, 1.000000000000000000 ) ) ;
#125162 = DIRECTION ( 'NONE',  ( -0.000000000000000000, -1.000000000000000000, -0.000000000000000000 ) ) ;
#125163 = CARTESIAN_POINT ( 'NONE',  ( 11.64999999999990621, 2.500000000000000000, 6.495190528383297135 ) ) ;
#125164 = ADVANCED_FACE ( 'NONE', ( #124459 ), #52686, .T. ) ;
#125165 = CARTESIAN_POINT ( 'NONE',  ( -13.34999999999999076, 2.500000000000000000, -2.857883832488651521 ) ) ;
#125166 = CARTESIAN_POINT ( 'NONE',  ( -12.09999999999999609, 12.50000000000000000, -5.088040615133788691 ) ) ;
#125168 = AXIS2_PLACEMENT_3D ( 'NONE', #124297, #113837, #34650 ) ;
#125167 = CARTESIAN_POINT ( 'NONE',  ( 13.74999999999989342, 2.500000000000000000, -1.472243186433550122 ) ) ;
#125169 = ORIENTED_EDGE ( 'NONE', *, *, #97444, .T. ) ;
#125170 = CARTESIAN_POINT ( 'NONE',  ( 15.39999999999989200, 2.500000000000000000, -0.6928203230275542523 ) ) ;
#125171 = ORIENTED_EDGE ( 'NONE', *, *, #60662, .T. ) ;
#125173 = PLANE ( 'NONE',  #77762 ) ;
#125172 = VECTOR ( 'NONE', #122953, 1000.000000000000000 ) ;
#125175 = EDGE_LOOP ( 'NONE', ( #78759, #671 ) ) ;
#125174 = VECTOR ( 'NONE', #19224, 1000.000000000000000 ) ;
#125176 = CARTESIAN_POINT ( 'NONE',  ( 185.8645833340161175, -6.668395609140180369, 3.849999999999994760 ) ) ;
#125177 = CIRCLE ( 'NONE', #102193, 0.06509327318403745899 ) ;
#125178 = VERTEX_POINT ( 'NONE', #56345 ) ;
#125179 = EDGE_CURVE ( 'NONE', #126922, #56443, #104897, .T. ) ;
#125180 = VERTEX_POINT ( 'NONE', #5946 ) ;
#125181 = DIRECTION ( 'NONE',  ( 0.000000000000000000, 1.000000000000000000, 0.000000000000000000 ) ) ;
#125182 = DIRECTION ( 'NONE',  ( -0.000000000000000000, 1.000000000000000000, -0.000000000000000000 ) ) ;
#125183 = AXIS2_PLACEMENT_3D ( 'NONE', #94889, #5842, #45799 ) ;
#125184 = AXIS2_PLACEMENT_3D ( 'NONE', #18088, #17431, #117553 ) ;
#125185 = CARTESIAN_POINT ( 'NONE',  ( -14.99999999999994671, 12.50000000000000000, -0.06509327318403743123 ) ) ;
#125186 = DIRECTION ( 'NONE',  ( -0.000000000000000000, -1.000000000000000000, -0.000000000000000000 ) ) ;
#125187 = DIRECTION ( 'NONE',  ( 0.000000000000000000, 1.000000000000000000, 0.000000000000000000 ) ) ;
#125188 = ORIENTED_EDGE ( 'NONE', *, *, #74151, .F. ) ;
#125189 = LINE ( 'NONE', #43429, #26822 ) ;
#125190 = CARTESIAN_POINT ( 'NONE',  ( 11.89999999999990798, 2.500000000000000000, 4.676537180435972552 ) ) ;
#125191 = DIRECTION ( 'NONE',  ( 0.000000000000000000, -0.9999939076577903929, 0.003490651415223739937 ) ) ;
#125192 = DIRECTION ( 'NONE',  ( 0.000000000000000000, 0.000000000000000000, 1.000000000000000000 ) ) ;
#125193 = CIRCLE ( 'NONE', #41591, 0.06509327318403745899 ) ;
#125194 = FACE_OUTER_BOUND ( 'NONE', #99060, .T. ) ;
#125195 = AXIS2_PLACEMENT_3D ( 'NONE', #11688, #11031, #52913 ) ;
#125196 = VERTEX_POINT ( 'NONE', #85169 ) ;
#125197 = VERTEX_POINT ( 'NONE', #64241 ) ;
#125198 = ORIENTED_EDGE ( 'NONE', *, *, #3346, .T. ) ;
#125199 = DIRECTION ( 'NONE',  ( 0.000000000000000000, 0.000000000000000000, -1.000000000000000000 ) ) ;
#125201 = CONICAL_SURFACE ( 'NONE', #12321, 0.1000000000000000472, 0.003490658503988666988 ) ;
#125200 = DIRECTION ( 'NONE',  ( -0.000000000000000000, 1.000000000000000000, -0.000000000000000000 ) ) ;
#125202 = EDGE_CURVE ( 'NONE', #120397, #25624, #90312, .T. ) ;
#125203 = CIRCLE ( 'NONE', #93813, 0.09999999999999999167 ) ;
#125204 = CARTESIAN_POINT ( 'NONE',  ( 187.5000000000000000, 0.000000000000000000, 7.700000000000000178 ) ) ;
#125205 = CARTESIAN_POINT ( 'NONE',  ( -11.89999999999999680, 2.500000000000000000, -4.776537180435975749 ) ) ;
#125206 = LINE ( 'NONE', #27011, #115603 ) ;
#125207 = CARTESIAN_POINT ( 'NONE',  ( 5.199999999999935341, 2.500000000000000000, -4.083716857408426826 ) ) ;
#125208 = DIRECTION ( 'NONE',  ( 0.000000000000000000, -0.9999939076577903929, 0.003490651415223739937 ) ) ;
#125209 = ORIENTED_EDGE ( 'NONE', *, *, #3910, .T. ) ;
#125210 = DIRECTION ( 'NONE',  ( 0.000000000000000000, 0.000000000000000000, -1.000000000000000000 ) ) ;
#125211 = DIRECTION ( 'NONE',  ( 0.000000000000000000, 0.000000000000000000, 1.000000000000000000 ) ) ;
#125212 = AXIS2_PLACEMENT_3D ( 'NONE', #12785, #92011, #2318 ) ;
#125213 = ORIENTED_EDGE ( 'NONE', *, *, #25813, .T. ) ;
#125214 = ADVANCED_FACE ( 'NONE', ( #46524 ), #34807, .T. ) ;
#125215 = ADVANCED_FACE ( 'NONE', ( #45901 ), #125830, .T. ) ;
#125216 = EDGE_CURVE ( 'NONE', #61323, #7453, #48477, .T. ) ;
#125218 = ADVANCED_FACE ( 'NONE', ( #75992 ), #111152, .T. ) ;
#125217 = DIRECTION ( 'NONE',  ( -0.000000000000000000, 1.000000000000000000, -0.000000000000000000 ) ) ;
#125219 = AXIS2_PLACEMENT_3D ( 'NONE', #99733, #69610, #91191 ) ;
#125220 = CARTESIAN_POINT ( 'NONE',  ( -8.550000000000009592, 12.50000000000000000, 6.906693963081109722 ) ) ;
#125221 = CARTESIAN_POINT ( 'NONE',  ( 6.249999999999932498, 2.500000000000000000, -2.857883832488653741 ) ) ;
#125222 = ORIENTED_EDGE ( 'NONE', *, *, #112984, .F. ) ;
#125223 = DIRECTION ( 'NONE',  ( -0.000000000000000000, 1.000000000000000000, -0.000000000000000000 ) ) ;
#125224 = ORIENTED_EDGE ( 'NONE', *, *, #100392, .T. ) ;
#125226 = CIRCLE ( 'NONE', #112710, 0.1000000000000002554 ) ;
#125225 = DIRECTION ( 'NONE',  ( 0.000000000000000000, 1.000000000000000000, 0.000000000000000000 ) ) ;
#125227 = CARTESIAN_POINT ( 'NONE',  ( 11.84999999999990372, 2.500000000000000000, 2.411473670974873862 ) ) ;
#125228 = ADVANCED_FACE ( 'NONE', ( #113996 ), #33908, .T. ) ;
#125229 = EDGE_LOOP ( 'NONE', ( #107325, #37043 ) ) ;
#125230 = ADVANCED_FACE ( 'NONE', ( #125097 ), #73602, .T. ) ;
#125232 = EDGE_CURVE ( 'NONE', #44668, #73184, #66801, .T. ) ;
#125231 = CARTESIAN_POINT ( 'NONE',  ( 185.6145833340161175, 6.668395609140177704, -3.849999999999998312 ) ) ;
#125234 = CIRCLE ( 'NONE', #12352, 0.06509327318403745899 ) ;
#125233 = AXIS2_PLACEMENT_3D ( 'NONE', #22971, #31498, #92336 ) ;
#125235 = DIRECTION ( 'NONE',  ( 0.000000000000000000, 0.000000000000000000, -1.000000000000000000 ) ) ;
#125236 = CIRCLE ( 'NONE', #112720, 0.06509327318403743123 ) ;
#125237 = VERTEX_POINT ( 'NONE', #104170 ) ;
#125238 = DIRECTION ( 'NONE',  ( 0.000000000000000000, 0.000000000000000000, 1.000000000000000000 ) ) ;
#125240 = AXIS2_PLACEMENT_3D ( 'NONE', #124085, #74343, #114264 ) ;
#125239 = AXIS2_PLACEMENT_3D ( 'NONE', #12310, #51612, #101353 ) ;
#125241 = ORIENTED_EDGE ( 'NONE', *, *, #26353, .F. ) ;
#125242 = VERTEX_POINT ( 'NONE', #75342 ) ;
#125243 = DIRECTION ( 'NONE',  ( 0.000000000000000000, 0.000000000000000000, 1.000000000000000000 ) ) ;
#125244 = DIRECTION ( 'NONE',  ( 0.000000000000000000, 0.000000000000000000, 1.000000000000000000 ) ) ;
#125245 = EDGE_LOOP ( 'NONE', ( #59864, #95228 ) ) ;
#125246 = LINE ( 'NONE', #113482, #113696 ) ;
#125247 = DIRECTION ( 'NONE',  ( 0.000000000000000000, 0.000000000000000000, 1.000000000000000000 ) ) ;
#125248 = EDGE_LOOP ( 'NONE', ( #59140, #51582, #30346, #97137 ) ) ;
#125249 = CARTESIAN_POINT ( 'NONE',  ( -3.150000000000029221, 2.500000000000000000, 2.511473670974873507 ) ) ;
#125250 = CARTESIAN_POINT ( 'NONE',  ( -10.00000000000000355, 2.500000000000000000, 3.637306695894644726 ) ) ;
#125251 = DIRECTION ( 'NONE',  ( -0.000000000000000000, -1.000000000000000000, -0.000000000000000000 ) ) ;
#125252 = AXIS2_PLACEMENT_3D ( 'NONE', #87897, #19836, #10006 ) ;
#125253 = CARTESIAN_POINT ( 'NONE',  ( 10.84999999999991260, 2.500000000000000000, -2.265063509461101798 ) ) ;
#125254 = CARTESIAN_POINT ( 'NONE',  ( -13.74999999999995381, 2.500000000000000000, -2.265063509461099578 ) ) ;
#125255 = DIRECTION ( 'NONE',  ( 0.000000000000000000, 0.000000000000000000, -1.000000000000000000 ) ) ;
#125256 = CONICAL_SURFACE ( 'NONE', #121050, 0.1000000000000002554, 0.003490658503988666988 ) ;
#125257 = CONICAL_SURFACE ( 'NONE', #3972, 0.09999999999999982514, 0.003490658503988666988 ) ;
#125258 = ORIENTED_EDGE ( 'NONE', *, *, #91626, .T. ) ;
#125259 = ORIENTED_EDGE ( 'NONE', *, *, #94771, .T. ) ;
#125260 = ORIENTED_EDGE ( 'NONE', *, *, #7895, .F. ) ;
#125261 = EDGE_LOOP ( 'NONE', ( #98105, #63531 ) ) ;
#125262 = CARTESIAN_POINT ( 'NONE',  ( 4.199999999999939782, 2.500000000000000000, -2.276824562219559311E-15 ) ) ;
#125263 = CARTESIAN_POINT ( 'NONE',  ( -3.750000000000031086, 12.50000000000000000, -5.802370205355749988 ) ) ;
#125264 = LINE ( 'NONE', #84035, #76123 ) ;
#125265 = ORIENTED_EDGE ( 'NONE', *, *, #41155, .T. ) ;
#125266 = FACE_BOUND ( 'NONE', #71485, .T. ) ;
#125267 = DIRECTION ( 'NONE',  ( 0.000000000000000000, 0.000000000000000000, -1.000000000000000000 ) ) ;
#125268 = PLANE ( 'NONE',  #73098 ) ;
#125269 = AXIS2_PLACEMENT_3D ( 'NONE', #47932, #95089, #17799 ) ;
#125270 = CIRCLE ( 'NONE', #85555, 0.06509327318403745899 ) ;
#125271 = EDGE_CURVE ( 'NONE', #53553, #43500, #98632, .T. ) ;
#125272 = CARTESIAN_POINT ( 'NONE',  ( -1.450000000000035483, 12.50000000000000000, 1.818653347947321475 ) ) ;
#125273 = AXIS2_PLACEMENT_3D ( 'NONE', #115282, #117218, #34848 ) ;
#125274 = DIRECTION ( 'NONE',  ( 0.000000000000000000, 1.000000000000000000, 0.000000000000000000 ) ) ;
#125275 = ADVANCED_FACE ( 'NONE', ( #93705 ), #107046, .T. ) ;
#125276 = DIRECTION ( 'NONE',  ( 0.000000000000000000, 0.000000000000000000, -1.000000000000000000 ) ) ;
#125277 = DIRECTION ( 'NONE',  ( -4.274815082592931898E-19, -0.9999939076577903929, -0.003490651415223739937 ) ) ;
#125278 = CARTESIAN_POINT ( 'NONE',  ( -11.84999999999999787, 2.500000000000000000, -2.411473670974874306 ) ) ;
#125279 = DIRECTION ( 'NONE',  ( -0.000000000000000000, -1.000000000000000000, -0.000000000000000000 ) ) ;
#125280 = DIRECTION ( 'NONE',  ( -0.000000000000000000, 1.000000000000000000, -0.000000000000000000 ) ) ;
#125281 = VECTOR ( 'NONE', #40911, 1000.000000000000000 ) ;
#125283 = EDGE_CURVE ( 'NONE', #64666, #62380, #83873, .T. ) ;
#125282 = CARTESIAN_POINT ( 'NONE',  ( 12.69999999999989981, 2.500000000000000000, -0.3464101615137783474 ) ) ;
#125284 = CIRCLE ( 'NONE', #68844, 0.09999999999999982514 ) ;
#125285 = ORIENTED_EDGE ( 'NONE', *, *, #128561, .T. ) ;
#125286 = ORIENTED_EDGE ( 'NONE', *, *, #34112, .F. ) ;
#125287 = CONICAL_SURFACE ( 'NONE', #18759, 0.1000000000000002554, 0.003490658503988666988 ) ;
#125288 = ORIENTED_EDGE ( 'NONE', *, *, #63931, .T. ) ;
#125289 = VERTEX_POINT ( 'NONE', #6573 ) ;
#125290 = DIRECTION ( 'NONE',  ( -0.000000000000000000, -1.000000000000000000, -0.000000000000000000 ) ) ;
#125291 = ORIENTED_EDGE ( 'NONE', *, *, #38288, .T. ) ;
#125292 = DIRECTION ( 'NONE',  ( -0.000000000000000000, -1.000000000000000000, -0.000000000000000000 ) ) ;
#125293 = VERTEX_POINT ( 'NONE', #114623 ) ;
#125294 = ORIENTED_EDGE ( 'NONE', *, *, #49847, .F. ) ;
#125295 = DIRECTION ( 'NONE',  ( 0.000000000000000000, 0.000000000000000000, 1.000000000000000000 ) ) ;
#125296 = CARTESIAN_POINT ( 'NONE',  ( 9.112263991835156673, -1.499999999999809042, 9.392448311626335311 ) ) ;
#125297 = DIRECTION ( 'NONE',  ( 0.000000000000000000, 1.000000000000000000, 0.000000000000000000 ) ) ;
#125298 = DIRECTION ( 'NONE',  ( 0.000000000000000000, 0.000000000000000000, 1.000000000000000000 ) ) ;
#125299 = AXIS2_PLACEMENT_3D ( 'NONE', #107144, #17469, #56112 ) ;
#125300 = LINE ( 'NONE', #66371, #120832 ) ;
#125301 = VERTEX_POINT ( 'NONE', #115240 ) ;
#125302 = EDGE_LOOP ( 'NONE', ( #124013, #64275 ) ) ;
#125303 = ORIENTED_EDGE ( 'NONE', *, *, #116245, .F. ) ;
#125305 = ORIENTED_EDGE ( 'NONE', *, *, #89146, .F. ) ;
#125304 = CARTESIAN_POINT ( 'NONE',  ( -1.850000000000033396, 12.50000000000000000, -6.148780366869526226 ) ) ;
#125306 = CARTESIAN_POINT ( 'NONE',  ( -11.24999999999999822, 12.50000000000000000, 5.867463478539781896 ) ) ;
#125307 = VERTEX_POINT ( 'NONE', #123790 ) ;
#125308 = ORIENTED_EDGE ( 'NONE', *, *, #8309, .T. ) ;
#125309 = CIRCLE ( 'NONE', #114829, 0.06509327318403745899 ) ;
#125310 = CARTESIAN_POINT ( 'NONE',  ( 15.59999999999988951, 2.500000000000000000, -0.2464101615137783419 ) ) ;
#125311 = DIRECTION ( 'NONE',  ( -4.274815082592931898E-19, -0.9999939076577903929, -0.003490651415223739937 ) ) ;
#125312 = CARTESIAN_POINT ( 'NONE',  ( -2.700000000000030820, 2.500000000000000000, 0.2464101615137735679 ) ) ;
#125313 = EDGE_CURVE ( 'NONE', #94142, #99145, #64872, .T. ) ;
#125314 = CARTESIAN_POINT ( 'NONE',  ( 6.899999999999928413, 12.50000000000000000, 4.048810130592458201 ) ) ;
#125315 = DIRECTION ( 'NONE',  ( 0.000000000000000000, -0.000000000000000000, 1.000000000000000000 ) ) ;
#125316 = PLANE ( 'NONE',  #39352 ) ;
#125317 = CIRCLE ( 'NONE', #127381, 0.1000000000000000472 ) ;
#125318 = VERTEX_POINT ( 'NONE', #45258 ) ;
#125319 = CARTESIAN_POINT ( 'NONE',  ( -8.550000000000014921, 12.50000000000000000, -6.083687093685483660 ) ) ;
#125320 = ORIENTED_EDGE ( 'NONE', *, *, #37320, .T. ) ;
#125321 = DIRECTION ( 'NONE',  ( -0.000000000000000000, -1.000000000000000000, -0.000000000000000000 ) ) ;
#125323 = AXIS2_PLACEMENT_3D ( 'NONE', #59421, #99327, #9650 ) ;
#125322 = AXIS2_PLACEMENT_3D ( 'NONE', #43907, #82542, #3324 ) ;
#125324 = ORIENTED_EDGE ( 'NONE', *, *, #1494, .F. ) ;
#125325 = FACE_OUTER_BOUND ( 'NONE', #72234, .T. ) ;
#125326 = FACE_OUTER_BOUND ( 'NONE', #29386, .T. ) ;
#125327 = EDGE_CURVE ( 'NONE', #22783, #22326, #42234, .T. ) ;
#125328 = ORIENTED_EDGE ( 'NONE', *, *, #122085, .T. ) ;
#125329 = CIRCLE ( 'NONE', #71045, 0.06509327318403745899 ) ;
#125330 = FACE_OUTER_BOUND ( 'NONE', #32430, .T. ) ;
#125331 = ADVANCED_FACE ( 'NONE', ( #108027 ), #12954, .T. ) ;
#125332 = DIRECTION ( 'NONE',  ( -0.000000000000000000, 1.000000000000000000, -0.000000000000000000 ) ) ;
#125333 = ORIENTED_EDGE ( 'NONE', *, *, #53147, .T. ) ;
#125334 = LINE ( 'NONE', #105702, #21435 ) ;
#125336 = CIRCLE ( 'NONE', #85615, 0.1000000000000002554 ) ;
#125335 = VECTOR ( 'NONE', #111492, 1000.000000000000000 ) ;
#125337 = LINE ( 'NONE', #16008, #96787 ) ;
#125338 = EDGE_LOOP ( 'NONE', ( #54858, #49426, #42813, #63332 ) ) ;
#125340 = VERTEX_POINT ( 'NONE', #79863 ) ;
#125339 = EDGE_CURVE ( 'NONE', #127915, #87106, #102840, .T. ) ;
#125341 = CARTESIAN_POINT ( 'NONE',  ( 0.8499999999999545697, 2.500000000000000000, 2.857883832488649301 ) ) ;
#125342 = DIRECTION ( 'NONE',  ( 0.000000000000000000, 0.000000000000000000, -1.000000000000000000 ) ) ;
#125343 = CARTESIAN_POINT ( 'NONE',  ( 186.2552083336747444, 6.551208109652275624, -3.782341765624998686 ) ) ;
#125344 = DIRECTION ( 'NONE',  ( 0.000000000000000000, 0.000000000000000000, 1.000000000000000000 ) ) ;
#125345 = DIRECTION ( 'NONE',  ( 0.000000000000000000, -0.9999939076577903929, 0.003490651415223739937 ) ) ;
#125346 = DIRECTION ( 'NONE',  ( 0.000000000000000000, 0.000000000000000000, 1.000000000000000000 ) ) ;
#125347 = AXIS2_PLACEMENT_3D ( 'NONE', #87261, #9362, #39496 ) ;
#125348 = ORIENTED_EDGE ( 'NONE', *, *, #128595, .T. ) ;
#125349 = DIRECTION ( 'NONE',  ( 0.000000000000000000, 1.000000000000000000, 0.000000000000000000 ) ) ;
#125350 = VECTOR ( 'NONE', #90356, 1000.000000000000000 ) ;
#125351 = EDGE_CURVE ( 'NONE', #61737, #2171, #67429, .T. ) ;
#125352 = ORIENTED_EDGE ( 'NONE', *, *, #35722, .T. ) ;
#125353 = DIRECTION ( 'NONE',  ( -4.274815082592931898E-19, -0.9999939076577903929, -0.003490651415223739937 ) ) ;
#125354 = LINE ( 'NONE', #55335, #491 ) ;
#125355 = CARTESIAN_POINT ( 'NONE',  ( -12.09999999999999609, 2.500000000000000000, 4.330127018922196314 ) ) ;
#125356 = AXIS2_PLACEMENT_3D ( 'NONE', #42123, #61777, #72871 ) ;
#125357 = VERTEX_POINT ( 'NONE', #69391 ) ;
#125359 = CIRCLE ( 'NONE', #41758, 0.1000000000000002554 ) ;
#125358 = CIRCLE ( 'NONE', #45955, 0.06509327318403745899 ) ;
#125360 = ADVANCED_FACE ( 'NONE', ( #98850 ), #10887, .T. ) ;
#125361 = CARTESIAN_POINT ( 'NONE',  ( -10.20000000000000284, 2.500000000000000000, 3.883716857408421319 ) ) ;
#125362 = CARTESIAN_POINT ( 'NONE',  ( -11.84999999999999609, 2.500000000000000000, 1.718653347947321386 ) ) ;
#125363 = EDGE_CURVE ( 'NONE', #108419, #7922, #96575, .T. ) ;
#125364 = ADVANCED_FACE ( 'NONE', ( #117176 ), #98205, .T. ) ;
#125365 = EDGE_CURVE ( 'NONE', #126837, #36298, #40179, .T. ) ;
#125367 = EDGE_CURVE ( 'NONE', #43127, #105608, #117405, .T. ) ;
#125366 = AXIS2_PLACEMENT_3D ( 'NONE', #94320, #4636, #44595 ) ;
#125368 = ORIENTED_EDGE ( 'NONE', *, *, #13888, .T. ) ;
#125369 = CARTESIAN_POINT ( 'NONE',  ( -0.4000000000000404898, 12.50000000000000000, 5.088040615133786027 ) ) ;
#125370 = AXIS2_PLACEMENT_3D ( 'NONE', #14580, #92507, #32974 ) ;
#125371 = AXIS2_PLACEMENT_3D ( 'NONE', #4617, #45227, #53747 ) ;
#125372 = ORIENTED_EDGE ( 'NONE', *, *, #20926, .F. ) ;
#125373 = VERTEX_POINT ( 'NONE', #8524 ) ;
#125374 = FACE_OUTER_BOUND ( 'NONE', #4871, .T. ) ;
#125375 = ADVANCED_FACE ( 'NONE', ( #127669 ), #77283, .T. ) ;
#125376 = ADVANCED_FACE ( 'NONE', ( #89044 ), #13038, .T. ) ;
#125377 = EDGE_LOOP ( 'NONE', ( #19357, #109610, #28648, #17344 ) ) ;
#125378 = DIRECTION ( 'NONE',  ( 0.000000000000000000, -0.000000000000000000, 1.000000000000000000 ) ) ;
#125379 = DIRECTION ( 'NONE',  ( -4.274815082592931898E-19, -0.9999939076577903929, -0.003490651415223739937 ) ) ;
#125380 = CIRCLE ( 'NONE', #85662, 3.000000000000000000 ) ;
#125381 = DIRECTION ( 'NONE',  ( -0.000000000000000000, 1.000000000000000000, -0.000000000000000000 ) ) ;
#125382 = ORIENTED_EDGE ( 'NONE', *, *, #33167, .F. ) ;
#125383 = ADVANCED_FACE ( 'NONE', ( #27519 ), #77921, .T. ) ;
#125385 = ADVANCED_FACE ( 'NONE', ( #78598 ), #119143, .T. ) ;
#125384 = FACE_BOUND ( 'NONE', #63845, .T. ) ;
#125387 = ORIENTED_EDGE ( 'NONE', *, *, #58610, .T. ) ;
#125386 = CARTESIAN_POINT ( 'NONE',  ( -2.300000000000033573, 2.500000000000000000, 4.676537180435972552 ) ) ;
#125388 = AXIS2_PLACEMENT_3D ( 'NONE', #121919, #91812, #44651 ) ;
#125389 = DIRECTION ( 'NONE',  ( 0.000000000000000000, 0.000000000000000000, -1.000000000000000000 ) ) ;
#125390 = ADVANCED_FACE ( 'NONE', ( #28842 ), #68750, .T. ) ;
#125391 = DIRECTION ( 'NONE',  ( 0.000000000000000000, 0.000000000000000000, -1.000000000000000000 ) ) ;
#125392 = EDGE_CURVE ( 'NONE', #80186, #128041, #121289, .T. ) ;
#125393 = ORIENTED_EDGE ( 'NONE', *, *, #87935, .T. ) ;
#125394 = ORIENTED_EDGE ( 'NONE', *, *, #12606, .F. ) ;
#125395 = ORIENTED_EDGE ( 'NONE', *, *, #66681, .T. ) ;
#125396 = CARTESIAN_POINT ( 'NONE',  ( -8.550000000000011369, 2.500000000000000000, 1.818653347947321475 ) ) ;
#125397 = CARTESIAN_POINT ( 'NONE',  ( 3.677269697638545054, 2.500000000000000000, 8.999999999909123360 ) ) ;
#125398 = CARTESIAN_POINT ( 'NONE',  ( -4.200000000000025935, 12.50000000000000000, -2.385244779468109755E-15 ) ) ;
#125399 = FACE_BOUND ( 'NONE', #13106, .T. ) ;
#125400 = ORIENTED_EDGE ( 'NONE', *, *, #58616, .T. ) ;
#125401 = CARTESIAN_POINT ( 'NONE',  ( 185.7760416670080588, 6.551208109652274736, 3.782341765625001351 ) ) ;
#125402 = DIRECTION ( 'NONE',  ( 0.000000000000000000, 1.000000000000000000, 0.000000000000000000 ) ) ;
#125403 = CARTESIAN_POINT ( 'NONE',  ( -1.050000000000037348, 2.500000000000000000, -6.841600689897078702 ) ) ;
#125404 = DIRECTION ( 'NONE',  ( 0.000000000000000000, 0.000000000000000000, 1.000000000000000000 ) ) ;
#125405 = DIRECTION ( 'NONE',  ( 0.000000000000000000, 1.000000000000000000, 0.000000000000000000 ) ) ;
#125406 = DIRECTION ( 'NONE',  ( 0.000000000000000000, 1.000000000000000000, -1.846105847067148761E-16 ) ) ;
#125407 = AXIS2_PLACEMENT_3D ( 'NONE', #24844, #26140, #6450 ) ;
#125408 = DIRECTION ( 'NONE',  ( 0.000000000000000000, 1.000000000000000000, 0.000000000000000000 ) ) ;
#125409 = DIRECTION ( 'NONE',  ( 0.000000000000000000, 0.000000000000000000, 1.000000000000000000 ) ) ;
#125410 = CARTESIAN_POINT ( 'NONE',  ( -6.050000000000018474, 2.500000000000000000, 2.411473670974873862 ) ) ;
#125411 = CONICAL_SURFACE ( 'NONE', #12530, 0.1000000000000002554, 0.003490658503988666988 ) ;
#125412 = VERTEX_POINT ( 'NONE', #10469 ) ;
#125413 = ORIENTED_EDGE ( 'NONE', *, *, #105605, .F. ) ;
#125414 = ORIENTED_EDGE ( 'NONE', *, *, #8200, .T. ) ;
#125415 = EDGE_LOOP ( 'NONE', ( #125772, #33862 ) ) ;
#125416 = ORIENTED_EDGE ( 'NONE', *, *, #82060, .T. ) ;
#125417 = CARTESIAN_POINT ( 'NONE',  ( 1.899999999999949507, 12.50000000000000000, 4.611443907251934426 ) ) ;
#125418 = FACE_OUTER_BOUND ( 'NONE', #112029, .T. ) ;
#125419 = VERTEX_POINT ( 'NONE', #70050 ) ;
#125420 = FACE_BOUND ( 'NONE', #87042, .T. ) ;
#125421 = CARTESIAN_POINT ( 'NONE',  ( -14.54999999999998472, 2.500000000000000000, 2.165063509461101265 ) ) ;
#125423 = AXIS2_PLACEMENT_3D ( 'NONE', #16368, #96880, #56310 ) ;
#125422 = VECTOR ( 'NONE', #22501, 1000.000000000000000 ) ;
#125424 = EDGE_CURVE ( 'NONE', #27855, #50402, #30785, .T. ) ;
#125425 = DIRECTION ( 'NONE',  ( -0.000000000000000000, -1.000000000000000000, -0.000000000000000000 ) ) ;
#125426 = EDGE_CURVE ( 'NONE', #81351, #90210, #52768, .T. ) ;
#125427 = ORIENTED_EDGE ( 'NONE', *, *, #52420, .T. ) ;
#125428 = CARTESIAN_POINT ( 'NONE',  ( 4.999999999999933387, 2.500000000000000000, 5.122947341949749323 ) ) ;
#125429 = FACE_OUTER_BOUND ( 'NONE', #58518, .T. ) ;
#125430 = DIRECTION ( 'NONE',  ( -0.000000000000000000, -1.000000000000000000, -0.000000000000000000 ) ) ;
#125431 = EDGE_LOOP ( 'NONE', ( #44597, #82363 ) ) ;
#125432 = DIRECTION ( 'NONE',  ( 0.000000000000000000, 0.000000000000000000, 1.000000000000000000 ) ) ;
#125433 = VERTEX_POINT ( 'NONE', #81160 ) ;
#125434 = VERTEX_POINT ( 'NONE', #20944 ) ;
#125435 = EDGE_LOOP ( 'NONE', ( #42145, #115299 ) ) ;
#125436 = CARTESIAN_POINT ( 'NONE',  ( -2.100000000000033396, 2.500000000000000000, -3.537306695894649966 ) ) ;
#125437 = CARTESIAN_POINT ( 'NONE',  ( -5.000000000000023093, 2.500000000000000000, 0.7928203230275495672 ) ) ;
#125438 = CARTESIAN_POINT ( 'NONE',  ( 1.899999999999951283, 2.500000000000000000, -4.676537180435977881 ) ) ;
#125439 = ORIENTED_EDGE ( 'NONE', *, *, #7098, .F. ) ;
#125440 = DIRECTION ( 'NONE',  ( 0.000000000000000000, 0.000000000000000000, 1.000000000000000000 ) ) ;
#125441 = PLANE ( 'NONE',  #5206 ) ;
#125442 = AXIS2_PLACEMENT_3D ( 'NONE', #125282, #114804, #25784 ) ;
#125443 = DIRECTION ( 'NONE',  ( 0.000000000000000000, -0.9999939076577903929, 0.003490651415223739937 ) ) ;
#125444 = CARTESIAN_POINT ( 'NONE',  ( 184.5312500006828031, 9.429780353434619030E-16, -7.700000000000000178 ) ) ;
#125445 = DIRECTION ( 'NONE',  ( 0.000000000000000000, 0.000000000000000000, -1.000000000000000000 ) ) ;
#125446 = CARTESIAN_POINT ( 'NONE',  ( -12.49999999999999289, 12.50000000000000000, -0.6928203230275500335 ) ) ;
#125447 = ORIENTED_EDGE ( 'NONE', *, *, #86523, .F. ) ;
#125448 = CARTESIAN_POINT ( 'NONE',  ( 15.79999999999989058, 2.500000000000000000, -2.385244779468109755E-15 ) ) ;
#125449 = AXIS2_PLACEMENT_3D ( 'NONE', #63399, #94789, #93503 ) ;
#125450 = VERTEX_POINT ( 'NONE', #20302 ) ;
#125451 = ORIENTED_EDGE ( 'NONE', *, *, #117460, .T. ) ;
#125452 = CARTESIAN_POINT ( 'NONE',  ( 13.74999999999989875, 2.500000000000000000, 1.572243186433545548 ) ) ;
#125453 = CARTESIAN_POINT ( 'NONE',  ( 12.04999999999990479, 12.50000000000000000, 2.165063509461097713 ) ) ;
#125454 = FACE_OUTER_BOUND ( 'NONE', #64925, .T. ) ;
#125455 = AXIS2_PLACEMENT_3D ( 'NONE', #115902, #15760, #19474 ) ;
#125456 = ORIENTED_EDGE ( 'NONE', *, *, #70579, .F. ) ;
#125457 = ORIENTED_EDGE ( 'NONE', *, *, #32754, .T. ) ;
#125459 = ADVANCED_FACE ( 'NONE', ( #70688 ), #60867, .T. ) ;
#125458 = AXIS2_PLACEMENT_3D ( 'NONE', #126336, #105405, #106681 ) ;
#125460 = DIRECTION ( 'NONE',  ( 0.000000000000000000, 0.000000000000000000, 1.000000000000000000 ) ) ;
#125461 = CONICAL_SURFACE ( 'NONE', #110790, 0.09999999999999982514, 0.003490658503988666988 ) ;
#125462 = DIRECTION ( 'NONE',  ( -0.000000000000000000, 1.000000000000000000, -0.000000000000000000 ) ) ;
#125463 = DIRECTION ( 'NONE',  ( 0.000000000000000000, 0.000000000000000000, 1.000000000000000000 ) ) ;
#125464 = ORIENTED_EDGE ( 'NONE', *, *, #14129, .F. ) ;
#125465 = VERTEX_POINT ( 'NONE', #90308 ) ;
#125466 = FACE_OUTER_BOUND ( 'NONE', #89844, .T. ) ;
#125467 = AXIS2_PLACEMENT_3D ( 'NONE', #110574, #20262, #60210 ) ;
#125468 = VERTEX_POINT ( 'NONE', #649 ) ;
#125469 = DIRECTION ( 'NONE',  ( 0.000000000000000000, 0.000000000000000000, 1.000000000000000000 ) ) ;
#125470 = FACE_OUTER_BOUND ( 'NONE', #18219, .T. ) ;
#125471 = EDGE_LOOP ( 'NONE', ( #52908, #57803, #92770, #56181 ) ) ;
#125472 = DIRECTION ( 'NONE',  ( -4.274815082592931898E-19, -0.9999939076577903929, -0.003490651415223739937 ) ) ;
#125473 = DIRECTION ( 'NONE',  ( -4.274815082592931898E-19, -0.9999939076577903929, -0.003490651415223739937 ) ) ;
#125474 = CONICAL_SURFACE ( 'NONE', #81, 0.1000000000000000472, 0.003490658503988666988 ) ;
#125475 = DIRECTION ( 'NONE',  ( 0.000000000000000000, 0.000000000000000000, 1.000000000000000000 ) ) ;
#125476 = EDGE_CURVE ( 'NONE', #35640, #71388, #6774, .T. ) ;
#125477 = EDGE_CURVE ( 'NONE', #9409, #85421, #8843, .T. ) ;
#125478 = DIRECTION ( 'NONE',  ( -0.000000000000000000, -1.000000000000000000, -0.000000000000000000 ) ) ;
#125479 = VERTEX_POINT ( 'NONE', #92923 ) ;
#125480 = PLANE ( 'NONE',  #96838 ) ;
#125481 = DIRECTION ( 'NONE',  ( 1.000000000000000000, -0.000000000000000000, -0.000000000000000000 ) ) ;
#125482 = ORIENTED_EDGE ( 'NONE', *, *, #4632, .F. ) ;
#125483 = SHAPE_REPRESENTATION ( 'Internal PCBA Controller Module', ( #108296 ), #106243 ) ;
#125484 = EDGE_LOOP ( 'NONE', ( #65161, #23710, #111729, #35900 ) ) ;
#125485 = EDGE_CURVE ( 'NONE', #7764, #111299, #112559, .T. ) ;
#125486 = CARTESIAN_POINT ( 'NONE',  ( 184.8385416670080872, 6.551208109652274736, 3.782341765625001351 ) ) ;
#125487 = DIRECTION ( 'NONE',  ( 0.000000000000000000, 0.000000000000000000, 1.000000000000000000 ) ) ;
#125488 = DIRECTION ( 'NONE',  ( -0.000000000000000000, 1.000000000000000000, -0.000000000000000000 ) ) ;
#125489 = CARTESIAN_POINT ( 'NONE',  ( 14.99999999999989342, 12.50000000000000000, -0.6277270498435166823 ) ) ;
#125490 = CARTESIAN_POINT ( 'NONE',  ( -12.49999999999999467, 2.500000000000000000, 0.7928203230275536750 ) ) ;
#125491 = CARTESIAN_POINT ( 'NONE',  ( 10.39999999999991154, 2.500000000000000000, -5.022947341949754119 ) ) ;
#125492 = DIRECTION ( 'NONE',  ( 0.000000000000000000, 0.000000000000000000, -1.000000000000000000 ) ) ;
#125493 = PLANE ( 'NONE',  #95047 ) ;
#125494 = DIRECTION ( 'NONE',  ( 0.000000000000000000, 0.000000000000000000, 1.000000000000000000 ) ) ;
#125495 = CIRCLE ( 'NONE', #110822, 0.06509327318403745899 ) ;
#125496 = CONICAL_SURFACE ( 'NONE', #56535, 0.1000000000000000472, 0.003490658503988666988 ) ;
#125497 = FACE_OUTER_BOUND ( 'NONE', #32956, .T. ) ;
#125498 = VERTEX_POINT ( 'NONE', #81781 ) ;
#125500 = CIRCLE ( 'NONE', #41897, 0.1000000000000002554 ) ;
#125499 = AXIS2_PLACEMENT_3D ( 'NONE', #69655, #108920, #111512 ) ;
#125501 = ORIENTED_EDGE ( 'NONE', *, *, #36045, .T. ) ;
#125502 = VERTEX_POINT ( 'NONE', #101443 ) ;
#125503 = CARTESIAN_POINT ( 'NONE',  ( 8.149999999999923972, 2.500000000000000000, -6.841600689897077814 ) ) ;
#125504 = DIRECTION ( 'NONE',  ( 0.000000000000000000, -0.9999939076577903929, 0.003490651415223739937 ) ) ;
#125505 = CARTESIAN_POINT ( 'NONE',  ( 187.5000000000000000, 0.000000000000000000, -8.699999999999999289 ) ) ;
#125506 = EDGE_LOOP ( 'NONE', ( #80555, #97938, #84940, #41457 ) ) ;
#125507 = CARTESIAN_POINT ( 'NONE',  ( -5.850000000000019185, 2.500000000000000000, 6.595190528383296780 ) ) ;
#125508 = ADVANCED_FACE ( 'NONE', ( #51068 ), #54820, .T. ) ;
#125509 = DIRECTION ( 'NONE',  ( 0.000000000000000000, 0.000000000000000000, -1.000000000000000000 ) ) ;
#125511 = ORIENTED_EDGE ( 'NONE', *, *, #68865, .F. ) ;
#125510 = LINE ( 'NONE', #35853, #129612 ) ;
#125512 = EDGE_CURVE ( 'NONE', #69417, #63398, #21376, .T. ) ;
#125513 = EDGE_CURVE ( 'NONE', #119556, #18789, #125921, .T. ) ;
#125514 = CARTESIAN_POINT ( 'NONE',  ( 9.199999999999915801, 2.500000000000000000, 4.330127018922196314 ) ) ;
#125515 = ORIENTED_EDGE ( 'NONE', *, *, #41680, .T. ) ;
#125516 = ORIENTED_EDGE ( 'NONE', *, *, #20970, .F. ) ;
#125517 = EDGE_LOOP ( 'NONE', ( #48335, #111396 ) ) ;
#125518 = ORIENTED_EDGE ( 'NONE', *, *, #85313, .F. ) ;
#125519 = CARTESIAN_POINT ( 'NONE',  ( -9.550000000000002487, 2.500000000000000000, 6.395190528383296602 ) ) ;
#125520 = EDGE_CURVE ( 'NONE', #77155, #101605, #100779, .T. ) ;
#125521 = EDGE_CURVE ( 'NONE', #31027, #64400, #63239, .T. ) ;
#125522 = EDGE_CURVE ( 'NONE', #19669, #7901, #22894, .T. ) ;
#125523 = CARTESIAN_POINT ( 'NONE',  ( 9.349999999999916156, 12.50000000000000000, -2.511473670974877948 ) ) ;
#125524 = CARTESIAN_POINT ( 'NONE',  ( -11.84999999999999787, 2.500000000000000000, -6.148780366869522673 ) ) ;
#125525 = CARTESIAN_POINT ( 'NONE',  ( -4.150000000000025224, 2.500000000000000000, -1.572243186433550211 ) ) ;
#125526 = AXIS2_PLACEMENT_3D ( 'NONE', #79315, #69462, #59686 ) ;
#125527 = VERTEX_POINT ( 'NONE', #92249 ) ;
#125528 = EDGE_CURVE ( 'NONE', #79994, #30131, #77804, .T. ) ;
#125529 = DIRECTION ( 'NONE',  ( 0.000000000000000000, 1.000000000000000000, 0.000000000000000000 ) ) ;
#125530 = VERTEX_POINT ( 'NONE', #41890 ) ;
#125531 = CARTESIAN_POINT ( 'NONE',  ( -4.077611073288324453E-14, 12.50000000000000000, -5.088040615133791356 ) ) ;
#125532 = DIRECTION ( 'NONE',  ( 0.000000000000000000, 0.000000000000000000, -1.000000000000000000 ) ) ;
#125533 = DIRECTION ( 'NONE',  ( -0.000000000000000000, -1.000000000000000000, -0.000000000000000000 ) ) ;
#125534 = CARTESIAN_POINT ( 'NONE',  ( 18.20334136263782199, -2.532871263996936406, 4.817802756298863898 ) ) ;
#125536 = ADVANCED_FACE ( 'NONE', ( #82462 ), #96667, .T. ) ;
#125535 = AXIS2_PLACEMENT_3D ( 'NONE', #54682, #3040, #103163 ) ;
#125537 = EDGE_LOOP ( 'NONE', ( #55075, #126118, #7292, #17407 ) ) ;
#125538 = VERTEX_POINT ( 'NONE', #102707 ) ;
#125539 = EDGE_LOOP ( 'NONE', ( #47317, #117254, #125087, #85792 ) ) ;
#125540 = CARTESIAN_POINT ( 'NONE',  ( -2.300000000000033573, 2.500000000000000000, -3.883716857408426648 ) ) ;
#125541 = DIRECTION ( 'NONE',  ( 0.000000000000000000, -0.000000000000000000, 1.000000000000000000 ) ) ;
#125542 = FACE_OUTER_BOUND ( 'NONE', #55241, .T. ) ;
#125543 = FACE_BOUND ( 'NONE', #27472, .T. ) ;
#125544 = DIRECTION ( 'NONE',  ( 0.000000000000000000, -0.9999939076577903929, 0.003490651415223739937 ) ) ;
#125545 = CARTESIAN_POINT ( 'NONE',  ( -7.500000000000001776, -1.500000000000000000, 1.734723475976807094E-15 ) ) ;
#125546 = CARTESIAN_POINT ( 'NONE',  ( -5.650000000000019895, 12.50000000000000000, 1.818653347947321475 ) ) ;
#125547 = CARTESIAN_POINT ( 'NONE',  ( 187.5000000000000000, 0.000000000000000000, 0.000000000000000000 ) ) ;
#125548 = CONICAL_SURFACE ( 'NONE', #52396, 0.1000000000000000056, 0.003490658503988666988 ) ;
#125549 = CARTESIAN_POINT ( 'NONE',  ( 185.1302083336747728, -4.367472073101514418, -7.564683531250002702 ) ) ;
#125550 = DIRECTION ( 'NONE',  ( -4.274815082592931898E-19, -0.9999939076577903929, -0.003490651415223739937 ) ) ;
#125551 = CARTESIAN_POINT ( 'NONE',  ( 11.44999999999990514, 12.50000000000000000, 2.576566944158910744 ) ) ;
#125552 = AXIS2_PLACEMENT_3D ( 'NONE', #14915, #75167, #67234 ) ;
#125553 = FACE_OUTER_BOUND ( 'NONE', #18102, .T. ) ;
#125554 = ORIENTED_EDGE ( 'NONE', *, *, #21382, .F. ) ;
#125555 = CIRCLE ( 'NONE', #35694, 0.09999999999999982514 ) ;
#125556 = ORIENTED_EDGE ( 'NONE', *, *, #24324, .T. ) ;
#125557 = EDGE_LOOP ( 'NONE', ( #91959, #54112, #46242, #62986 ) ) ;
#125558 = ORIENTED_EDGE ( 'NONE', *, *, #55045, .T. ) ;
#125559 = DIRECTION ( 'NONE',  ( 0.000000000000000000, 0.000000000000000000, 1.000000000000000000 ) ) ;
#125560 = FACE_BOUND ( 'NONE', #15097, .T. ) ;
#125561 = CARTESIAN_POINT ( 'NONE',  ( 1.699999999999951994, 2.500000000000000000, -4.430127018922202176 ) ) ;
#125562 = ADVANCED_FACE ( 'NONE', ( #43184 ), #83100, .T. ) ;
#125563 = EDGE_LOOP ( 'NONE', ( #58605, #16598 ) ) ;
#125564 = DIRECTION ( 'NONE',  ( -0.000000000000000000, -1.000000000000000000, -0.000000000000000000 ) ) ;
#125565 = DIRECTION ( 'NONE',  ( 0.000000000000000000, 0.000000000000000000, 1.000000000000000000 ) ) ;
#125566 = ORIENTED_EDGE ( 'NONE', *, *, #85848, .F. ) ;
#125567 = CARTESIAN_POINT ( 'NONE',  ( -14.14999999999998614, 2.500000000000000000, -2.757883832488651876 ) ) ;
#125568 = FACE_OUTER_BOUND ( 'NONE', #75049, .T. ) ;
#125569 = EDGE_CURVE ( 'NONE', #108133, #126539, #23520, .T. ) ;
#125570 = AXIS2_PLACEMENT_3D ( 'NONE', #43241, #43883, #123073 ) ;
#125571 = ORIENTED_EDGE ( 'NONE', *, *, #121700, .T. ) ;
#125572 = CONICAL_SURFACE ( 'NONE', #54484, 0.09999999999999982514, 0.003490658503988666988 ) ;
#125573 = CARTESIAN_POINT ( 'NONE',  ( -11.25000000000000000, 2.500000000000000000, 2.857883832488649301 ) ) ;
#125574 = CIRCLE ( 'NONE', #44112, 0.1000000000000000056 ) ;
#125575 = CARTESIAN_POINT ( 'NONE',  ( -5.450000000000019718, 12.50000000000000000, 6.560283801567334372 ) ) ;
#125576 = EDGE_LOOP ( 'NONE', ( #26488, #78472 ) ) ;
#125577 = DIRECTION ( 'NONE',  ( 0.000000000000000000, 0.000000000000000000, -1.000000000000000000 ) ) ;
#125578 = VECTOR ( 'NONE', #68207, 1000.000000000000000 ) ;
#125579 = DIRECTION ( 'NONE',  ( -0.000000000000000000, -1.000000000000000000, -0.000000000000000000 ) ) ;
#125580 = ORIENTED_EDGE ( 'NONE', *, *, #15560, .T. ) ;
#125581 = DIRECTION ( 'NONE',  ( 0.000000000000000000, 1.000000000000000000, 0.000000000000000000 ) ) ;
#125582 = EDGE_LOOP ( 'NONE', ( #95200, #79495 ) ) ;
#125583 = CIRCLE ( 'NONE', #90076, 0.06509327318403745899 ) ;
#125584 = ORIENTED_EDGE ( 'NONE', *, *, #38304, .T. ) ;
#125585 = DIRECTION ( 'NONE',  ( 0.000000000000000000, 0.000000000000000000, -1.000000000000000000 ) ) ;
#125586 = VERTEX_POINT ( 'NONE', #104020 ) ;
#125587 = LINE ( 'NONE', #94210, #86708 ) ;
#125588 = DIRECTION ( 'NONE',  ( -0.000000000000000000, -1.000000000000000000, -0.000000000000000000 ) ) ;
#125589 = ORIENTED_EDGE ( 'NONE', *, *, #23639, .F. ) ;
#125590 = CARTESIAN_POINT ( 'NONE',  ( 1.649999999999949729, 12.50000000000000000, 5.802370205355744659 ) ) ;
#125591 = DIRECTION ( 'NONE',  ( 0.000000000000000000, -0.9999939076577903929, 0.003490651415223739937 ) ) ;
#125592 = DIRECTION ( 'NONE',  ( -0.000000000000000000, -1.000000000000000000, -0.000000000000000000 ) ) ;
#125593 = DIRECTION ( 'NONE',  ( 0.000000000000000000, 0.000000000000000000, 1.000000000000000000 ) ) ;
#125594 = DIRECTION ( 'NONE',  ( 0.000000000000000000, 0.000000000000000000, 1.000000000000000000 ) ) ;
#125595 = CARTESIAN_POINT ( 'NONE',  ( 17.48308156489505549, 2.102418598454959486, -4.293689242909686676 ) ) ;
#125596 = VERTEX_POINT ( 'NONE', #26108 ) ;
#125598 = VERTEX_POINT ( 'NONE', #113179 ) ;
#125597 = EDGE_CURVE ( 'NONE', #97446, #11600, #533, .T. ) ;
#125599 = AXIS2_PLACEMENT_3D ( 'NONE', #23532, #44467, #55583 ) ;
#125600 = FACE_OUTER_BOUND ( 'NONE', #46884, .T. ) ;
#125601 = CARTESIAN_POINT ( 'NONE',  ( -1.050000000000037792, 2.500000000000000000, 1.818653347947321475 ) ) ;
#125602 = CARTESIAN_POINT ( 'NONE',  ( -14.34999999999998543, 2.500000000000000000, 2.511473670974877503 ) ) ;
#125604 = ORIENTED_EDGE ( 'NONE', *, *, #41554, .F. ) ;
#125603 = ORIENTED_EDGE ( 'NONE', *, *, #75871, .F. ) ;
#125605 = EDGE_LOOP ( 'NONE', ( #21444, #115281, #53811, #62690 ) ) ;
#125606 = ADVANCED_FACE ( 'NONE', ( #105948 ), #45108, .T. ) ;
#125607 = LINE ( 'NONE', #16918, #114885 ) ;
#125608 = AXIS2_PLACEMENT_3D ( 'NONE', #121636, #92174, #109902 ) ;
#125610 = ADVANCED_FACE ( 'NONE', ( #104644 ), #27621, .T. ) ;
#125609 = DIRECTION ( 'NONE',  ( -0.000000000000000000, -1.000000000000000000, -0.000000000000000000 ) ) ;
#125611 = DIRECTION ( 'NONE',  ( 0.000000000000000000, 1.000000000000000000, 0.000000000000000000 ) ) ;
#125612 = DIRECTION ( 'NONE',  ( 1.000000000000000000, 0.000000000000000000, 0.000000000000000000 ) ) ;
#125613 = FACE_OUTER_BOUND ( 'NONE', #75371, .T. ) ;
#125614 = CARTESIAN_POINT ( 'NONE',  ( -10.40000000000000391, 12.50000000000000000, -3.572213422710607933 ) ) ;
#125615 = FACE_OUTER_BOUND ( 'NONE', #71780, .T. ) ;
#125616 = DIRECTION ( 'NONE',  ( 0.000000000000000000, 0.000000000000000000, 1.000000000000000000 ) ) ;
#125617 = LINE ( 'NONE', #117724, #46717 ) ;
#125618 = ADVANCED_FACE ( 'NONE', ( #44451 ), #56957, .T. ) ;
#125619 = ADVANCED_FACE ( 'NONE', ( #86290 ), #53629, .T. ) ;
#125621 = CONICAL_SURFACE ( 'NONE', #19004, 0.09999999999999982514, 0.003490658503988666988 ) ;
#125620 = CARTESIAN_POINT ( 'NONE',  ( 6.449999999999930012, 2.500000000000000000, 1.918653347947321564 ) ) ;
#125622 = CONICAL_SURFACE ( 'NONE', #21072, 0.1000000000000002554, 0.003490658503988666988 ) ;
#125623 = ORIENTED_EDGE ( 'NONE', *, *, #29583, .F. ) ;
#125624 = ADVANCED_FACE ( 'NONE', ( #65367 ), #48581, .T. ) ;
#125625 = DIRECTION ( 'NONE',  ( 0.000000000000000000, 0.000000000000000000, 1.000000000000000000 ) ) ;
#125626 = VERTEX_POINT ( 'NONE', #93552 ) ;
#125627 = EDGE_LOOP ( 'NONE', ( #107488, #123149 ) ) ;
#125628 = EDGE_CURVE ( 'NONE', #85037, #102865, #59045, .T. ) ;
#125629 = CARTESIAN_POINT ( 'NONE',  ( 6.899999999999926636, 2.500000000000000000, 0.3464101615137736845 ) ) ;
#125630 = FACE_OUTER_BOUND ( 'NONE', #71303, .T. ) ;
#125631 = CARTESIAN_POINT ( 'NONE',  ( -6.250000000000021316, 2.500000000000000000, -1.472243186433550122 ) ) ;
#125632 = CONICAL_SURFACE ( 'NONE', #113027, 0.1000000000000002554, 0.003490658503988666988 ) ;
#125633 = DIRECTION ( 'NONE',  ( 0.000000000000000000, -0.9999939076577903929, 0.003490651415223739937 ) ) ;
#125634 = CIRCLE ( 'NONE', #39898, 0.09999999999999982514 ) ;
#125635 = DIRECTION ( 'NONE',  ( -0.000000000000000000, -1.000000000000000000, -0.000000000000000000 ) ) ;
#125636 = DIRECTION ( 'NONE',  ( 0.000000000000000000, 1.000000000000000000, 0.000000000000000000 ) ) ;
#125637 = CARTESIAN_POINT ( 'NONE',  ( 11.84999999999990727, 2.500000000000000000, -1.918653347947326004 ) ) ;
#125638 = ORIENTED_EDGE ( 'NONE', *, *, #22311, .T. ) ;
#125639 = CARTESIAN_POINT ( 'NONE',  ( 10.44999999999991047, 2.500000000000000000, 2.165063509461097713 ) ) ;
#125640 = AXIS2_PLACEMENT_3D ( 'NONE', #123450, #93361, #42329 ) ;
#125641 = PLANE ( 'NONE',  #87494 ) ;
#125642 = EDGE_LOOP ( 'NONE', ( #32604, #110432, #18, #95057 ) ) ;
#125643 = EDGE_LOOP ( 'NONE', ( #15552, #9270, #89974, #32865 ) ) ;
#125644 = AXIS2_PLACEMENT_3D ( 'NONE', #38411, #97311, #78333 ) ;
#125645 = VERTEX_POINT ( 'NONE', #84376 ) ;
#125646 = ORIENTED_EDGE ( 'NONE', *, *, #94919, .T. ) ;
#125647 = DIRECTION ( 'NONE',  ( 0.000000000000000000, 1.000000000000000000, 0.000000000000000000 ) ) ;
#125648 = DIRECTION ( 'NONE',  ( 0.000000000000000000, 0.000000000000000000, -1.000000000000000000 ) ) ;
#125649 = PLANE ( 'NONE',  #12979 ) ;
#125650 = CARTESIAN_POINT ( 'NONE',  ( 0.8499999999999553468, 2.500000000000000000, 2.065063509461097624 ) ) ;
#125651 = DIRECTION ( 'NONE',  ( -4.274815082592931898E-19, -0.9999939076577903929, -0.003490651415223739937 ) ) ;
#125652 = ORIENTED_EDGE ( 'NONE', *, *, #50639, .T. ) ;
#125653 = DIRECTION ( 'NONE',  ( 0.000000000000000000, 1.000000000000000000, 0.000000000000000000 ) ) ;
#125654 = ADVANCED_FACE ( 'NONE', ( #14951 ), #124303, .T. ) ;
#125655 = DIRECTION ( 'NONE',  ( 0.000000000000000000, -0.9999939076577903929, 0.003490651415223739937 ) ) ;
#125656 = EDGE_LOOP ( 'NONE', ( #89548, #11354, #102663, #38504 ) ) ;
#125657 = VERTEX_POINT ( 'NONE', #74554 ) ;
#125658 = EDGE_LOOP ( 'NONE', ( #45519, #119858, #51505, #126976 ) ) ;
#125660 = EDGE_CURVE ( 'NONE', #43024, #88967, #73689, .T. ) ;
#125659 = AXIS2_PLACEMENT_3D ( 'NONE', #96172, #94897, #77192 ) ;
#125661 = DIRECTION ( 'NONE',  ( 0.000000000000000000, 0.000000000000000000, 1.000000000000000000 ) ) ;
#125662 = AXIS2_PLACEMENT_3D ( 'NONE', #110676, #70129, #50473 ) ;
#125663 = ADVANCED_FACE ( 'NONE', ( #96122 ), #42317, .T. ) ;
#125664 = ADVANCED_FACE ( 'NONE', ( #94842 ), #33998, .T. ) ;
#125665 = EDGE_CURVE ( 'NONE', #13889, #127971, #2576, .T. ) ;
#125666 = CARTESIAN_POINT ( 'NONE',  ( 165.4999999999999716, 6.123233995736767268E-17, -1.500000000000000000 ) ) ;
#125667 = CARTESIAN_POINT ( 'NONE',  ( -10.85000000000000142, 2.500000000000000000, -6.595190528383298556 ) ) ;
#125668 = CIRCLE ( 'NONE', #69235, 0.1000000000000002554 ) ;
#125669 = CIRCLE ( 'NONE', #12796, 0.09999999999999982514 ) ;
#125670 = EDGE_CURVE ( 'NONE', #74953, #19040, #83735, .T. ) ;
#125671 = ORIENTED_EDGE ( 'NONE', *, *, #97604, .F. ) ;
#125672 = DIRECTION ( 'NONE',  ( 0.000000000000000000, 0.000000000000000000, 1.000000000000000000 ) ) ;
#125673 = FACE_OUTER_BOUND ( 'NONE', #19370, .T. ) ;
#125674 = CARTESIAN_POINT ( 'NONE',  ( -6.250000000000019540, 2.500000000000000000, -2.857883832488653741 ) ) ;
#125675 = CARTESIAN_POINT ( 'NONE',  ( 130.5000000000000000, 0.5000000000000000000, -7.500000000000001776 ) ) ;
#125676 = CARTESIAN_POINT ( 'NONE',  ( 8.149999999999920419, 2.500000000000000000, -1.818653347947325916 ) ) ;
#125677 = EDGE_CURVE ( 'NONE', #101819, #110619, #109198, .T. ) ;
#125678 = VERTEX_POINT ( 'NONE', #103377 ) ;
#125679 = ADVANCED_FACE ( 'NONE', ( #16880 ), #77759, .T. ) ;
#125680 = DIRECTION ( 'NONE',  ( 0.000000000000000000, 0.000000000000000000, -1.000000000000000000 ) ) ;
#125681 = VERTEX_POINT ( 'NONE', #8381 ) ;
#125682 = VERTEX_POINT ( 'NONE', #29337 ) ;
#125683 = EDGE_LOOP ( 'NONE', ( #30821, #55489, #33397, #120945 ) ) ;
#125684 = CARTESIAN_POINT ( 'NONE',  ( -9.800000000000006040, 2.500000000000000000, 4.676537180435972552 ) ) ;
#125685 = FACE_BOUND ( 'NONE', #92714, .T. ) ;
#125686 = CARTESIAN_POINT ( 'NONE',  ( -3.350000000000028511, 12.50000000000000000, -2.922977105672691422 ) ) ;
#125687 = DIRECTION ( 'NONE',  ( -0.000000000000000000, 1.000000000000000000, -0.000000000000000000 ) ) ;
#125688 = DIRECTION ( 'NONE',  ( 0.000000000000000000, 0.000000000000000000, -1.000000000000000000 ) ) ;
#125689 = ORIENTED_EDGE ( 'NONE', *, *, #14711, .T. ) ;
#125690 = DIRECTION ( 'NONE',  ( -0.000000000000000000, 1.000000000000000000, -0.000000000000000000 ) ) ;
#125691 = DIRECTION ( 'NONE',  ( 0.000000000000000000, -0.9999939076577903929, 0.003490651415223739937 ) ) ;
#125692 = CARTESIAN_POINT ( 'NONE',  ( -7.900000000000011013, 12.50000000000000000, 3.637306695894644726 ) ) ;
#125693 = DIRECTION ( 'NONE',  ( 0.000000000000000000, 1.000000000000000000, 0.000000000000000000 ) ) ;
#125694 = ORIENTED_EDGE ( 'NONE', *, *, #52619, .F. ) ;
#125695 = CONICAL_SURFACE ( 'NONE', #29570, 0.09999999999999982514, 0.003490658503988666988 ) ;
#125696 = CARTESIAN_POINT ( 'NONE',  ( 1.849999999999949019, 12.50000000000000000, 6.776507416713035248 ) ) ;
#125697 = DIRECTION ( 'NONE',  ( -0.000000000000000000, -1.000000000000000000, -0.000000000000000000 ) ) ;
#125698 = EDGE_LOOP ( 'NONE', ( #67776, #59796 ) ) ;
#125699 = DIRECTION ( 'NONE',  ( 0.000000000000000000, -0.000000000000000000, 1.000000000000000000 ) ) ;
#125700 = FACE_BOUND ( 'NONE', #99058, .T. ) ;
#125701 = CIRCLE ( 'NONE', #54687, 0.06509327318403745899 ) ;
#125702 = DIRECTION ( 'NONE',  ( 0.000000000000000000, 0.000000000000000000, -1.000000000000000000 ) ) ;
#125703 = AXIS2_PLACEMENT_3D ( 'NONE', #88952, #78507, #28751 ) ;
#125704 = VERTEX_POINT ( 'NONE', #99363 ) ;
#125705 = PLANE ( 'NONE',  #65361 ) ;
#125706 = DIRECTION ( 'NONE',  ( -0.000000000000000000, 1.000000000000000000, -0.000000000000000000 ) ) ;
#125707 = EDGE_LOOP ( 'NONE', ( #71985, #41816, #107440, #91039 ) ) ;
#125708 = VERTEX_POINT ( 'NONE', #107234 ) ;
#125709 = APPLICATION_CONTEXT ( 'automotive_design' ) ;
#125710 = CARTESIAN_POINT ( 'NONE',  ( 186.4166666666666856, 6.668395609140176816, 3.850000000000000977 ) ) ;
#125711 = EDGE_LOOP ( 'NONE', ( #58321, #32106 ) ) ;
#125713 = CARTESIAN_POINT ( 'NONE',  ( 185.5468750003414300, -8.734944146203032389, -1.604583208406767949E-15 ) ) ;
#125712 = VECTOR ( 'NONE', #35867, 1000.000000000000000 ) ;
#125714 = DIRECTION ( 'NONE',  ( 0.000000000000000000, -0.000000000000000000, 1.000000000000000000 ) ) ;
#125715 = ADVANCED_FACE ( 'NONE', ( #118343 ), #7083, .T. ) ;
#125716 = DIRECTION ( 'NONE',  ( 0.000000000000000000, 0.000000000000000000, -1.000000000000000000 ) ) ;
#125717 = CIRCLE ( 'NONE', #65083, 0.09999999999999982514 ) ;
#125718 = LINE ( 'NONE', #104168, #75994 ) ;
#125719 = CARTESIAN_POINT ( 'NONE',  ( -6.650000000000018119, 12.50000000000000000, -2.165063509461101710 ) ) ;
#125720 = AXIS2_PLACEMENT_3D ( 'NONE', #92552, #72920, #23164 ) ;
#125721 = ORIENTED_EDGE ( 'NONE', *, *, #98551, .F. ) ;
#125722 = ORIENTED_EDGE ( 'NONE', *, *, #120009, .F. ) ;
#125723 = CARTESIAN_POINT ( 'NONE',  ( 1.249999999999988898, 12.50000000000000000, -6.495190528383302464 ) ) ;
#125724 = AXIS2_PLACEMENT_3D ( 'NONE', #127203, #60404, #98355 ) ;
#125725 = AXIS2_PLACEMENT_3D ( 'NONE', #80899, #40335, #90050 ) ;
#125726 = CARTESIAN_POINT ( 'NONE',  ( -4.150000000000024336, 2.500000000000000000, 2.265063509461097357 ) ) ;
#125727 = CARTESIAN_POINT ( 'NONE',  ( -8.150000000000012790, 12.50000000000000000, 2.511473670974873507 ) ) ;
#125728 = DIRECTION ( 'NONE',  ( 0.000000000000000000, 0.000000000000000000, -1.000000000000000000 ) ) ;
#125730 = ORIENTED_EDGE ( 'NONE', *, *, #86939, .T. ) ;
#125729 = EDGE_LOOP ( 'NONE', ( #46674, #47022 ) ) ;
#125731 = CARTESIAN_POINT ( 'NONE',  ( -8.550000000000014921, 2.500000000000000000, -6.148780366869520897 ) ) ;
#125732 = VERTEX_POINT ( 'NONE', #117674 ) ;
#125733 = DIRECTION ( 'NONE',  ( 0.000000000000000000, -0.000000000000000000, 1.000000000000000000 ) ) ;
#125734 = DIRECTION ( 'NONE',  ( 0.000000000000000000, 1.000000000000000000, 0.000000000000000000 ) ) ;
#125735 = EDGE_LOOP ( 'NONE', ( #50962, #34500, #118419, #50923 ) ) ;
#125736 = CARTESIAN_POINT ( 'NONE',  ( 5.199999999999937117, 12.50000000000000000, -4.676537180435978769 ) ) ;
#125737 = LINE ( 'NONE', #7253, #62007 ) ;
#125738 = DIRECTION ( 'NONE',  ( -0.000000000000000000, 1.000000000000000000, -0.000000000000000000 ) ) ;
#125739 = DIRECTION ( 'NONE',  ( 0.000000000000000000, 1.000000000000000000, 0.000000000000000000 ) ) ;
#125740 = DIRECTION ( 'NONE',  ( 0.000000000000000000, 0.000000000000000000, -1.000000000000000000 ) ) ;
#125741 = DIRECTION ( 'NONE',  ( -0.000000000000000000, -1.000000000000000000, -0.000000000000000000 ) ) ;
#125742 = CARTESIAN_POINT ( 'NONE',  ( -5.600000000000020073, 2.500000000000000000, 4.676537180435972552 ) ) ;
#125743 = DIRECTION ( 'NONE',  ( -0.000000000000000000, 1.000000000000000000, -0.000000000000000000 ) ) ;
#125744 = DIRECTION ( 'NONE',  ( -0.000000000000000000, 1.000000000000000000, -0.000000000000000000 ) ) ;
#125745 = ORIENTED_EDGE ( 'NONE', *, *, #54879, .T. ) ;
#125746 = ORIENTED_EDGE ( 'NONE', *, *, #94665, .F. ) ;
#125747 = DIRECTION ( 'NONE',  ( -0.000000000000000000, 1.000000000000000000, -0.000000000000000000 ) ) ;
#125748 = ORIENTED_EDGE ( 'NONE', *, *, #52839, .F. ) ;
#125749 = AXIS2_PLACEMENT_3D ( 'NONE', #127643, #97531, #7858 ) ;
#125750 = DIRECTION ( 'NONE',  ( 0.000000000000000000, 0.000000000000000000, 1.000000000000000000 ) ) ;
#125751 = AXIS2_PLACEMENT_3D ( 'NONE', #65278, #105211, #35833 ) ;
#125753 = ORIENTED_EDGE ( 'NONE', *, *, #18173, .T. ) ;
#125752 = VERTEX_POINT ( 'NONE', #49627 ) ;
#125754 = ORIENTED_EDGE ( 'NONE', *, *, #56730, .T. ) ;
#125755 = DIRECTION ( 'NONE',  ( 0.000000000000000000, -0.000000000000000000, 1.000000000000000000 ) ) ;
#125756 = ADVANCED_FACE ( 'NONE', ( #128178 ), #88350, .T. ) ;
#125757 = AXIS2_PLACEMENT_3D ( 'NONE', #123597, #111865, #102670 ) ;
#125758 = CARTESIAN_POINT ( 'NONE',  ( -5.850000000000022737, 12.50000000000000000, -6.560283801567339701 ) ) ;
#125759 = CIRCLE ( 'NONE', #96509, 0.09999999999999999167 ) ;
#125760 = DIRECTION ( 'NONE',  ( 0.000000000000000000, 0.000000000000000000, 1.000000000000000000 ) ) ;
#125761 = FACE_OUTER_BOUND ( 'NONE', #30123, .T. ) ;
#125762 = CIRCLE ( 'NONE', #27564, 0.06509327318403745899 ) ;
#125763 = CARTESIAN_POINT ( 'NONE',  ( -0.8500000000000386136, 12.50000000000000000, 7.122917578226811486 ) ) ;
#125764 = AXIS2_PLACEMENT_3D ( 'NONE', #63068, #94447, #4767 ) ;
#125765 = EDGE_CURVE ( 'NONE', #124238, #98747, #57501, .T. ) ;
#125766 = ORIENTED_EDGE ( 'NONE', *, *, #9047, .F. ) ;
#125767 = EDGE_CURVE ( 'NONE', #45092, #15933, #76498, .T. ) ;
#125768 = DIRECTION ( 'NONE',  ( -4.274815082592931898E-19, -0.9999939076577903929, -0.003490651415223739937 ) ) ;
#125770 = EDGE_LOOP ( 'NONE', ( #110284, #56015 ) ) ;
#125769 = CIRCLE ( 'NONE', #79816, 0.06509327318403745899 ) ;
#125771 = EDGE_LOOP ( 'NONE', ( #101788, #82119 ) ) ;
#125772 = ORIENTED_EDGE ( 'NONE', *, *, #65859, .T. ) ;
#125773 = ORIENTED_EDGE ( 'NONE', *, *, #42138, .F. ) ;
#125774 = ADVANCED_FACE ( 'NONE', ( #116398 ), #42421, .T. ) ;
#125776 = EDGE_CURVE ( 'NONE', #56169, #88605, #61187, .T. ) ;
#125775 = CARTESIAN_POINT ( 'NONE',  ( 3.099999999999943245, 2.500000000000000000, 3.983716857408420076 ) ) ;
#125778 = ORIENTED_EDGE ( 'NONE', *, *, #95048, .F. ) ;
#125777 = EDGE_CURVE ( 'NONE', #7618, #43527, #54911, .T. ) ;
#125779 = EDGE_LOOP ( 'NONE', ( #9333, #122204 ) ) ;
#125780 = ADVANCED_FACE ( 'NONE', ( #69230 ), #19402, .T. ) ;
#125781 = DIRECTION ( 'NONE',  ( 0.000000000000000000, 0.000000000000000000, -1.000000000000000000 ) ) ;
#125782 = CARTESIAN_POINT ( 'NONE',  ( 10.39999999999990976, 2.500000000000000000, 4.330127018922196314 ) ) ;
#125783 = PLANE ( 'NONE',  #67244 ) ;
#125784 = PLANE ( 'NONE',  #17832 ) ;
#125785 = B_SPLINE_CURVE_WITH_KNOTS ( 'NONE', 3,
 ( #85686, #35951, #127554, #85040, #117066, #75225, #37882, #65398, #26775, #86322, #37255, #16913 ),
 .UNSPECIFIED., .F., .F.,
 ( 4, 2, 2, 2, 2, 4 ),
 ( 8.673617379884035472E-19, 0.0006571239767409088736, 0.001314247953481816880, 0.002628495906963632892, 0.003942743860445448688, 0.005256991813927264917 ),
 .UNSPECIFIED. ) ;
#125786 = CARTESIAN_POINT ( 'NONE',  ( -7.100000000000018296, 12.50000000000000000, -2.385244779468109755E-15 ) ) ;
#125787 = ORIENTED_EDGE ( 'NONE', *, *, #2313, .F. ) ;
#125788 = ADVANCED_FACE ( 'NONE', ( #37223 ), #59145, .T. ) ;
#125789 = DIRECTION ( 'NONE',  ( 0.000000000000000000, 0.000000000000000000, -1.000000000000000000 ) ) ;
#125790 = AXIS2_PLACEMENT_3D ( 'NONE', #109744, #80932, #120845 ) ;
#125791 = AXIS2_PLACEMENT_3D ( 'NONE', #99587, #119857, #29547 ) ;
#125792 = VERTEX_POINT ( 'NONE', #88888 ) ;
#125793 = DIRECTION ( 'NONE',  ( -0.000000000000000000, -1.000000000000000000, -0.000000000000000000 ) ) ;
#125794 = ORIENTED_EDGE ( 'NONE', *, *, #122856, .F. ) ;
#125795 = DIRECTION ( 'NONE',  ( -0.000000000000000000, -1.000000000000000000, -0.000000000000000000 ) ) ;
#125796 = ORIENTED_EDGE ( 'NONE', *, *, #20049, .F. ) ;
#125797 = ORIENTED_EDGE ( 'NONE', *, *, #42034, .T. ) ;
#125798 = AXIS2_PLACEMENT_3D ( 'NONE', #48929, #88834, #128792 ) ;
#125799 = DIRECTION ( 'NONE',  ( 0.000000000000000000, -0.000000000000000000, 1.000000000000000000 ) ) ;
#125800 = CARTESIAN_POINT ( 'NONE',  ( -8.350000000000008527, 2.500000000000000000, 7.188010851410848723 ) ) ;
#125801 = CIRCLE ( 'NONE', #38088, 0.06509327318403745899 ) ;
#125802 = CIRCLE ( 'NONE', #2468, 0.06509327318403745899 ) ;
#125803 = DIRECTION ( 'NONE',  ( 1.000000000000000000, -0.000000000000000000, -0.000000000000000000 ) ) ;
#125804 = CIRCLE ( 'NONE', #86082, 0.1000000000000002554 ) ;
#125805 = AXIS2_PLACEMENT_3D ( 'NONE', #11938, #82634, #72808 ) ;
#125806 = CARTESIAN_POINT ( 'NONE',  ( 7.099999999999927702, 2.500000000000000000, -3.637306695894650055 ) ) ;
#125807 = CARTESIAN_POINT ( 'NONE',  ( -5.650000000000023448, 12.50000000000000000, -2.576566944158915184 ) ) ;
#125808 = ORIENTED_EDGE ( 'NONE', *, *, #22511, .F. ) ;
#125809 = DIRECTION ( 'NONE',  ( 0.000000000000000000, 1.000000000000000000, 0.000000000000000000 ) ) ;
#125810 = CARTESIAN_POINT ( 'NONE',  ( -11.24999999999999822, 2.500000000000000000, 5.702370205355745014 ) ) ;
#125811 = ADVANCED_FACE ( 'NONE', ( #18201 ), #71647, .T. ) ;
#125812 = DIRECTION ( 'NONE',  ( 0.000000000000000000, 0.000000000000000000, -1.000000000000000000 ) ) ;
#125813 = CARTESIAN_POINT ( 'NONE',  ( 11.64999999999990798, 12.50000000000000000, 5.867463478539781896 ) ) ;
#125814 = CIRCLE ( 'NONE', #86095, 3.000000000000000000 ) ;
#125815 = AXIS2_PLACEMENT_3D ( 'NONE', #15913, #2892, #122659 ) ;
#125816 = DIRECTION ( 'NONE',  ( -0.000000000000000000, -1.000000000000000000, -0.000000000000000000 ) ) ;
#125817 = ORIENTED_EDGE ( 'NONE', *, *, #124857, .T. ) ;
#125818 = AXIS2_PLACEMENT_3D ( 'NONE', #92560, #2900, #42852 ) ;
#125819 = CONICAL_SURFACE ( 'NONE', #33899, 0.1000000000000002554, 0.003490658503988666988 ) ;
#125820 = CIRCLE ( 'NONE', #61285, 0.06509327318403745899 ) ;
#125821 = EDGE_LOOP ( 'NONE', ( #77116, #26298, #108913, #110127 ) ) ;
#125822 = CARTESIAN_POINT ( 'NONE',  ( -6.050000000000018474, 2.500000000000000000, 2.611473670974873151 ) ) ;
#125823 = EDGE_CURVE ( 'NONE', #54592, #42013, #128089, .T. ) ;
#125824 = CONICAL_SURFACE ( 'NONE', #35960, 0.1000000000000002554, 0.003490658503988666988 ) ;
#125825 = EDGE_CURVE ( 'NONE', #54921, #83172, #105079, .T. ) ;
#125826 = ORIENTED_EDGE ( 'NONE', *, *, #123718, .F. ) ;
#125827 = FACE_OUTER_BOUND ( 'NONE', #119403, .T. ) ;
#125828 = DIRECTION ( 'NONE',  ( 0.000000000000000000, 0.000000000000000000, -1.000000000000000000 ) ) ;
#125829 = ADVANCED_FACE ( 'NONE', ( #68594 ), #63337, .T. ) ;
#125830 = CONICAL_SURFACE ( 'NONE', #113318, 0.09999999999999999167, 0.003490658503988666988 ) ;
#125831 = ORIENTED_EDGE ( 'NONE', *, *, #36327, .F. ) ;
#125832 = CARTESIAN_POINT ( 'NONE',  ( 185.2916666666666572, 4.445597072760120838, -7.699999999999998401 ) ) ;
#125833 = CARTESIAN_POINT ( 'NONE',  ( -2.100000000000034284, 2.500000000000000000, -4.230127018922201998 ) ) ;
#125834 = CARTESIAN_POINT ( 'NONE',  ( -8.750000000000010658, 12.50000000000000000, 2.792790559304612064 ) ) ;
#125835 = ADVANCED_FACE ( 'NONE', ( #28040 ), #58788, .T. ) ;
#125836 = CARTESIAN_POINT ( 'NONE',  ( 1.449999999999951328, 2.500000000000000000, 2.411473670974873862 ) ) ;
#125837 = DIRECTION ( 'NONE',  ( -0.000000000000000000, 1.000000000000000000, -0.000000000000000000 ) ) ;
#125838 = ORIENTED_EDGE ( 'NONE', *, *, #14185, .T. ) ;
#125839 = EDGE_CURVE ( 'NONE', #8618, #119760, #103031, .T. ) ;
#125840 = EDGE_CURVE ( 'NONE', #41779, #104766, #90515, .T. ) ;
#125841 = ADVANCED_FACE ( 'NONE', ( #90820 ), #123958, .T. ) ;
#125842 = DIRECTION ( 'NONE',  ( 0.000000000000000000, 0.000000000000000000, 1.000000000000000000 ) ) ;
#125843 = CARTESIAN_POINT ( 'NONE',  ( 8.149999999999923972, 2.500000000000000000, 2.511473670974873507 ) ) ;
#125844 = ORIENTED_EDGE ( 'NONE', *, *, #109405, .T. ) ;
#125845 = DIRECTION ( 'NONE',  ( 0.000000000000000000, 0.000000000000000000, -1.000000000000000000 ) ) ;
#125846 = PLANE ( 'NONE',  #41361 ) ;
#125847 = EDGE_CURVE ( 'NONE', #67678, #99722, #101292, .T. ) ;
#125848 = DIRECTION ( 'NONE',  ( -4.274815082592931898E-19, -0.9999939076577903929, -0.003490651415223739937 ) ) ;
#125849 = ORIENTED_EDGE ( 'NONE', *, *, #57353, .T. ) ;
#125850 = DIRECTION ( 'NONE',  ( 0.000000000000000000, 1.000000000000000000, -1.224646799147353207E-16 ) ) ;
#125851 = CONICAL_SURFACE ( 'NONE', #69420, 0.1000000000000002554, 0.003490658503988666988 ) ;
#125852 = AXIS2_PLACEMENT_3D ( 'NONE', #113240, #15676, #34053 ) ;
#125853 = ORIENTED_EDGE ( 'NONE', *, *, #95058, .F. ) ;
#125854 = CARTESIAN_POINT ( 'NONE',  ( 10.39999999999991331, 2.500000000000000000, -0.1000000000000023925 ) ) ;
#125855 = DIRECTION ( 'NONE',  ( 0.000000000000000000, 0.000000000000000000, -1.000000000000000000 ) ) ;
#125856 = DIRECTION ( 'NONE',  ( -0.000000000000000000, 1.000000000000000000, -0.000000000000000000 ) ) ;
#125857 = ORIENTED_EDGE ( 'NONE', *, *, #72240, .T. ) ;
#125858 = CARTESIAN_POINT ( 'NONE',  ( 7.899999999999924860, 12.50000000000000000, -4.395220292106239768 ) ) ;
#125859 = AXIS2_PLACEMENT_3D ( 'NONE', #126964, #127606, #76574 ) ;
#125860 = VECTOR ( 'NONE', #79901, 1000.000000000000000 ) ;
#125861 = DIRECTION ( 'NONE',  ( 0.000000000000000000, -0.9999939076577903929, 0.003490651415223739937 ) ) ;
#125862 = ORIENTED_EDGE ( 'NONE', *, *, #74665, .F. ) ;
#125863 = CIRCLE ( 'NONE', #15031, 0.06509327318403745899 ) ;
#125864 = VERTEX_POINT ( 'NONE', #111753 ) ;
#125865 = CONICAL_SURFACE ( 'NONE', #4664, 0.1000000000000002554, 0.003490658503988666988 ) ;
#125866 = DIRECTION ( 'NONE',  ( -0.000000000000000000, -1.000000000000000000, -0.000000000000000000 ) ) ;
#125867 = VERTEX_POINT ( 'NONE', #112403 ) ;
#125868 = FACE_OUTER_BOUND ( 'NONE', #94970, .T. ) ;
#125869 = DIRECTION ( 'NONE',  ( 0.000000000000000000, 0.000000000000000000, 1.000000000000000000 ) ) ;
#125870 = ORIENTED_EDGE ( 'NONE', *, *, #18016, .T. ) ;
#125871 = DIRECTION ( 'NONE',  ( 0.000000000000000000, 0.000000000000000000, 1.000000000000000000 ) ) ;
#125872 = LINE ( 'NONE', #106876, #2484 ) ;
#125873 = ORIENTED_EDGE ( 'NONE', *, *, #16265, .F. ) ;
#125874 = CARTESIAN_POINT ( 'NONE',  ( -9.800000000000004263, 2.500000000000000000, -0.3464101615137783474 ) ) ;
#125875 = DIRECTION ( 'NONE',  ( -0.000000000000000000, 1.000000000000000000, -0.000000000000000000 ) ) ;
#125876 = EDGE_CURVE ( 'NONE', #111738, #6241, #121815, .T. ) ;
#125877 = CARTESIAN_POINT ( 'NONE',  ( 17.27572160909437926, -2.230096426605189031, -5.047229640871994327 ) ) ;
#125878 = CARTESIAN_POINT ( 'NONE',  ( 0.3999999999999563904, 2.500000000000000000, 5.122947341949749323 ) ) ;
#125879 = DIRECTION ( 'NONE',  ( -0.000000000000000000, 1.000000000000000000, -0.000000000000000000 ) ) ;
#125880 = DIRECTION ( 'NONE',  ( 0.000000000000000000, 0.000000000000000000, 1.000000000000000000 ) ) ;
#125881 = AXIS2_PLACEMENT_3D ( 'NONE', #86055, #116814, #75594 ) ;
#125882 = ORIENTED_EDGE ( 'NONE', *, *, #116805, .F. ) ;
#125883 = ORIENTED_EDGE ( 'NONE', *, *, #39698, .F. ) ;
#125884 = ORIENTED_EDGE ( 'NONE', *, *, #37823, .T. ) ;
#125885 = ORIENTED_EDGE ( 'NONE', *, *, #97843, .F. ) ;
#125886 = CARTESIAN_POINT ( 'NONE',  ( 5.599999999999931255, 12.50000000000000000, 4.741630453620009789 ) ) ;
#125887 = LINE ( 'NONE', #68262, #115978 ) ;
#125888 = CARTESIAN_POINT ( 'NONE',  ( -2.700000000000031264, 2.500000000000000000, 4.676537180435972552 ) ) ;
#125889 = ORIENTED_EDGE ( 'NONE', *, *, #33380, .F. ) ;
#125890 = EDGE_CURVE ( 'NONE', #5720, #25038, #65375, .T. ) ;
#125891 = FACE_BOUND ( 'NONE', #92602, .T. ) ;
#125892 = CIRCLE ( 'NONE', #100852, 0.1000000000000000472 ) ;
#125893 = DIRECTION ( 'NONE',  ( -0.000000000000000000, -1.000000000000000000, -0.000000000000000000 ) ) ;
#125894 = CARTESIAN_POINT ( 'NONE',  ( 2.899999999999945732, 2.500000000000000000, 0.09999999999999761857 ) ) ;
#125895 = CONICAL_SURFACE ( 'NONE', #123841, 0.09999999999999999167, 0.003490658503988666988 ) ;
#125897 = DIRECTION ( 'NONE',  ( 0.000000000000000000, 0.000000000000000000, 1.000000000000000000 ) ) ;
#125896 = AXIS2_PLACEMENT_3D ( 'NONE', #93729, #43996, #32253 ) ;
#125898 = VECTOR ( 'NONE', #129249, 1000.000000000000000 ) ;
#125899 = PLANE ( 'NONE',  #107702 ) ;
#125900 = FACE_OUTER_BOUND ( 'NONE', #100481, .T. ) ;
#125901 = PLANE ( 'NONE',  #110278 ) ;
#125902 = DIRECTION ( 'NONE',  ( 0.000000000000000000, 0.000000000000000000, -1.000000000000000000 ) ) ;
#125903 = DIRECTION ( 'NONE',  ( 0.000000000000000000, 0.000000000000000000, 1.000000000000000000 ) ) ;
#125904 = DIRECTION ( 'NONE',  ( 0.000000000000000000, 0.000000000000000000, 1.000000000000000000 ) ) ;
#125905 = VECTOR ( 'NONE', #70969, 1000.000000000000000 ) ;
#125906 = DIRECTION ( 'NONE',  ( 0.000000000000000000, 0.000000000000000000, 1.000000000000000000 ) ) ;
#125907 = AXIS2_PLACEMENT_3D ( 'NONE', #13828, #114611, #112695 ) ;
#125908 = VERTEX_POINT ( 'NONE', #89531 ) ;
#125909 = ORIENTED_EDGE ( 'NONE', *, *, #90362, .T. ) ;
#125910 = ORIENTED_EDGE ( 'NONE', *, *, #115309, .T. ) ;
#125912 = EDGE_LOOP ( 'NONE', ( #17369, #80688, #107749, #67847 ) ) ;
#125911 = AXIS2_PLACEMENT_3D ( 'NONE', #56868, #77178, #26150 ) ;
#125913 = VECTOR ( 'NONE', #91669, 1000.000000000000000 ) ;
#125914 = CARTESIAN_POINT ( 'NONE',  ( 3.349999999999942801, 2.500000000000000000, 2.757883832488649656 ) ) ;
#125915 = ORIENTED_EDGE ( 'NONE', *, *, #88253, .F. ) ;
#125916 = CARTESIAN_POINT ( 'NONE',  ( -10.65000000000000213, 2.500000000000000000, 6.941600689897073018 ) ) ;
#125917 = EDGE_LOOP ( 'NONE', ( #95221, #48429, #25991, #5119 ) ) ;
#125918 = ORIENTED_EDGE ( 'NONE', *, *, #115920, .T. ) ;
#125919 = FACE_OUTER_BOUND ( 'NONE', #4174, .T. ) ;
#125920 = EDGE_CURVE ( 'NONE', #52063, #108189, #101936, .T. ) ;
#125921 = CIRCLE ( 'NONE', #67410, 0.06509327318403745899 ) ;
#125922 = CARTESIAN_POINT ( 'NONE',  ( 2.049999999999950084, 2.500000000000000000, -6.595190528383302109 ) ) ;
#125923 = DIRECTION ( 'NONE',  ( 0.000000000000000000, 0.000000000000000000, 1.000000000000000000 ) ) ;
#125924 = CARTESIAN_POINT ( 'NONE',  ( -1.700000000000034817, 2.500000000000000000, -4.230127018922201998 ) ) ;
#125925 = CARTESIAN_POINT ( 'NONE',  ( -7.900000000000014566, 12.50000000000000000, -3.637306695894650055 ) ) ;
#125926 = ORIENTED_EDGE ( 'NONE', *, *, #98371, .T. ) ;
#125927 = EDGE_CURVE ( 'NONE', #114454, #67065, #113498, .T. ) ;
#125928 = VERTEX_POINT ( 'NONE', #62664 ) ;
#125929 = VERTEX_POINT ( 'NONE', #41102 ) ;
#125930 = EDGE_LOOP ( 'NONE', ( #66184, #56915, #92486, #108526 ) ) ;
#125931 = ADVANCED_FACE ( 'NONE', ( #22102 ), #31273, .T. ) ;
#125933 = EDGE_CURVE ( 'NONE', #23542, #122530, #109298, .T. ) ;
#125932 = LINE ( 'NONE', #95208, #25331 ) ;
#125935 = ORIENTED_EDGE ( 'NONE', *, *, #123008, .F. ) ;
#125934 = EDGE_CURVE ( 'NONE', #87918, #104138, #61370, .T. ) ;
#125936 = EDGE_CURVE ( 'NONE', #117538, #80227, #126012, .T. ) ;
#125938 = EDGE_LOOP ( 'NONE', ( #58581, #80940, #108242, #119575 ) ) ;
#125937 = ADVANCED_FACE ( 'NONE', ( #80372 ), #102562, .T. ) ;
#125939 = FACE_OUTER_BOUND ( 'NONE', #81084, .T. ) ;
#125940 = LINE ( 'NONE', #95857, #49681 ) ;
#125941 = CARTESIAN_POINT ( 'NONE',  ( -5.400000000000020783, 2.500000000000000000, 5.122947341949749323 ) ) ;
#125942 = DIRECTION ( 'NONE',  ( 0.000000000000000000, 0.000000000000000000, 1.000000000000000000 ) ) ;
#125943 = CONICAL_SURFACE ( 'NONE', #84177, 0.09999999999999999167, 0.003490658503988666988 ) ;
#125944 = VECTOR ( 'NONE', #110978, 1000.000000000000000 ) ;
#125945 = DIRECTION ( 'NONE',  ( -0.000000000000000000, 1.000000000000000000, -0.000000000000000000 ) ) ;
#125946 = DIRECTION ( 'NONE',  ( 0.000000000000000000, 1.000000000000000000, 0.000000000000000000 ) ) ;
#125947 = EDGE_CURVE ( 'NONE', #84422, #100878, #13135, .T. ) ;
#125948 = ORIENTED_EDGE ( 'NONE', *, *, #61964, .F. ) ;
#125949 = CARTESIAN_POINT ( 'NONE',  ( 12.69999999999989981, 12.50000000000000000, -0.3464101615137783474 ) ) ;
#125950 = EDGE_CURVE ( 'NONE', #122396, #108909, #57061, .T. ) ;
#125952 = EDGE_CURVE ( 'NONE', #107019, #20664, #46606, .T. ) ;
#125951 = VECTOR ( 'NONE', #28094, 1000.000000000000000 ) ;
#125954 = EDGE_LOOP ( 'NONE', ( #87099, #21691 ) ) ;
#125953 = AXIS2_PLACEMENT_3D ( 'NONE', #33291, #52916, #73197 ) ;
#125955 = CARTESIAN_POINT ( 'NONE',  ( 186.1666666666666856, -6.668395609140176816, -3.850000000000003642 ) ) ;
#125956 = ORIENTED_EDGE ( 'NONE', *, *, #8577, .F. ) ;
#125957 = CARTESIAN_POINT ( 'NONE',  ( 0.4499999999999552136, 2.500000000000000000, 6.495190528383297135 ) ) ;
#125958 = CARTESIAN_POINT ( 'NONE',  ( -0.6500000000000398792, 2.500000000000000000, -2.511473670974877948 ) ) ;
#125959 = CIRCLE ( 'NONE', #23564, 0.1000000000000002554 ) ;
#125960 = VERTEX_POINT ( 'NONE', #39810 ) ;
#125961 = AXIS2_PLACEMENT_3D ( 'NONE', #84409, #64763, #26781 ) ;
#125962 = DIRECTION ( 'NONE',  ( 0.000000000000000000, 0.000000000000000000, -1.000000000000000000 ) ) ;
#125963 = CARTESIAN_POINT ( 'NONE',  ( -1.650000000000034772, 12.50000000000000000, 6.495190528383297135 ) ) ;
#125964 = ORIENTED_EDGE ( 'NONE', *, *, #96390, .T. ) ;
#125965 = AXIS2_PLACEMENT_3D ( 'NONE', #8287, #128079, #17454 ) ;
#125966 = CARTESIAN_POINT ( 'NONE',  ( 9.599999999999914380, 2.500000000000000000, 3.737306695894644371 ) ) ;
#125967 = VERTEX_POINT ( 'NONE', #119623 ) ;
#125968 = ORIENTED_EDGE ( 'NONE', *, *, #1285, .F. ) ;
#125969 = LINE ( 'NONE', #116150, #60388 ) ;
#125970 = DIRECTION ( 'NONE',  ( 0.000000000000000000, 0.000000000000000000, 1.000000000000000000 ) ) ;
#125971 = CARTESIAN_POINT ( 'NONE',  ( 186.3385416670080872, 6.551208109652274736, 3.782341765625001351 ) ) ;
#125972 = CARTESIAN_POINT ( 'NONE',  ( -1.450000000000035039, 2.500000000000000000, -2.611473670974877592 ) ) ;
#125973 = AXIS2_PLACEMENT_3D ( 'NONE', #18636, #95912, #58584 ) ;
#125974 = CARTESIAN_POINT ( 'NONE',  ( -8.950000000000004619, 12.50000000000000000, 6.148780366869520897 ) ) ;
#125975 = DIRECTION ( 'NONE',  ( 0.000000000000000000, -0.9999939076577903929, 0.003490651415223739937 ) ) ;
#125976 = AXIS2_PLACEMENT_3D ( 'NONE', #15884, #105567, #116665 ) ;
#125977 = EDGE_LOOP ( 'NONE', ( #105072, #32689, #64989, #110388 ) ) ;
#125978 = AXIS2_PLACEMENT_3D ( 'NONE', #106404, #86101, #36399 ) ;
#125979 = DIRECTION ( 'NONE',  ( 0.000000000000000000, -0.9999939076577903929, 0.003490651415223739937 ) ) ;
#125980 = VECTOR ( 'NONE', #62957, 1000.000000000000000 ) ;
#125981 = ORIENTED_EDGE ( 'NONE', *, *, #95572, .F. ) ;
#125982 = DIRECTION ( 'NONE',  ( -0.000000000000000000, -1.000000000000000000, -0.000000000000000000 ) ) ;
#125983 = DIRECTION ( 'NONE',  ( -4.274815082592931898E-19, -0.9999939076577903929, -0.003490651415223739937 ) ) ;
#125984 = ADVANCED_FACE ( 'NONE', ( #2415 ), #4726, .T. ) ;
#125985 = CARTESIAN_POINT ( 'NONE',  ( -10.20000000000000639, 12.50000000000000000, -4.048810130592459089 ) ) ;
#125986 = AXIS2_PLACEMENT_3D ( 'NONE', #53844, #114682, #74134 ) ;
#125987 = ORIENTED_EDGE ( 'NONE', *, *, #98979, .T. ) ;
#125988 = ADVANCED_FACE ( 'NONE', ( #44953 ), #38004, .T. ) ;
#125989 = CONICAL_SURFACE ( 'NONE', #34075, 0.1000000000000000472, 0.003490658503988666988 ) ;
#125990 = VECTOR ( 'NONE', #45364, 1000.000000000000000 ) ;
#125991 = EDGE_CURVE ( 'NONE', #121009, #112979, #23349, .T. ) ;
#125992 = DIRECTION ( 'NONE',  ( 0.000000000000000000, 0.000000000000000000, 1.000000000000000000 ) ) ;
#125993 = LINE ( 'NONE', #106366, #78903 ) ;
#125994 = AXIS2_PLACEMENT_3D ( 'NONE', #78561, #109283, #39298 ) ;
#125995 = VERTEX_POINT ( 'NONE', #73118 ) ;
#125996 = EDGE_CURVE ( 'NONE', #17997, #35493, #15468, .T. ) ;
#125998 = AXIS2_PLACEMENT_3D ( 'NONE', #47831, #38664, #87724 ) ;
#125997 = CARTESIAN_POINT ( 'NONE',  ( 1.649999999999949729, 2.500000000000000000, 7.088010851410848190 ) ) ;
#125999 = VERTEX_POINT ( 'NONE', #95334 ) ;
#126000 = CIRCLE ( 'NONE', #23611, 0.06509327318403745899 ) ;
#126002 = VERTEX_POINT ( 'NONE', #43678 ) ;
#126001 = CIRCLE ( 'NONE', #69580, 0.06509327318403745899 ) ;
#126003 = AXIS2_PLACEMENT_3D ( 'NONE', #9864, #17730, #49804 ) ;
#126004 = CARTESIAN_POINT ( 'NONE',  ( 7.499999999999923617, 2.500000000000000000, 0.6928203230275494784 ) ) ;
#126006 = VERTEX_POINT ( 'NONE', #52827 ) ;
#126005 = AXIS2_PLACEMENT_3D ( 'NONE', #86113, #16083, #95318 ) ;
#126007 = CARTESIAN_POINT ( 'NONE',  ( 3.949999999999938005, 12.50000000000000000, 6.841600689897072485 ) ) ;
#126008 = FACE_OUTER_BOUND ( 'NONE', #4319, .T. ) ;
#126009 = DIRECTION ( 'NONE',  ( -0.000000000000000000, 1.000000000000000000, -0.000000000000000000 ) ) ;
#126010 = ORIENTED_EDGE ( 'NONE', *, *, #79968, .T. ) ;
#126011 = FACE_BOUND ( 'NONE', #103782, .T. ) ;
#126012 = CIRCLE ( 'NONE', #107239, 0.06509327318403745899 ) ;
#126014 = ORIENTED_EDGE ( 'NONE', *, *, #63347, .T. ) ;
#126013 = DIRECTION ( 'NONE',  ( -4.274815082592931898E-19, -0.9999939076577903929, -0.003490651415223739937 ) ) ;
#126015 = DIRECTION ( 'NONE',  ( 0.000000000000000000, 0.000000000000000000, 1.000000000000000000 ) ) ;
#126016 = CARTESIAN_POINT ( 'NONE',  ( -11.64999999999999680, 12.50000000000000000, -6.430097255199260786 ) ) ;
#126017 = EDGE_CURVE ( 'NONE', #108104, #29267, #54745, .T. ) ;
#126018 = EDGE_LOOP ( 'NONE', ( #19237, #80734, #76240, #6582 ) ) ;
#126019 = ORIENTED_EDGE ( 'NONE', *, *, #123684, .F. ) ;
#126020 = ORIENTED_EDGE ( 'NONE', *, *, #82783, .F. ) ;
#126021 = DIRECTION ( 'NONE',  ( -0.000000000000000000, 1.000000000000000000, -0.000000000000000000 ) ) ;
#126022 = CARTESIAN_POINT ( 'NONE',  ( 5.599999999999934808, 12.50000000000000000, -4.676537180435978769 ) ) ;
#126023 = FACE_OUTER_BOUND ( 'NONE', #56650, .T. ) ;
#126024 = AXIS2_PLACEMENT_3D ( 'NONE', #104098, #54348, #56906 ) ;
#126025 = FACE_BOUND ( 'NONE', #42430, .T. ) ;
#126026 = VERTEX_POINT ( 'NONE', #114954 ) ;
#126027 = CARTESIAN_POINT ( 'NONE',  ( 186.8593750003414016, 0.000000000000000000, 7.564683531250000925 ) ) ;
#126028 = FACE_OUTER_BOUND ( 'NONE', #18276, .T. ) ;
#126029 = FACE_OUTER_BOUND ( 'NONE', #23088, .T. ) ;
#126031 = FACE_OUTER_BOUND ( 'NONE', #53859, .T. ) ;
#126030 = CIRCLE ( 'NONE', #109615, 0.06509327318403745899 ) ;
#126032 = ADVANCED_FACE ( 'NONE', ( #82945 ), #124797, .T. ) ;
#126033 = CONICAL_SURFACE ( 'NONE', #23640, 0.1000000000000000056, 0.003490658503988666988 ) ;
#126034 = AXIS2_PLACEMENT_3D ( 'NONE', #88914, #108549, #128864 ) ;
#126036 = AXIS2_PLACEMENT_3D ( 'NONE', #126633, #23922, #4246 ) ;
#126035 = FACE_OUTER_BOUND ( 'NONE', #840, .T. ) ;
#126037 = DIRECTION ( 'NONE',  ( 0.000000000000000000, 0.000000000000000000, -1.000000000000000000 ) ) ;
#126038 = DIRECTION ( 'NONE',  ( 0.000000000000000000, 0.000000000000000000, -1.000000000000000000 ) ) ;
#126039 = DIRECTION ( 'NONE',  ( 0.000000000000000000, 0.000000000000000000, 1.000000000000000000 ) ) ;
#126040 = AXIS2_PLACEMENT_3D ( 'NONE', #70150, #78025, #19079 ) ;
#126042 = DIRECTION ( 'NONE',  ( 0.000000000000000000, 0.000000000000000000, -1.000000000000000000 ) ) ;
#126041 = AXIS2_PLACEMENT_3D ( 'NONE', #80936, #92679, #12804 ) ;
#126043 = ORIENTED_EDGE ( 'NONE', *, *, #120029, .F. ) ;
#126044 = VERTEX_POINT ( 'NONE', #115597 ) ;
#126045 = EDGE_LOOP ( 'NONE', ( #76832, #6858 ) ) ;
#126046 = ORIENTED_EDGE ( 'NONE', *, *, #55309, .F. ) ;
#126048 = ORIENTED_EDGE ( 'NONE', *, *, #122741, .F. ) ;
#126047 = AXIS2_PLACEMENT_3D ( 'NONE', #33851, #112428, #12269 ) ;
#126049 = DIRECTION ( 'NONE',  ( -0.000000000000000000, 1.000000000000000000, 1.846105847067148022E-16 ) ) ;
#126050 = AXIS2_PLACEMENT_3D ( 'NONE', #29778, #80169, #59261 ) ;
#126051 = DIRECTION ( 'NONE',  ( 0.000000000000000000, -0.000000000000000000, 1.000000000000000000 ) ) ;
#126052 = VERTEX_POINT ( 'NONE', #85510 ) ;
#126053 = EDGE_CURVE ( 'NONE', #11304, #54885, #3723, .T. ) ;
#126054 = FACE_BOUND ( 'NONE', #32220, .T. ) ;
#126055 = AXIS2_PLACEMENT_3D ( 'NONE', #19749, #91053, #9274 ) ;
#126056 = CARTESIAN_POINT ( 'NONE',  ( -3.550000000000031797, 2.500000000000000000, -6.248780366869526759 ) ) ;
#126057 = DIRECTION ( 'NONE',  ( -4.274815082592931898E-19, -0.9999939076577903929, -0.003490651415223739937 ) ) ;
#126058 = FACE_OUTER_BOUND ( 'NONE', #33494, .T. ) ;
#126059 = ADVANCED_FACE ( 'NONE', ( #124143 ), #21280, .T. ) ;
#126060 = DIRECTION ( 'NONE',  ( 0.000000000000000000, 1.000000000000000000, 0.000000000000000000 ) ) ;
#126061 = DIRECTION ( 'NONE',  ( 1.000000000000000000, 0.000000000000000000, 0.000000000000000000 ) ) ;
#126062 = ORIENTED_EDGE ( 'NONE', *, *, #5363, .T. ) ;
#126063 = CARTESIAN_POINT ( 'NONE',  ( -11.69999999999999574, 2.500000000000000000, 4.230127018922196669 ) ) ;
#126064 = AXIS2_PLACEMENT_3D ( 'NONE', #53278, #93834, #63734 ) ;
#126065 = ORIENTED_EDGE ( 'NONE', *, *, #66461, .F. ) ;
#126066 = ORIENTED_EDGE ( 'NONE', *, *, #128975, .F. ) ;
#126067 = VERTEX_POINT ( 'NONE', #125436 ) ;
#126068 = DIRECTION ( 'NONE',  ( -0.000000000000000000, 1.000000000000000000, -0.000000000000000000 ) ) ;
#126069 = CARTESIAN_POINT ( 'NONE',  ( 5.849999999999933031, 2.500000000000000000, -1.472243186433550122 ) ) ;
#126070 = DIRECTION ( 'NONE',  ( 0.000000000000000000, 0.000000000000000000, -1.000000000000000000 ) ) ;
#126071 = ORIENTED_EDGE ( 'NONE', *, *, #106607, .T. ) ;
#126072 = CARTESIAN_POINT ( 'NONE',  ( 16.31259999906430025, 2.500000000000969891, -6.357732693023527837 ) ) ;
#126073 = AXIS2_PLACEMENT_3D ( 'NONE', #45055, #73851, #84956 ) ;
#126074 = AXIS2_PLACEMENT_3D ( 'NONE', #30454, #60560, #50712 ) ;
#126076 = DIRECTION ( 'NONE',  ( 0.000000000000000000, 1.000000000000000000, 0.000000000000000000 ) ) ;
#126075 = AXIS2_PLACEMENT_3D ( 'NONE', #19665, #68105, #20310 ) ;
#126077 = ADVANCED_FACE ( 'NONE', ( #5644 ), #104500, .T. ) ;
#126078 = DIRECTION ( 'NONE',  ( 0.000000000000000000, 0.000000000000000000, -1.000000000000000000 ) ) ;
#126079 = CARTESIAN_POINT ( 'NONE',  ( 186.6510416670080303, 4.367472073101518859, -7.564683531249999149 ) ) ;
#126080 = CARTESIAN_POINT ( 'NONE',  ( -2.900000000000029665, 2.500000000000000000, 4.330127018922196314 ) ) ;
#126081 = DIRECTION ( 'NONE',  ( 0.000000000000000000, 0.000000000000000000, -1.000000000000000000 ) ) ;
#126082 = CIRCLE ( 'NONE', #69656, 0.06509327318403745899 ) ;
#126083 = ORIENTED_EDGE ( 'NONE', *, *, #44553, .F. ) ;
#126084 = DIRECTION ( 'NONE',  ( -0.000000000000000000, 1.000000000000000000, -0.000000000000000000 ) ) ;
#126085 = AXIS2_PLACEMENT_3D ( 'NONE', #124845, #95382, #85557 ) ;
#126087 = EDGE_CURVE ( 'NONE', #100531, #15792, #81906, .T. ) ;
#126086 = AXIS2_PLACEMENT_3D ( 'NONE', #15478, #32091, #111924 ) ;
#126088 = EDGE_LOOP ( 'NONE', ( #84123, #86742, #53911, #23662 ) ) ;
#126089 = AXIS2_PLACEMENT_3D ( 'NONE', #82228, #22677, #10874 ) ;
#126090 = ORIENTED_EDGE ( 'NONE', *, *, #111742, .T. ) ;
#126091 = CARTESIAN_POINT ( 'NONE',  ( -4.400000000000028777, 2.500000000000000000, -3.883716857408426648 ) ) ;
#126092 = ADVANCED_FACE ( 'NONE', ( #93402 ), #2487, .T. ) ;
#126093 = DIRECTION ( 'NONE',  ( 0.000000000000000000, 0.000000000000000000, 1.000000000000000000 ) ) ;
#126095 = EDGE_CURVE ( 'NONE', #91667, #52767, #102830, .T. ) ;
#126094 = DIRECTION ( 'NONE',  ( 0.000000000000000000, 1.000000000000000000, 0.000000000000000000 ) ) ;
#126096 = EDGE_CURVE ( 'NONE', #57274, #121670, #94721, .T. ) ;
#126097 = EDGE_CURVE ( 'NONE', #98528, #49455, #31762, .T. ) ;
#126098 = VERTEX_POINT ( 'NONE', #94043 ) ;
#126099 = ORIENTED_EDGE ( 'NONE', *, *, #103635, .F. ) ;
#126100 = DIRECTION ( 'NONE',  ( 1.000000000000000000, 0.000000000000000000, 0.000000000000000000 ) ) ;
#126102 = AXIS2_PLACEMENT_3D ( 'NONE', #10124, #99155, #58588 ) ;
#126101 = CARTESIAN_POINT ( 'NONE',  ( 87.50000000000001421, 3.975344334345554120, -6.360552532166837914 ) ) ;
#126103 = CIRCLE ( 'NONE', #117767, 0.09999999999999982514 ) ;
#126104 = AXIS2_PLACEMENT_3D ( 'NONE', #118362, #68615, #108550 ) ;
#126105 = EDGE_CURVE ( 'NONE', #121644, #57128, #125820, .T. ) ;
#126106 = LINE ( 'NONE', #113721, #75315 ) ;
#126107 = EDGE_LOOP ( 'NONE', ( #113748, #120894 ) ) ;
#126108 = VERTEX_POINT ( 'NONE', #84862 ) ;
#126109 = EDGE_CURVE ( 'NONE', #119087, #127598, #4819, .T. ) ;
#126110 = CARTESIAN_POINT ( 'NONE',  ( -10.84999999999999964, 2.500000000000000000, 1.372243186433545370 ) ) ;
#126111 = CIRCLE ( 'NONE', #11180, 0.09999999999999982514 ) ;
#126112 = EDGE_CURVE ( 'NONE', #88786, #71397, #54713, .T. ) ;
#126113 = VERTEX_POINT ( 'NONE', #6280 ) ;
#126114 = DIRECTION ( 'NONE',  ( 0.000000000000000000, 1.000000000000000000, 0.000000000000000000 ) ) ;
#126115 = ADVANCED_FACE ( 'NONE', ( #126731 ), #97900, .T. ) ;
#126116 = EDGE_CURVE ( 'NONE', #99549, #21005, #25764, .T. ) ;
#126117 = DIRECTION ( 'NONE',  ( 0.000000000000000000, 0.000000000000000000, 1.000000000000000000 ) ) ;
#126118 = ORIENTED_EDGE ( 'NONE', *, *, #83451, .F. ) ;
#126119 = DIRECTION ( 'NONE',  ( -0.000000000000000000, -1.000000000000000000, -0.000000000000000000 ) ) ;
#126120 = DIRECTION ( 'NONE',  ( 0.000000000000000000, -0.000000000000000000, 1.000000000000000000 ) ) ;
#126121 = CARTESIAN_POINT ( 'NONE',  ( -1.250000000000037526, 2.500000000000000000, -1.372243186433550033 ) ) ;
#126123 = EDGE_CURVE ( 'NONE', #57756, #72103, #14990, .T. ) ;
#126122 = DIRECTION ( 'NONE',  ( 0.000000000000000000, 0.000000000000000000, 1.000000000000000000 ) ) ;
#126124 = ORIENTED_EDGE ( 'NONE', *, *, #2682, .T. ) ;
#126125 = LINE ( 'NONE', #64627, #50885 ) ;
#126126 = CARTESIAN_POINT ( 'NONE',  ( -3.550000000000028244, 2.500000000000000000, -1.818653347947326138 ) ) ;
#126127 = VERTEX_POINT ( 'NONE', #67800 ) ;
#126128 = ORIENTED_EDGE ( 'NONE', *, *, #38452, .F. ) ;
#126129 = AXIS2_PLACEMENT_3D ( 'NONE', #115136, #16301, #15658 ) ;
#126130 = CIRCLE ( 'NONE', #69695, 0.1000000000000002554 ) ;
#126131 = CARTESIAN_POINT ( 'NONE',  ( -11.64999999999999858, 2.500000000000000000, -5.702370205355745902 ) ) ;
#126132 = DIRECTION ( 'NONE',  ( 0.000000000000000000, 0.000000000000000000, -1.000000000000000000 ) ) ;
#126133 = CARTESIAN_POINT ( 'NONE',  ( 6.449999999999930012, 2.500000000000000000, 1.818653347947321475 ) ) ;
#126134 = CARTESIAN_POINT ( 'NONE',  ( 11.89999999999990798, 2.500000000000000000, -4.576537180435977348 ) ) ;
#126135 = DIRECTION ( 'NONE',  ( 0.000000000000000000, 1.000000000000000000, 0.000000000000000000 ) ) ;
#126136 = DIRECTION ( 'NONE',  ( 0.000000000000000000, 0.000000000000000000, 1.000000000000000000 ) ) ;
#126137 = AXIS2_PLACEMENT_3D ( 'NONE', #13471, #92693, #3030 ) ;
#126138 = VECTOR ( 'NONE', #45016, 1000.000000000000000 ) ;
#126139 = DIRECTION ( 'NONE',  ( 0.000000000000000000, 0.000000000000000000, -1.000000000000000000 ) ) ;
#126140 = AXIS2_PLACEMENT_3D ( 'NONE', #53621, #66012, #13679 ) ;
#126141 = PLANE ( 'NONE',  #57389 ) ;
#126143 = CIRCLE ( 'NONE', #128305, 0.1000000000000002554 ) ;
#126142 = DIRECTION ( 'NONE',  ( 0.000000000000000000, 1.000000000000000000, 0.000000000000000000 ) ) ;
#126144 = AXIS2_PLACEMENT_3D ( 'NONE', #115332, #125186, #6035 ) ;
#126145 = DIRECTION ( 'NONE',  ( 0.000000000000000000, 0.000000000000000000, 1.000000000000000000 ) ) ;
#126146 = EDGE_LOOP ( 'NONE', ( #116402, #42221, #64048, #92173 ) ) ;
#126147 = AXIS2_PLACEMENT_3D ( 'NONE', #115857, #119090, #37319 ) ;
#126148 = AXIS2_PLACEMENT_3D ( 'NONE', #59144, #99064, #49337 ) ;
#126149 = AXIS2_PLACEMENT_3D ( 'NONE', #115392, #16558, #96411 ) ;
#126150 = EDGE_LOOP ( 'NONE', ( #117837, #72696 ) ) ;
#126151 = AXIS2_PLACEMENT_3D ( 'NONE', #50140, #58020, #89404 ) ;
#126152 = FACE_OUTER_BOUND ( 'NONE', #123871, .T. ) ;
#126153 = VECTOR ( 'NONE', #27585, 1000.000000000000000 ) ;
#126154 = ORIENTED_EDGE ( 'NONE', *, *, #78886, .F. ) ;
#126155 = CARTESIAN_POINT ( 'NONE',  ( -4.800000000000022915, 2.500000000000000000, 3.983716857408420076 ) ) ;
#126156 = CARTESIAN_POINT ( 'NONE',  ( -3.750000000000027978, 12.50000000000000000, 7.122917578226811486 ) ) ;
#126157 = DIRECTION ( 'NONE',  ( 0.000000000000000000, 0.000000000000000000, 1.000000000000000000 ) ) ;
#126158 = ORIENTED_EDGE ( 'NONE', *, *, #103062, .T. ) ;
#126159 = CARTESIAN_POINT ( 'NONE',  ( 17.50000000000000000, -2.500000000000000000, -2.922290670087884124 ) ) ;
#126160 = EDGE_CURVE ( 'NONE', #65136, #9133, #107731, .T. ) ;
#126161 = EDGE_CURVE ( 'NONE', #73855, #89818, #19209, .T. ) ;
#126162 = DIRECTION ( 'NONE',  ( 0.000000000000000000, -0.9999939076577903929, 0.003490651415223739937 ) ) ;
#126164 = VERTEX_POINT ( 'NONE', #116884 ) ;
#126163 = CARTESIAN_POINT ( 'NONE',  ( -4.350000000000023626, 2.500000000000000000, 2.511473670974873507 ) ) ;
#126166 = DIRECTION ( 'NONE',  ( 0.000000000000000000, 0.000000000000000000, 1.000000000000000000 ) ) ;
#126165 = AXIS2_PLACEMENT_3D ( 'NONE', #4618, #121837, #82582 ) ;
#126167 = EDGE_LOOP ( 'NONE', ( #24309, #100701 ) ) ;
#126168 = ADVANCED_FACE ( 'NONE', ( #7582 ), #121921, .T. ) ;
#126169 = EDGE_LOOP ( 'NONE', ( #34763, #57193 ) ) ;
#126170 = ORIENTED_EDGE ( 'NONE', *, *, #43107, .F. ) ;
#126171 = ORIENTED_EDGE ( 'NONE', *, *, #53836, .F. ) ;
#126172 = FACE_OUTER_BOUND ( 'NONE', #14946, .T. ) ;
#126174 = CIRCLE ( 'NONE', #688, 0.09999999999999999167 ) ;
#126173 = CARTESIAN_POINT ( 'NONE',  ( -7.499999999999980460, 12.50000000000000000, -2.276824562219559311E-15 ) ) ;
#126175 = FACE_OUTER_BOUND ( 'NONE', #115372, .T. ) ;
#126176 = AXIS2_PLACEMENT_3D ( 'NONE', #100310, #100931, #2732 ) ;
#126177 = DIRECTION ( 'NONE',  ( 0.000000000000000000, 0.000000000000000000, 1.000000000000000000 ) ) ;
#126178 = VECTOR ( 'NONE', #6868, 1000.000000000000114 ) ;
#126179 = EDGE_LOOP ( 'NONE', ( #77874, #120148 ) ) ;
#126180 = CARTESIAN_POINT ( 'NONE',  ( 8.749999999999921840, 2.500000000000000000, -5.902370205355750521 ) ) ;
#126181 = ORIENTED_EDGE ( 'NONE', *, *, #122381, .T. ) ;
#126182 = LINE ( 'NONE', #75154, #124915 ) ;
#126183 = CARTESIAN_POINT ( 'NONE',  ( -5.400000000000019895, 2.500000000000000000, 3.637306695894644726 ) ) ;
#126184 = DIRECTION ( 'NONE',  ( 0.000000000000000000, 0.000000000000000000, 1.000000000000000000 ) ) ;
#126185 = CARTESIAN_POINT ( 'NONE',  ( 20.06694580393955007, -2.635910463901628642, 2.269534205242087044 ) ) ;
#126186 = VECTOR ( 'NONE', #3064, 1000.000000000000000 ) ;
#126187 = AXIS2_PLACEMENT_3D ( 'NONE', #20693, #42271, #91355 ) ;
#126188 = CIRCLE ( 'NONE', #128360, 0.06509327318403745899 ) ;
#126189 = EDGE_LOOP ( 'NONE', ( #13894, #124060, #87254, #73092 ) ) ;
#126190 = VECTOR ( 'NONE', #4925, 1000.000000000000000 ) ;
#126191 = ORIENTED_EDGE ( 'NONE', *, *, #65947, .F. ) ;
#126192 = ORIENTED_EDGE ( 'NONE', *, *, #18089, .T. ) ;
#126193 = DIRECTION ( 'NONE',  ( 0.000000000000000000, -0.000000000000000000, 1.000000000000000000 ) ) ;
#126194 = CARTESIAN_POINT ( 'NONE',  ( -8.550000000000014921, 12.50000000000000000, -6.213873640053559022 ) ) ;
#126195 = FACE_OUTER_BOUND ( 'NONE', #63615, .T. ) ;
#126196 = FACE_BOUND ( 'NONE', #15844, .T. ) ;
#126197 = CONICAL_SURFACE ( 'NONE', #69762, 0.1000000000000002554, 0.003490658503988666988 ) ;
#126198 = DIRECTION ( 'NONE',  ( 0.000000000000000000, 0.000000000000000000, 1.000000000000000000 ) ) ;
#126199 = FACE_OUTER_BOUND ( 'NONE', #34008, .T. ) ;
#126200 = DIRECTION ( 'NONE',  ( 0.000000000000000000, 0.000000000000000000, 1.000000000000000000 ) ) ;
#126201 = CARTESIAN_POINT ( 'NONE',  ( -3.550000000000028244, 12.50000000000000000, -1.818653347947326138 ) ) ;
#126202 = EDGE_CURVE ( 'NONE', #40952, #57912, #88453, .T. ) ;
#126203 = AXIS2_PLACEMENT_3D ( 'NONE', #72909, #53285, #23155 ) ;
#126204 = CONICAL_SURFACE ( 'NONE', #25860, 0.1000000000000002554, 0.003490658503988666988 ) ;
#126205 = CARTESIAN_POINT ( 'NONE',  ( 186.2968750003414584, 8.734944146203032389, 5.348610694689227483E-16 ) ) ;
#126206 = LINE ( 'NONE', #37195, #19579 ) ;
#126207 = AXIS2_PLACEMENT_3D ( 'NONE', #52024, #122054, #82781 ) ;
#126208 = CARTESIAN_POINT ( 'NONE',  ( -3.350000000000028955, 2.500000000000000000, 5.802370205355744659 ) ) ;
#126209 = AXIS2_PLACEMENT_3D ( 'NONE', #46685, #108807, #38830 ) ;
#126210 = CARTESIAN_POINT ( 'NONE',  ( 8.949999999999921130, 2.500000000000000000, 1.818653347947321475 ) ) ;
#126211 = ORIENTED_EDGE ( 'NONE', *, *, #46315, .F. ) ;
#126212 = ORIENTED_EDGE ( 'NONE', *, *, #4, .F. ) ;
#126213 = EDGE_LOOP ( 'NONE', ( #67943, #89838, #101368, #68786 ) ) ;
#126214 = ORIENTED_EDGE ( 'NONE', *, *, #124463, .T. ) ;
#126215 = EDGE_CURVE ( 'NONE', #5786, #121359, #65467, .T. ) ;
#126216 = DIRECTION ( 'NONE',  ( 0.000000000000000000, 0.000000000000000000, 1.000000000000000000 ) ) ;
#126217 = EDGE_CURVE ( 'NONE', #51195, #65955, #37070, .T. ) ;
#126218 = FACE_BOUND ( 'NONE', #45102, .T. ) ;
#126219 = CARTESIAN_POINT ( 'NONE',  ( 2.299999999999949640, 2.500000000000000000, -4.776537180435977525 ) ) ;
#126220 = CARTESIAN_POINT ( 'NONE',  ( 129.5000000000000000, 0.6250000000000000000, 7.634788798650556707 ) ) ;
#126222 = VERTEX_POINT ( 'NONE', #36434 ) ;
#126221 = AXIS2_PLACEMENT_3D ( 'NONE', #31323, #72530, #111122 ) ;
#126224 = VECTOR ( 'NONE', #115770, 1000.000000000000000 ) ;
#126223 = FACE_OUTER_BOUND ( 'NONE', #43493, .T. ) ;
#126225 = EDGE_CURVE ( 'NONE', #7522, #108949, #21570, .T. ) ;
#126226 = FACE_BOUND ( 'NONE', #52127, .T. ) ;
#126227 = ORIENTED_EDGE ( 'NONE', *, *, #16843, .T. ) ;
#126228 = DIRECTION ( 'NONE',  ( -0.000000000000000000, -1.000000000000000000, -0.000000000000000000 ) ) ;
#126229 = CARTESIAN_POINT ( 'NONE',  ( 5.599999999999933031, 2.500000000000000000, 0.4464101615137735513 ) ) ;
#126230 = VECTOR ( 'NONE', #29751, 1000.000000000000000 ) ;
#126231 = AXIS2_PLACEMENT_3D ( 'NONE', #100540, #29878, #1055 ) ;
#126232 = AXIS2_PLACEMENT_3D ( 'NONE', #21420, #86719, #118753 ) ;
#126233 = VECTOR ( 'NONE', #102448, 1000.000000000000000 ) ;
#126234 = VECTOR ( 'NONE', #78009, 1000.000000000000000 ) ;
#126235 = ORIENTED_EDGE ( 'NONE', *, *, #46908, .F. ) ;
#126236 = CARTESIAN_POINT ( 'NONE',  ( -11.44999999999999751, 2.500000000000000000, 2.611473670974873151 ) ) ;
#126237 = CARTESIAN_POINT ( 'NONE',  ( 0.3999999999999555023, 12.50000000000000000, 4.330127018922196314 ) ) ;
#126239 = EDGE_LOOP ( 'NONE', ( #121766, #72502 ) ) ;
#126238 = AXIS2_PLACEMENT_3D ( 'NONE', #86350, #74613, #35978 ) ;
#126240 = VECTOR ( 'NONE', #119284, 1000.000000000000000 ) ;
#126241 = DIRECTION ( 'NONE',  ( -0.000000000000000000, -1.000000000000000000, -0.000000000000000000 ) ) ;
#126242 = FACE_OUTER_BOUND ( 'NONE', #8176, .T. ) ;
#126243 = VERTEX_POINT ( 'NONE', #87433 ) ;
#126244 = DIRECTION ( 'NONE',  ( -0.000000000000000000, 1.000000000000000000, -0.000000000000000000 ) ) ;
#126246 = ORIENTED_EDGE ( 'NONE', *, *, #111164, .T. ) ;
#126245 = AXIS2_PLACEMENT_3D ( 'NONE', #91683, #110669, #51133 ) ;
#126247 = EDGE_LOOP ( 'NONE', ( #1090, #7880, #126942, #103847 ) ) ;
#126248 = DIRECTION ( 'NONE',  ( 0.000000000000000000, 1.000000000000000000, 0.000000000000000000 ) ) ;
#126249 = ORIENTED_EDGE ( 'NONE', *, *, #15606, .T. ) ;
#126250 = CARTESIAN_POINT ( 'NONE',  ( -4.150000000000024336, 2.500000000000000000, -2.165063509461101710 ) ) ;
#126251 = CARTESIAN_POINT ( 'NONE',  ( 13.34999999999990017, 12.50000000000000000, 2.792790559304612064 ) ) ;
#126252 = EDGE_CURVE ( 'NONE', #36118, #7221, #65170, .T. ) ;
#126253 = ORIENTED_EDGE ( 'NONE', *, *, #51344, .F. ) ;
#126254 = DIRECTION ( 'NONE',  ( 0.000000000000000000, 0.000000000000000000, 1.000000000000000000 ) ) ;
#126255 = DIRECTION ( 'NONE',  ( 0.000000000000000000, 0.000000000000000000, 1.000000000000000000 ) ) ;
#126256 = CARTESIAN_POINT ( 'NONE',  ( 7.499999999999961808, 12.50000000000000000, -4.330127018922201643 ) ) ;
#126257 =( BOUNDED_CURVE ( )  B_SPLINE_CURVE ( 2, ( #73260, #50394, #120433, #111904, #23508, #63447, #644 ),
 .UNSPECIFIED., .F., .F. ) 
 B_SPLINE_CURVE_WITH_KNOTS ( ( 3, 2, 2, 3 ),
 ( 0.1428571428571429880, 0.1666666666666668239, 0.1904761904761906322, 0.2142857142857144681 ),
 .UNSPECIFIED. ) 
 CURVE ( )  GEOMETRIC_REPRESENTATION_ITEM ( )  RATIONAL_B_SPLINE_CURVE ( ( 0.9999999999999992228, 0.8660254037844394848, 1.000000000000000000, 0.8660254037844387076, 1.000000000000000000, 0.8660254037844375974, 1.000000000000001110 ) ) 
 REPRESENTATION_ITEM ( '' )  );
#126258 = CARTESIAN_POINT ( 'NONE',  ( -0.8500000000000382805, 12.50000000000000000, -2.922977105672691422 ) ) ;
#126260 = EDGE_CURVE ( 'NONE', #38409, #6262, #16741, .T. ) ;
#126259 = CARTESIAN_POINT ( 'NONE',  ( -1.650000000000034772, 12.50000000000000000, 2.165063509461097713 ) ) ;
#126261 = DIRECTION ( 'NONE',  ( -1.000000000000000000, 0.000000000000000000, 7.228014483236698281E-17 ) ) ;
#126262 = EDGE_CURVE ( 'NONE', #14356, #27444, #46885, .T. ) ;
#126263 = AXIS2_PLACEMENT_3D ( 'NONE', #68718, #59585, #9806 ) ;
#126264 = ORIENTED_EDGE ( 'NONE', *, *, #95996, .F. ) ;
#126265 = EDGE_LOOP ( 'NONE', ( #49017, #110859, #80902, #18394 ) ) ;
#126266 = CARTESIAN_POINT ( 'NONE',  ( 5.649999999999934630, 12.50000000000000000, -2.576566944158915184 ) ) ;
#126267 = DIRECTION ( 'NONE',  ( -0.000000000000000000, -1.000000000000000000, -0.000000000000000000 ) ) ;
#126268 = ADVANCED_FACE ( 'NONE', ( #77611 ), #108369, .T. ) ;
#126269 = DIRECTION ( 'NONE',  ( -0.000000000000000000, -1.000000000000000000, -0.000000000000000000 ) ) ;
#126271 = VERTEX_POINT ( 'NONE', #8863 ) ;
#126270 = ORIENTED_EDGE ( 'NONE', *, *, #69046, .F. ) ;
#126272 = EDGE_CURVE ( 'NONE', #113921, #99720, #9030, .T. ) ;
#126273 = ORIENTED_EDGE ( 'NONE', *, *, #2756, .T. ) ;
#126274 = EDGE_CURVE ( 'NONE', #105841, #9122, #111438, .T. ) ;
#126275 = DIRECTION ( 'NONE',  ( -0.000000000000000000, 1.000000000000000000, -0.000000000000000000 ) ) ;
#126276 = AXIS2_PLACEMENT_3D ( 'NONE', #104789, #113993, #3385 ) ;
#126277 = CARTESIAN_POINT ( 'NONE',  ( 0.000000000000000000, 0.000000000000000000, -5.000000000000004441 ) ) ;
#126278 = CONICAL_SURFACE ( 'NONE', #30142, 0.09999999999999982514, 0.003490658503988666988 ) ;
#126279 = DIRECTION ( 'NONE',  ( 0.000000000000000000, 0.000000000000000000, 1.000000000000000000 ) ) ;
#126280 = ITEM_DEFINED_TRANSFORMATION ( 'NONE', 'NONE', #2379,  #108296 ) ;
#126281 = EDGE_CURVE ( 'NONE', #108388, #107957, #63142, .T. ) ;
#126282 = CARTESIAN_POINT ( 'NONE',  ( -14.14999999999998614, 2.500000000000000000, -2.857883832488651521 ) ) ;
#126283 = DIRECTION ( 'NONE',  ( 0.000000000000000000, 0.000000000000000000, -1.000000000000000000 ) ) ;
#126284 = CARTESIAN_POINT ( 'NONE',  ( 149.5981739382431783, 2.500000000000000000, -1.703575533167231537 ) ) ;
#126285 = DIRECTION ( 'NONE',  ( 0.000000000000000000, 0.000000000000000000, 1.000000000000000000 ) ) ;
#126286 = CARTESIAN_POINT ( 'NONE',  ( 11.64999999999990443, 2.500000000000000000, -7.088010851410853519 ) ) ;
#126287 = VECTOR ( 'NONE', #75645, 1000.000000000000000 ) ;
#126289 = EDGE_CURVE ( 'NONE', #41760, #69690, #95976, .T. ) ;
#126288 = CARTESIAN_POINT ( 'NONE',  ( -0.2000000000000339284, 12.50000000000000000, -0.3464101615137759604 ) ) ;
#126290 = ORIENTED_EDGE ( 'NONE', *, *, #43879, .F. ) ;
#126291 = CONICAL_SURFACE ( 'NONE', #69757, 0.09999999999999982514, 0.003490658503988666988 ) ;
#126292 = CARTESIAN_POINT ( 'NONE',  ( 5.799999999999933209, 2.500000000000000000, -2.385244779468109755E-15 ) ) ;
#126293 = ORIENTED_EDGE ( 'NONE', *, *, #90511, .T. ) ;
#126294 = VERTEX_POINT ( 'NONE', #123818 ) ;
#126295 = FACE_OUTER_BOUND ( 'NONE', #104441, .T. ) ;
#126296 = LINE ( 'NONE', #5212, #36377 ) ;
#126297 = PLANE ( 'NONE',  #80092 ) ;
#126298 = DIRECTION ( 'NONE',  ( -0.000000000000000000, -1.000000000000000000, -0.000000000000000000 ) ) ;
#126299 = CARTESIAN_POINT ( 'NONE',  ( 185.2083333333333144, -4.445597072760163471, -7.699999999999919353 ) ) ;
#126300 = CIRCLE ( 'NONE', #53138, 0.09999999999999982514 ) ;
#126301 = PLANE ( 'NONE',  #59543 ) ;
#126302 = AXIS2_PLACEMENT_3D ( 'NONE', #83101, #32076, #123020 ) ;
#126303 = AXIS2_PLACEMENT_3D ( 'NONE', #118626, #37512, #28979 ) ;
#126304 = DIRECTION ( 'NONE',  ( 0.000000000000000000, 0.000000000000000000, 1.000000000000000000 ) ) ;
#126305 = ORIENTED_EDGE ( 'NONE', *, *, #8570, .F. ) ;
#126306 = CARTESIAN_POINT ( 'NONE',  ( 0.8499999999999557909, 2.500000000000000000, -7.188010851410854052 ) ) ;
#126307 = AXIS2_PLACEMENT_3D ( 'NONE', #66965, #77450, #68263 ) ;
#126308 = AXIS2_PLACEMENT_3D ( 'NONE', #66470, #35733, #114285 ) ;
#126309 = CARTESIAN_POINT ( 'NONE',  ( 186.7500000000000000, 9.429780353434619030E-16, -7.700000000000000178 ) ) ;
#126310 = ORIENTED_EDGE ( 'NONE', *, *, #83296, .F. ) ;
#126311 = ORIENTED_EDGE ( 'NONE', *, *, #77752, .F. ) ;
#126312 = VERTEX_POINT ( 'NONE', #23706 ) ;
#126313 = VERTEX_POINT ( 'NONE', #21783 ) ;
#126314 = DIRECTION ( 'NONE',  ( 0.000000000000000000, -0.000000000000000000, 1.000000000000000000 ) ) ;
#126315 = DIRECTION ( 'NONE',  ( -0.000000000000000000, 1.000000000000000000, -0.000000000000000000 ) ) ;
#126316 = EDGE_LOOP ( 'NONE', ( #111626, #102442 ) ) ;
#126317 = DIRECTION ( 'NONE',  ( 0.000000000000000000, -0.000000000000000000, 1.000000000000000000 ) ) ;
#126318 = EDGE_CURVE ( 'NONE', #128359, #71554, #1472, .T. ) ;
#126319 = CARTESIAN_POINT ( 'NONE',  ( 2.500000000000002220, 0.9166666666666682950, -9.999999999999998224 ) ) ;
#126320 = VECTOR ( 'NONE', #47746, 1000.000000000000000 ) ;
#126321 = AXIS2_PLACEMENT_3D ( 'NONE', #73176, #12312, #102621 ) ;
#126322 = CARTESIAN_POINT ( 'NONE',  ( -0.8500000000000386136, 12.50000000000000000, 1.472243186433545459 ) ) ;
#126323 = ORIENTED_EDGE ( 'NONE', *, *, #14812, .T. ) ;
#126324 = CIRCLE ( 'NONE', #40665, 0.06509327318403745899 ) ;
#126325 = CIRCLE ( 'NONE', #88663, 0.9999999999999998890 ) ;
#126326 = DIRECTION ( 'NONE',  ( -0.000000000000000000, -1.000000000000000000, -0.000000000000000000 ) ) ;
#126328 = EDGE_CURVE ( 'NONE', #63386, #31251, #15278, .T. ) ;
#126327 = DIRECTION ( 'NONE',  ( 0.000000000000000000, 0.000000000000000000, -1.000000000000000000 ) ) ;
#126329 = ORIENTED_EDGE ( 'NONE', *, *, #70900, .T. ) ;
#126330 = CONICAL_SURFACE ( 'NONE', #69893, 0.09999999999999999167, 0.003490658503988666988 ) ;
#126331 = AXIS2_PLACEMENT_3D ( 'NONE', #73159, #103268, #113069 ) ;
#126332 = VECTOR ( 'NONE', #12128, 1000.000000000000000 ) ;
#126333 = ORIENTED_EDGE ( 'NONE', *, *, #109684, .T. ) ;
#126334 = VERTEX_POINT ( 'NONE', #51253 ) ;
#126335 = DIRECTION ( 'NONE',  ( -0.000000000000000000, -1.000000000000000000, -0.000000000000000000 ) ) ;
#126336 = CARTESIAN_POINT ( 'NONE',  ( -4.800000000000026468, 12.50000000000000000, -4.676537180435978769 ) ) ;
#126337 = AXIS2_PLACEMENT_3D ( 'NONE', #20092, #72418, #90094 ) ;
#126338 = VECTOR ( 'NONE', #20208, 1000.000000000000000 ) ;
#126339 = AXIS2_PLACEMENT_3D ( 'NONE', #47839, #18357, #17701 ) ;
#126340 = CIRCLE ( 'NONE', #80284, 0.06509327318403745899 ) ;
#126341 = VERTEX_POINT ( 'NONE', #23060 ) ;
#126342 = CARTESIAN_POINT ( 'NONE',  ( -4.350000000000023626, 2.500000000000000000, 1.818653347947321475 ) ) ;
#126343 = DIRECTION ( 'NONE',  ( 0.000000000000000000, -0.9999939076577903929, 0.003490651415223739937 ) ) ;
#126344 = LINE ( 'NONE', #16982, #121468 ) ;
#126345 = LINE ( 'NONE', #76593, #23221 ) ;
#126346 = ORIENTED_EDGE ( 'NONE', *, *, #27051, .F. ) ;
#126347 = CARTESIAN_POINT ( 'NONE',  ( -6.450000000000017941, 2.500000000000000000, -2.511473670974877948 ) ) ;
#126348 = ORIENTED_EDGE ( 'NONE', *, *, #61581, .F. ) ;
#126349 = EDGE_LOOP ( 'NONE', ( #78107, #114139 ) ) ;
#126350 = ORIENTED_EDGE ( 'NONE', *, *, #91674, .F. ) ;
#126351 = CARTESIAN_POINT ( 'NONE',  ( 2.099999999999950351, 12.50000000000000000, -0.7579135962115916003 ) ) ;
#126352 = FACE_BOUND ( 'NONE', #122442, .T. ) ;
#126353 = FACE_OUTER_BOUND ( 'NONE', #10486, .T. ) ;
#126354 = AXIS2_PLACEMENT_3D ( 'NONE', #90063, #50806, #80268 ) ;
#126355 = DIRECTION ( 'NONE',  ( -0.000000000000000000, 1.000000000000000000, -0.000000000000000000 ) ) ;
#126356 = DIRECTION ( 'NONE',  ( 0.000000000000000000, 1.000000000000000000, 0.000000000000000000 ) ) ;
#126357 = ADVANCED_FACE ( 'NONE', ( #82636 ), #32899, .T. ) ;
#126358 = VERTEX_POINT ( 'NONE', #93735 ) ;
#126359 = CARTESIAN_POINT ( 'NONE',  ( 108.0000000000000142, 8.500000000000000000, 0.000000000000000000 ) ) ;
#126360 = DIRECTION ( 'NONE',  ( 0.000000000000000000, 0.000000000000000000, -1.000000000000000000 ) ) ;
#126361 = DIRECTION ( 'NONE',  ( 0.000000000000000000, 0.000000000000000000, -1.000000000000000000 ) ) ;
#126362 = FACE_OUTER_BOUND ( 'NONE', #60990, .T. ) ;
#126363 = ORIENTED_EDGE ( 'NONE', *, *, #80016, .T. ) ;
#126364 = CIRCLE ( 'NONE', #30242, 7.500000000000000000 ) ;
#126365 = EDGE_CURVE ( 'NONE', #61083, #2989, #112737, .T. ) ;
#126366 = AXIS2_PLACEMENT_3D ( 'NONE', #1910, #52964, #54248 ) ;
#126367 = LINE ( 'NONE', #36709, #36429 ) ;
#126368 = DIRECTION ( 'NONE',  ( 0.000000000000000000, 0.000000000000000000, 1.000000000000000000 ) ) ;
#126369 = ORIENTED_EDGE ( 'NONE', *, *, #342, .F. ) ;
#126370 = EDGE_CURVE ( 'NONE', #67997, #29869, #71436, .T. ) ;
#126371 = PLANE ( 'NONE',  #114996 ) ;
#126373 = EDGE_CURVE ( 'NONE', #59250, #89734, #121713, .T. ) ;
#126372 = DIRECTION ( 'NONE',  ( 0.000000000000000000, 0.000000000000000000, 1.000000000000000000 ) ) ;
#126374 = FACE_BOUND ( 'NONE', #120449, .T. ) ;
#126375 = DIRECTION ( 'NONE',  ( 0.000000000000000000, 0.000000000000000000, -1.000000000000000000 ) ) ;
#126376 = CONICAL_SURFACE ( 'NONE', #38575, 0.09999999999999982514, 0.003490658503988666988 ) ;
#126377 = ORIENTED_EDGE ( 'NONE', *, *, #17170, .T. ) ;
#126378 = CARTESIAN_POINT ( 'NONE',  ( -0.6500000000000403233, 2.500000000000000000, 6.148780366869520009 ) ) ;
#126379 = DIRECTION ( 'NONE',  ( 0.000000000000000000, 0.000000000000000000, -1.000000000000000000 ) ) ;
#126380 = EDGE_CURVE ( 'NONE', #56480, #110736, #11297, .T. ) ;
#126381 = VERTEX_POINT ( 'NONE', #72810 ) ;
#126382 = ORIENTED_EDGE ( 'NONE', *, *, #120544, .F. ) ;
#126383 = EDGE_CURVE ( 'NONE', #13274, #30016, #94528, .T. ) ;
#126384 = CARTESIAN_POINT ( 'NONE',  ( 186.8333333333333144, 6.668395609140177704, -3.849999999999998312 ) ) ;
#126385 = VERTEX_POINT ( 'NONE', #12578 ) ;
#126386 = CARTESIAN_POINT ( 'NONE',  ( 11.84999999999990727, 12.50000000000000000, -2.511473670974877948 ) ) ;
#126387 = FACE_OUTER_BOUND ( 'NONE', #92309, .T. ) ;
#126388 = AXIS2_PLACEMENT_3D ( 'NONE', #119761, #51684, #30119 ) ;
#126389 = VECTOR ( 'NONE', #51196, 1000.000000000000000 ) ;
#126390 = DIRECTION ( 'NONE',  ( 0.000000000000000000, 0.000000000000000000, 1.000000000000000000 ) ) ;
#126391 = AXIS2_PLACEMENT_3D ( 'NONE', #36086, #114631, #26271 ) ;
#126392 = DIRECTION ( 'NONE',  ( 0.000000000000000000, -0.000000000000000000, 1.000000000000000000 ) ) ;
#126393 = CIRCLE ( 'NONE', #40738, 0.1000000000000002554 ) ;
#126394 = ORIENTED_EDGE ( 'NONE', *, *, #78037, .F. ) ;
#126395 = CARTESIAN_POINT ( 'NONE',  ( -10.40000000000000213, 2.500000000000000000, 4.430127018922196847 ) ) ;
#126396 = DIRECTION ( 'NONE',  ( 0.000000000000000000, 1.000000000000000000, 0.000000000000000000 ) ) ;
#126397 = CARTESIAN_POINT ( 'NONE',  ( -6.650000000000014566, 12.50000000000000000, 1.472243186433545459 ) ) ;
#126398 = DIRECTION ( 'NONE',  ( -4.274815082592931898E-19, -0.9999939076577903929, -0.003490651415223739937 ) ) ;
#126399 = ORIENTED_EDGE ( 'NONE', *, *, #17496, .T. ) ;
#126400 = DIRECTION ( 'NONE',  ( 0.000000000000000000, -0.000000000000000000, 1.000000000000000000 ) ) ;
#126401 = VERTEX_POINT ( 'NONE', #43361 ) ;
#126402 = DIRECTION ( 'NONE',  ( 0.000000000000000000, 0.000000000000000000, -1.000000000000000000 ) ) ;
#126403 = CARTESIAN_POINT ( 'NONE',  ( 11.89999999999990443, 12.50000000000000000, -0.3464101615137782364 ) ) ;
#126404 = ORIENTED_EDGE ( 'NONE', *, *, #58885, .F. ) ;
#126405 = DIRECTION ( 'NONE',  ( 0.000000000000000000, 1.000000000000000000, 0.000000000000000000 ) ) ;
#126406 = CARTESIAN_POINT ( 'NONE',  ( 17.50000000000000000, -2.499999999999999556, -3.666666666666664298 ) ) ;
#126407 = EDGE_CURVE ( 'NONE', #44421, #8315, #75745, .T. ) ;
#126408 = DIRECTION ( 'NONE',  ( -0.000000000000000000, -1.000000000000000000, -0.000000000000000000 ) ) ;
#126410 = DIRECTION ( 'NONE',  ( 0.000000000000000000, 0.000000000000000000, 1.000000000000000000 ) ) ;
#126409 = CONICAL_SURFACE ( 'NONE', #113896, 0.09999999999999999167, 0.003490658503988666988 ) ;
#126411 = EDGE_LOOP ( 'NONE', ( #116229, #81871 ) ) ;
#126412 = AXIS2_PLACEMENT_3D ( 'NONE', #82200, #54028, #33738 ) ;
#126413 = DIRECTION ( 'NONE',  ( 0.000000000000000000, 0.000000000000000000, -1.000000000000000000 ) ) ;
#126414 = CARTESIAN_POINT ( 'NONE',  ( -6.650000000000019007, 12.50000000000000000, -5.802370205355749988 ) ) ;
#126415 = CONICAL_SURFACE ( 'NONE', #30284, 0.1000000000000002554, 0.003490658503988666988 ) ;
#126416 = CIRCLE ( 'NONE', #68004, 2.250000000000001776 ) ;
#126417 = CARTESIAN_POINT ( 'NONE',  ( 186.1927083336747160, 6.551208109652275624, -3.782341765624998686 ) ) ;
#126418 = FACE_OUTER_BOUND ( 'NONE', #36582, .T. ) ;
#126419 = CARTESIAN_POINT ( 'NONE',  ( 10.39999999999991509, 2.500000000000000000, -0.7928203230275543412 ) ) ;
#126420 = EDGE_CURVE ( 'NONE', #43475, #99497, #111419, .T. ) ;
#126421 = CONICAL_SURFACE ( 'NONE', #111848, 0.09999999999999999167, 0.003490658503988666988 ) ;
#126422 = VERTEX_POINT ( 'NONE', #101631 ) ;
#126424 = ORIENTED_EDGE ( 'NONE', *, *, #46174, .T. ) ;
#126423 = AXIS2_PLACEMENT_3D ( 'NONE', #105964, #96137, #24827 ) ;
#126426 = LINE ( 'NONE', #45294, #99321 ) ;
#126425 = CIRCLE ( 'NONE', #13534, 0.1000000000000000056 ) ;
#126427 = ORIENTED_EDGE ( 'NONE', *, *, #15445, .F. ) ;
#126428 = DIRECTION ( 'NONE',  ( 0.000000000000000000, 0.000000000000000000, 1.000000000000000000 ) ) ;
#126429 = ADVANCED_FACE ( 'NONE', ( #51884 ), #90307, .T. ) ;
#126432 = EDGE_LOOP ( 'NONE', ( #128202, #71915 ) ) ;
#126431 = VERTEX_POINT ( 'NONE', #2114 ) ;
#126430 = CIRCLE ( 'NONE', #59647, 0.06509327318403745899 ) ;
#126433 = VERTEX_POINT ( 'NONE', #83278 ) ;
#126434 = EDGE_CURVE ( 'NONE', #9737, #104138, #23512, .T. ) ;
#126435 = DIRECTION ( 'NONE',  ( -0.000000000000000000, -0.000000000000000000, -1.000000000000000000 ) ) ;
#126436 = EDGE_CURVE ( 'NONE', #86367, #11533, #98723, .T. ) ;
#126437 = CIRCLE ( 'NONE', #47018, 0.1000000000000002554 ) ;
#126439 = AXIS2_PLACEMENT_3D ( 'NONE', #27362, #80201, #87580 ) ;
#126438 = CARTESIAN_POINT ( 'NONE',  ( -6.900000000000019007, 2.500000000000000000, -0.3464101615137783474 ) ) ;
#126440 = CARTESIAN_POINT ( 'NONE',  ( 115.5000000000000000, -5.000000000000000000, -1.999999999999997335 ) ) ;
#126441 = EDGE_CURVE ( 'NONE', #34192, #29616, #102941, .T. ) ;
#126442 = DIRECTION ( 'NONE',  ( 0.000000000000000000, 0.000000000000000000, 1.000000000000000000 ) ) ;
#126443 = DIRECTION ( 'NONE',  ( 0.000000000000000000, -0.9999939076577903929, 0.003490651415223739937 ) ) ;
#126444 = CIRCLE ( 'NONE', #30308, 0.09999999999999982514 ) ;
#126445 = DIRECTION ( 'NONE',  ( 0.000000000000000000, 1.000000000000000000, 0.000000000000000000 ) ) ;
#126446 = ORIENTED_EDGE ( 'NONE', *, *, #13020, .F. ) ;
#126448 = ADVANCED_FACE ( 'NONE', ( #72172 ), #88248, .T. ) ;
#126447 = CARTESIAN_POINT ( 'NONE',  ( 1.899999999999951283, 12.50000000000000000, -3.983716857408426293 ) ) ;
#126449 = ORIENTED_EDGE ( 'NONE', *, *, #53733, .T. ) ;
#126450 = ADVANCED_FACE ( 'NONE', ( #83898 ), #96568, .T. ) ;
#126451 = EDGE_LOOP ( 'NONE', ( #117892, #20403, #79853, #99678 ) ) ;
#126452 = EDGE_LOOP ( 'NONE', ( #42521, #58129 ) ) ;
#126453 = ORIENTED_EDGE ( 'NONE', *, *, #110931, .F. ) ;
#126454 = CARTESIAN_POINT ( 'NONE',  ( -8.150000000000009237, 12.50000000000000000, 6.213873640053558134 ) ) ;
#126455 = VERTEX_POINT ( 'NONE', #4675 ) ;
#126456 = ORIENTED_EDGE ( 'NONE', *, *, #87514, .T. ) ;
#126457 = AXIS2_PLACEMENT_3D ( 'NONE', #88551, #100943, #58475 ) ;
#126458 = CARTESIAN_POINT ( 'NONE',  ( -13.14999999999999147, 12.50000000000000000, 2.511473670974877503 ) ) ;
#126459 = DIRECTION ( 'NONE',  ( 0.000000000000000000, 0.000000000000000000, 1.000000000000000000 ) ) ;
#126460 = DIRECTION ( 'NONE',  ( 0.000000000000000000, -0.000000000000000000, 1.000000000000000000 ) ) ;
#126461 = DIRECTION ( 'NONE',  ( 0.000000000000000000, 1.000000000000000000, 0.000000000000000000 ) ) ;
#126462 = DIRECTION ( 'NONE',  ( -0.000000000000000000, -1.000000000000000000, -0.000000000000000000 ) ) ;
#126463 = EDGE_LOOP ( 'NONE', ( #127282, #71311 ) ) ;
#126464 = DIRECTION ( 'NONE',  ( 0.000000000000000000, 0.000000000000000000, -1.000000000000000000 ) ) ;
#126465 = CIRCLE ( 'NONE', #72188, 0.06509327318403745899 ) ;
#126466 = VECTOR ( 'NONE', #78421, 1000.000000000000000 ) ;
#126467 = ORIENTED_EDGE ( 'NONE', *, *, #30716, .T. ) ;
#126468 = DIRECTION ( 'NONE',  ( 0.000000000000000000, 0.000000000000000000, 1.000000000000000000 ) ) ;
#126469 = ORIENTED_EDGE ( 'NONE', *, *, #91837, .T. ) ;
#126470 = DIRECTION ( 'NONE',  ( -4.274815082592931898E-19, -0.9999939076577903929, -0.003490651415223739937 ) ) ;
#126471 = ORIENTED_EDGE ( 'NONE', *, *, #52939, .F. ) ;
#126472 = ORIENTED_EDGE ( 'NONE', *, *, #115591, .T. ) ;
#126473 = CARTESIAN_POINT ( 'NONE',  ( 8.749999999999957367, 2.500000000000000000, -6.495190528383302464 ) ) ;
#126474 = DIRECTION ( 'NONE',  ( -0.000000000000000000, -1.000000000000000000, -0.000000000000000000 ) ) ;
#126475 = CARTESIAN_POINT ( 'NONE',  ( -13.34999999999999076, 2.500000000000000000, 2.957883832488652942 ) ) ;
#126476 = ADVANCED_FACE ( 'NONE', ( #45934 ), #57010, .T. ) ;
#126477 = DIRECTION ( 'NONE',  ( -0.000000000000000000, -1.000000000000000000, -0.000000000000000000 ) ) ;
#126478 = CIRCLE ( 'NONE', #5266, 0.1000000000000002554 ) ;
#126479 = DIRECTION ( 'NONE',  ( 0.000000000000000000, -0.9999939076577903929, 0.003490651415223739937 ) ) ;
#126480 = ORIENTED_EDGE ( 'NONE', *, *, #98655, .T. ) ;
#126481 = FACE_OUTER_BOUND ( 'NONE', #105931, .T. ) ;
#126482 = DIRECTION ( 'NONE',  ( 0.000000000000000000, 0.000000000000000000, 1.000000000000000000 ) ) ;
#126483 = DIRECTION ( 'NONE',  ( 0.000000000000000000, 0.000000000000000000, -1.000000000000000000 ) ) ;
#126484 = FACE_OUTER_BOUND ( 'NONE', #115028, .T. ) ;
#126486 = EDGE_CURVE ( 'NONE', #35924, #66203, #117482, .T. ) ;
#126485 = DIRECTION ( 'NONE',  ( -0.000000000000000000, 1.000000000000000000, -0.000000000000000000 ) ) ;
#126487 = VERTEX_POINT ( 'NONE', #25618 ) ;
#126488 = AXIS2_PLACEMENT_3D ( 'NONE', #7548, #40920, #59913 ) ;
#126489 = AXIS2_PLACEMENT_3D ( 'NONE', #43509, #83428, #91298 ) ;
#126490 = EDGE_LOOP ( 'NONE', ( #9823, #92778, #99676, #111066 ) ) ;
#126491 = PLANE ( 'NONE',  #40157 ) ;
#126492 = ORIENTED_EDGE ( 'NONE', *, *, #119633, .T. ) ;
#126493 = DIRECTION ( 'NONE',  ( -0.000000000000000000, 1.000000000000000000, -0.000000000000000000 ) ) ;
#126494 = CARTESIAN_POINT ( 'NONE',  ( 11.24999999999991118, 12.50000000000000000, 5.802370205355744659 ) ) ;
#126495 = EDGE_LOOP ( 'NONE', ( #124688, #40633, #71850, #53133 ) ) ;
#126496 = CARTESIAN_POINT ( 'NONE',  ( 184.8333333333333144, 6.668395609140177704, -3.849999999999998312 ) ) ;
#126497 = DIRECTION ( 'NONE',  ( 0.000000000000000000, 1.000000000000000000, 0.000000000000000000 ) ) ;
#126498 = CARTESIAN_POINT ( 'NONE',  ( -12.09999999999999609, 12.50000000000000000, -5.022947341949751454 ) ) ;
#126499 = AXIS2_PLACEMENT_3D ( 'NONE', #113224, #105996, #94235 ) ;
#126500 = CARTESIAN_POINT ( 'NONE',  ( 11.64999999999990443, 2.500000000000000000, 2.757883832488649656 ) ) ;
#126501 = ORIENTED_EDGE ( 'NONE', *, *, #35514, .T. ) ;
#126503 = DIRECTION ( 'NONE',  ( 0.000000000000000000, 1.000000000000000000, 0.000000000000000000 ) ) ;
#126502 = AXIS2_PLACEMENT_3D ( 'NONE', #122062, #39653, #101773 ) ;
#126504 = DIRECTION ( 'NONE',  ( -0.000000000000000000, -1.000000000000000000, -0.000000000000000000 ) ) ;
#126505 = AXIS2_PLACEMENT_3D ( 'NONE', #77523, #19911, #97170 ) ;
#126506 = ORIENTED_EDGE ( 'NONE', *, *, #124508, .F. ) ;
#126507 = CIRCLE ( 'NONE', #30379, 0.1000000000000002554 ) ;
#126508 = CARTESIAN_POINT ( 'NONE',  ( 9.999999999999952038, 12.50000000000000000, -2.276824562219559311E-15 ) ) ;
#126509 = CARTESIAN_POINT ( 'NONE',  ( 175.5000000000000000, 0.000000000000000000, -2.000000000000000000 ) ) ;
#126510 = CARTESIAN_POINT ( 'NONE',  ( 3.549999999999940314, 12.50000000000000000, 6.776507416713035248 ) ) ;
#126511 = CONICAL_SURFACE ( 'NONE', #76337, 0.1000000000000002554, 0.003490658503988666988 ) ;
#126512 = CONICAL_SURFACE ( 'NONE', #3185, 0.09999999999999982514, 0.003490658503988666988 ) ;
#126513 = ORIENTED_EDGE ( 'NONE', *, *, #106024, .F. ) ;
#126514 = CIRCLE ( 'NONE', #70080, 0.1000000000000002554 ) ;
#126515 = FACE_OUTER_BOUND ( 'NONE', #99853, .T. ) ;
#126516 = AXIS2_PLACEMENT_3D ( 'NONE', #1071, #41027, #10257 ) ;
#126517 = ORIENTED_EDGE ( 'NONE', *, *, #116074, .F. ) ;
#126518 = PLANE ( 'NONE',  #45872 ) ;
#126519 = DIRECTION ( 'NONE',  ( 0.000000000000000000, 0.000000000000000000, -1.000000000000000000 ) ) ;
#126520 = PLANE ( 'NONE',  #41284 ) ;
#126521 = EDGE_LOOP ( 'NONE', ( #92373, #102304, #58109, #61047 ) ) ;
#126522 = AXIS2_PLACEMENT_3D ( 'NONE', #44191, #104411, #74955 ) ;
#126524 = EDGE_CURVE ( 'NONE', #9000, #35674, #65277, .T. ) ;
#126523 = CIRCLE ( 'NONE', #11501, 0.06509327318403745899 ) ;
#126525 = DIRECTION ( 'NONE',  ( 0.000000000000000000, 0.000000000000000000, -1.000000000000000000 ) ) ;
#126526 = LINE ( 'NONE', #55839, #51616 ) ;
#126527 = AXIS2_PLACEMENT_3D ( 'NONE', #118900, #109053, #19396 ) ;
#126528 = EDGE_LOOP ( 'NONE', ( #91272, #5294, #15597, #96421 ) ) ;
#126529 = EDGE_CURVE ( 'NONE', #107252, #54196, #45288, .T. ) ;
#126530 = ADVANCED_FACE ( 'NONE', ( #44633 ), #114649, .T. ) ;
#126531 = EDGE_LOOP ( 'NONE', ( #55677, #103590, #100765, #40934 ) ) ;
#126532 = CARTESIAN_POINT ( 'NONE',  ( 11.04999999999990834, 12.50000000000000000, -6.841600689897077814 ) ) ;
#126533 = VERTEX_POINT ( 'NONE', #85828 ) ;
#126534 = DIRECTION ( 'NONE',  ( 0.000000000000000000, -0.9999939076577903929, 0.003490651415223739937 ) ) ;
#126535 = DIRECTION ( 'NONE',  ( -0.000000000000000000, 1.000000000000000000, -0.000000000000000000 ) ) ;
#126536 = EDGE_CURVE ( 'NONE', #1046, #22334, #104193, .T. ) ;
#126537 = ADVANCED_FACE ( 'NONE', ( #84557 ), #64263, .T. ) ;
#126538 = ORIENTED_EDGE ( 'NONE', *, *, #90046, .F. ) ;
#126539 = VERTEX_POINT ( 'NONE', #95029 ) ;
#126540 = ADVANCED_FACE ( 'NONE', ( #65555 ), #111233, .T. ) ;
#126541 = CARTESIAN_POINT ( 'NONE',  ( 3.099999999999945466, 2.500000000000000000, -3.883716857408426648 ) ) ;
#126542 = DIRECTION ( 'NONE',  ( -4.274815082592931898E-19, -0.9999939076577903929, -0.003490651415223739937 ) ) ;
#126543 = CIRCLE ( 'NONE', #65985, 0.06509327318403745899 ) ;
#126544 = ORIENTED_EDGE ( 'NONE', *, *, #126845, .F. ) ;
#126545 = DIRECTION ( 'NONE',  ( 0.000000000000000000, 1.000000000000000000, 0.000000000000000000 ) ) ;
#126546 = CARTESIAN_POINT ( 'NONE',  ( -3.350000000000028955, 12.50000000000000000, 2.099970236277060032 ) ) ;
#126547 = CARTESIAN_POINT ( 'NONE',  ( 3.749999999999978684, 12.50000000000000000, -6.430097255199264339 ) ) ;
#126548 = LINE ( 'NONE', #108176, #55072 ) ;
#126549 = CARTESIAN_POINT ( 'NONE',  ( -15.19999999999998153, 12.50000000000000000, -0.3464101615137759604 ) ) ;
#126550 = CIRCLE ( 'NONE', #1150, 0.06509327318403745899 ) ;
#126551 = CARTESIAN_POINT ( 'NONE',  ( 10.84999999999990905, 2.500000000000000000, -6.495190528383302464 ) ) ;
#126552 = AXIS2_PLACEMENT_3D ( 'NONE', #101751, #13991, #103691 ) ;
#126553 = CIRCLE ( 'NONE', #111982, 0.1000000000000000472 ) ;
#126554 = EDGE_LOOP ( 'NONE', ( #100626, #123367 ) ) ;
#126555 = ORIENTED_EDGE ( 'NONE', *, *, #64653, .T. ) ;
#126556 = ORIENTED_EDGE ( 'NONE', *, *, #49599, .F. ) ;
#126557 = ORIENTED_EDGE ( 'NONE', *, *, #20443, .T. ) ;
#126558 = CARTESIAN_POINT ( 'NONE',  ( 6.049999999999935874, 2.500000000000000000, -6.841600689897077814 ) ) ;
#126559 = DIRECTION ( 'NONE',  ( 0.000000000000000000, 0.000000000000000000, 1.000000000000000000 ) ) ;
#126560 = CARTESIAN_POINT ( 'NONE',  ( -1.224646799147353269E-17, 2.500000000000000000, -0.1000000000000000056 ) ) ;
#126561 = EDGE_LOOP ( 'NONE', ( #87908, #80624 ) ) ;
#126562 = FACE_BOUND ( 'NONE', #10376, .T. ) ;
#126563 = DIRECTION ( 'NONE',  ( 0.000000000000000000, 1.000000000000000000, 0.000000000000000000 ) ) ;
#126564 = CARTESIAN_POINT ( 'NONE',  ( 10.84999999999991260, 12.50000000000000000, -2.165063509461101710 ) ) ;
#126565 = AXIS2_PLACEMENT_3D ( 'NONE', #34767, #103493, #3354 ) ;
#126566 = CARTESIAN_POINT ( 'NONE',  ( -1.450000000000036371, 2.500000000000000000, 6.741600689897071952 ) ) ;
#126567 = DIRECTION ( 'NONE',  ( 0.000000000000000000, 1.000000000000000000, 0.000000000000000000 ) ) ;
#126568 = CONICAL_SURFACE ( 'NONE', #38861, 0.09999999999999982514, 0.003490658503988666988 ) ;
#126569 = CARTESIAN_POINT ( 'NONE',  ( 11.64999999999990621, 2.500000000000000000, 6.495190528383297135 ) ) ;
#126570 = DIRECTION ( 'NONE',  ( 0.000000000000000000, -0.000000000000000000, 1.000000000000000000 ) ) ;
#126571 = CARTESIAN_POINT ( 'NONE',  ( -7.300000000000016698, 12.50000000000000000, -0.3464101615137783474 ) ) ;
#126572 = DIRECTION ( 'NONE',  ( 0.000000000000000000, 1.000000000000000000, 0.000000000000000000 ) ) ;
#126573 = CARTESIAN_POINT ( 'NONE',  ( 7.299999999999927880, 2.500000000000000000, -4.576537180435977348 ) ) ;
#126574 = CARTESIAN_POINT ( 'NONE',  ( 6.249999999999967137, 12.50000000000000000, -2.099970236277064473 ) ) ;
#126575 = AXIS2_PLACEMENT_3D ( 'NONE', #14624, #44766, #95149 ) ;
#126576 = EDGE_LOOP ( 'NONE', ( #120111, #48691 ) ) ;
#126577 = VERTEX_POINT ( 'NONE', #54440 ) ;
#126578 = AXIS2_PLACEMENT_3D ( 'NONE', #64414, #76177, #96437 ) ;
#126579 = ORIENTED_EDGE ( 'NONE', *, *, #123626, .T. ) ;
#126580 = VERTEX_POINT ( 'NONE', #26925 ) ;
#126581 = DIRECTION ( 'NONE',  ( 0.000000000000000000, 1.000000000000000000, 0.000000000000000000 ) ) ;
#126582 = EDGE_CURVE ( 'NONE', #90407, #51178, #54814, .T. ) ;
#126583 = CARTESIAN_POINT ( 'NONE',  ( -10.40000000000000213, 12.50000000000000000, -4.330127018922197202 ) ) ;
#126584 = EDGE_CURVE ( 'NONE', #43268, #33034, #35467, .T. ) ;
#126586 = ORIENTED_EDGE ( 'NONE', *, *, #56555, .F. ) ;
#126585 = ORIENTED_EDGE ( 'NONE', *, *, #106676, .F. ) ;
#126587 = VERTEX_POINT ( 'NONE', #116580 ) ;
#126588 = ADVANCED_FACE ( 'NONE', ( #75365 ), #48574, .T. ) ;
#126589 = DIRECTION ( 'NONE',  ( -0.000000000000000000, -1.000000000000000000, -0.000000000000000000 ) ) ;
#126590 = AXIS2_PLACEMENT_3D ( 'NONE', #9705, #129508, #39828 ) ;
#126591 = CARTESIAN_POINT ( 'NONE',  ( 11.75764115780431851, -2.499999999999999112, 7.679135278101805184 ) ) ;
#126592 = DIRECTION ( 'NONE',  ( 0.000000000000000000, 0.000000000000000000, -1.000000000000000000 ) ) ;
#126593 = DIRECTION ( 'NONE',  ( 0.000000000000000000, -0.9999939076577903929, 0.003490651415223739937 ) ) ;
#126594 = ADVANCED_FACE ( 'NONE', ( #36107 ), #86197, .T. ) ;
#126595 = DIRECTION ( 'NONE',  ( -4.274815082592931898E-19, -0.9999939076577903929, -0.003490651415223739937 ) ) ;
#126596 = ADVANCED_FACE ( 'NONE', ( #5975 ), #95666, .T. ) ;
#126597 = AXIS2_PLACEMENT_3D ( 'NONE', #7130, #107279, #37894 ) ;
#126598 = ORIENTED_EDGE ( 'NONE', *, *, #114119, .T. ) ;
#126599 = ADVANCED_FACE ( 'NONE', ( #126418 ), #63231, .T. ) ;
#126600 = EDGE_CURVE ( 'NONE', #71330, #109372, #15076, .T. ) ;
#126601 = EDGE_LOOP ( 'NONE', ( #83544, #43773, #78316, #37739 ) ) ;
#126602 = EDGE_CURVE ( 'NONE', #118967, #17267, #117202, .T. ) ;
#126604 = VERTEX_POINT ( 'NONE', #30161 ) ;
#126603 = CIRCLE ( 'NONE', #70163, 0.06509327318403745899 ) ;
#126605 = ORIENTED_EDGE ( 'NONE', *, *, #52357, .T. ) ;
#126606 = AXIS2_PLACEMENT_3D ( 'NONE', #28442, #119375, #18607 ) ;
#126607 = DIRECTION ( 'NONE',  ( -0.000000000000000000, -1.000000000000000000, -0.000000000000000000 ) ) ;
#126608 = ORIENTED_EDGE ( 'NONE', *, *, #124508, .T. ) ;
#126609 = VERTEX_POINT ( 'NONE', #88401 ) ;
#126610 = EDGE_CURVE ( 'NONE', #19230, #117173, #44357, .T. ) ;
#126611 = CARTESIAN_POINT ( 'NONE',  ( 11.44999999999990514, 12.50000000000000000, 2.511473670974873507 ) ) ;
#126612 = AXIS2_PLACEMENT_3D ( 'NONE', #28907, #6015, #117241 ) ;
#126613 = CARTESIAN_POINT ( 'NONE',  ( -8.749999999999975131, 2.500000000000000000, 2.065063509461097624 ) ) ;
#126614 = DIRECTION ( 'NONE',  ( -0.000000000000000000, -1.000000000000000000, -0.000000000000000000 ) ) ;
#126615 = PLANE ( 'NONE',  #73444 ) ;
#126616 = CONICAL_SURFACE ( 'NONE', #17837, 0.1000000000000002554, 0.003490658503988666988 ) ;
#126617 = FACE_OUTER_BOUND ( 'NONE', #58580, .T. ) ;
#126618 = VERTEX_POINT ( 'NONE', #128371 ) ;
#126619 = LINE ( 'NONE', #35654, #103354 ) ;
#126620 = CONICAL_SURFACE ( 'NONE', #91196, 0.1000000000000000056, 0.003490658503988666988 ) ;
#126621 = CIRCLE ( 'NONE', #72251, 0.09999999999999982514 ) ;
#126622 = ORIENTED_EDGE ( 'NONE', *, *, #5831, .F. ) ;
#126623 = DIRECTION ( 'NONE',  ( -0.000000000000000000, -1.000000000000000000, -0.000000000000000000 ) ) ;
#126624 = CIRCLE ( 'NONE', #70181, 0.1000000000000002554 ) ;
#126625 = ORIENTED_EDGE ( 'NONE', *, *, #14245, .F. ) ;
#126626 = CARTESIAN_POINT ( 'NONE',  ( 108.0000000000000142, 7.119691004531021328, -5.000000000000004441 ) ) ;
#126627 = DIRECTION ( 'NONE',  ( -4.274815082592931898E-19, -0.9999939076577903929, -0.003490651415223739937 ) ) ;
#126628 = CIRCLE ( 'NONE', #107742, 0.1000000000000000056 ) ;
#126629 = ORIENTED_EDGE ( 'NONE', *, *, #2345, .T. ) ;
#126630 = DIRECTION ( 'NONE',  ( 0.000000000000000000, 1.000000000000000000, 0.000000000000000000 ) ) ;
#126631 = FACE_OUTER_BOUND ( 'NONE', #102425, .T. ) ;
#126632 = ORIENTED_EDGE ( 'NONE', *, *, #55855, .F. ) ;
#126633 = CARTESIAN_POINT ( 'NONE',  ( 11.64999999999990443, 12.50000000000000000, 2.857883832488649301 ) ) ;
#126634 = ORIENTED_EDGE ( 'NONE', *, *, #78735, .T. ) ;
#126635 = ORIENTED_EDGE ( 'NONE', *, *, #98185, .F. ) ;
#126636 = FACE_OUTER_BOUND ( 'NONE', #124795, .T. ) ;
#126637 = CARTESIAN_POINT ( 'NONE',  ( 8.549999999999924327, 2.500000000000000000, -6.741600689897077281 ) ) ;
#126638 = CARTESIAN_POINT ( 'NONE',  ( 186.8385416670080872, 6.551208109652274736, 3.782341765625001351 ) ) ;
#126639 = AXIS2_PLACEMENT_3D ( 'NONE', #83108, #122385, #113852 ) ;
#126640 = DIRECTION ( 'NONE',  ( 0.000000000000000000, -1.000000000000000000, 0.000000000000000000 ) ) ;
#126642 = EDGE_CURVE ( 'NONE', #119412, #57054, #84063, .T. ) ;
#126641 = DIRECTION ( 'NONE',  ( 0.000000000000000000, -0.9999939076577903929, 0.003490651415223739937 ) ) ;
#126643 = CARTESIAN_POINT ( 'NONE',  ( -11.84999999999999609, 2.500000000000000000, 6.841600689897072485 ) ) ;
#126644 = CIRCLE ( 'NONE', #49294, 0.09999999999999982514 ) ;
#126645 = CONICAL_SURFACE ( 'NONE', #22198, 0.09999999999999982514, 0.003490658503988666988 ) ;
#126646 = VERTEX_POINT ( 'NONE', #20330 ) ;
#126647 = CIRCLE ( 'NONE', #91131, 0.06509327318403745899 ) ;
#126648 = CARTESIAN_POINT ( 'NONE',  ( 48.83353579394137967, 2.320413785907065485, -5.300554616748716974 ) ) ;
#126649 = AXIS2_PLACEMENT_3D ( 'NONE', #77902, #35423, #37988 ) ;
#126650 = ORIENTED_EDGE ( 'NONE', *, *, #18743, .F. ) ;
#126651 = CARTESIAN_POINT ( 'NONE',  ( -8.950000000000004619, 12.50000000000000000, 6.148780366869520897 ) ) ;
#126652 = DIRECTION ( 'NONE',  ( 0.000000000000000000, 0.000000000000000000, -1.000000000000000000 ) ) ;
#126653 = CARTESIAN_POINT ( 'NONE',  ( 2.699999999999946443, 2.500000000000000000, 0.3464101615137735735 ) ) ;
#126654 = CARTESIAN_POINT ( 'NONE',  ( 8.349999999999919709, 2.500000000000000000, 5.902370205355745192 ) ) ;
#126655 = CARTESIAN_POINT ( 'NONE',  ( 10.59999999999991260, 12.50000000000000000, 0.3464101615137735735 ) ) ;
#126656 = ORIENTED_EDGE ( 'NONE', *, *, #127682, .T. ) ;
#126657 = CIRCLE ( 'NONE', #13764, 0.09999999999999982514 ) ;
#126659 = CONICAL_SURFACE ( 'NONE', #95356, 0.1000000000000002554, 0.003490658503988666988 ) ;
#126658 = AXIS2_PLACEMENT_3D ( 'NONE', #60287, #683, #68783 ) ;
#126660 = CARTESIAN_POINT ( 'NONE',  ( 3.949999999999939782, 2.500000000000000000, 2.511473670974873507 ) ) ;
#126661 = DIRECTION ( 'NONE',  ( 0.000000000000000000, 1.000000000000000000, 0.000000000000000000 ) ) ;
#126662 = ORIENTED_EDGE ( 'NONE', *, *, #6202, .T. ) ;
#126663 = CARTESIAN_POINT ( 'NONE',  ( 3.749999999999942268, 2.500000000000000000, -1.572243186433550211 ) ) ;
#126664 = AXIS2_PLACEMENT_3D ( 'NONE', #26257, #85165, #84522 ) ;
#126665 = AXIS2_PLACEMENT_3D ( 'NONE', #31589, #102265, #72805 ) ;
#126666 = ORIENTED_EDGE ( 'NONE', *, *, #72040, .T. ) ;
#126667 = ORIENTED_EDGE ( 'NONE', *, *, #56497, .T. ) ;
#126668 = DIRECTION ( 'NONE',  ( 0.000000000000000000, 1.000000000000000000, 0.000000000000000000 ) ) ;
#126669 = VERTEX_POINT ( 'NONE', #79887 ) ;
#126670 = CARTESIAN_POINT ( 'NONE',  ( 10.59999999999990905, 12.50000000000000000, -4.676537180435978769 ) ) ;
#126671 = DIRECTION ( 'NONE',  ( -4.274815082592931898E-19, -0.9999939076577903929, -0.003490651415223739937 ) ) ;
#126672 = CARTESIAN_POINT ( 'NONE',  ( 7.899999999999924860, 2.500000000000000000, 3.537306695894645081 ) ) ;
#126673 = ORIENTED_EDGE ( 'NONE', *, *, #122241, .T. ) ;
#126674 = EDGE_CURVE ( 'NONE', #129385, #94750, #56855, .T. ) ;
#126675 = FACE_BOUND ( 'NONE', #121082, .T. ) ;
#126677 = ORIENTED_EDGE ( 'NONE', *, *, #55869, .T. ) ;
#126676 = CARTESIAN_POINT ( 'NONE',  ( -4.600000000000024514, 2.500000000000000000, 0.7928203230275495672 ) ) ;
#126678 = DIRECTION ( 'NONE',  ( -0.000000000000000000, 1.000000000000000000, -0.000000000000000000 ) ) ;
#126679 = EDGE_CURVE ( 'NONE', #107267, #33453, #57681, .T. ) ;
#126680 = DIRECTION ( 'NONE',  ( 0.000000000000000000, -0.000000000000000000, 1.000000000000000000 ) ) ;
#126681 = EDGE_CURVE ( 'NONE', #12101, #62381, #423, .T. ) ;
#126682 = ORIENTED_EDGE ( 'NONE', *, *, #91505, .T. ) ;
#126683 = AXIS2_PLACEMENT_3D ( 'NONE', #3417, #36109, #76023 ) ;
#126684 = EDGE_LOOP ( 'NONE', ( #9208, #33290, #92446, #38038 ) ) ;
#126685 = CIRCLE ( 'NONE', #66037, 0.06509327318403745899 ) ;
#126686 = ORIENTED_EDGE ( 'NONE', *, *, #58168, .F. ) ;
#126687 = DIRECTION ( 'NONE',  ( -0.000000000000000000, 1.000000000000000000, -0.000000000000000000 ) ) ;
#126688 = FACE_OUTER_BOUND ( 'NONE', #12827, .T. ) ;
#126689 = EDGE_CURVE ( 'NONE', #27988, #93997, #4613, .T. ) ;
#126690 = EDGE_CURVE ( 'NONE', #44951, #14578, #110000, .T. ) ;
#126691 = DIRECTION ( 'NONE',  ( 0.000000000000000000, 1.000000000000000000, 0.000000000000000000 ) ) ;
#126692 = EDGE_CURVE ( 'NONE', #4337, #74953, #59135, .T. ) ;
#126693 = FACE_BOUND ( 'NONE', #110848, .T. ) ;
#126695 = ADVANCED_FACE ( 'NONE', ( #89072 ), #9215, .T. ) ;
#126694 = EDGE_LOOP ( 'NONE', ( #64948, #99859, #72643, #99439 ) ) ;
#126696 = EDGE_CURVE ( 'NONE', #5490, #13290, #60278, .T. ) ;
#126697 = CARTESIAN_POINT ( 'NONE',  ( -9.800000000000006040, 2.500000000000000000, 0.2464101615137735679 ) ) ;
#126698 = FACE_OUTER_BOUND ( 'NONE', #27355, .T. ) ;
#126699 = CIRCLE ( 'NONE', #109974, 0.09999999999999982514 ) ;
#126700 = DIRECTION ( 'NONE',  ( 0.000000000000000000, 1.000000000000000000, 0.000000000000000000 ) ) ;
#126701 = FACE_OUTER_BOUND ( 'NONE', #23329, .T. ) ;
#126702 = DIRECTION ( 'NONE',  ( -0.000000000000000000, -1.000000000000000000, -0.000000000000000000 ) ) ;
#126703 = EDGE_CURVE ( 'NONE', #85963, #121068, #117865, .T. ) ;
#126704 = DIRECTION ( 'NONE',  ( 0.000000000000000000, 0.000000000000000000, 1.000000000000000000 ) ) ;
#126705 = CARTESIAN_POINT ( 'NONE',  ( -2.900000000000030553, 2.500000000000000000, 5.022947341949748790 ) ) ;
#126706 = AXIS2_PLACEMENT_3D ( 'NONE', #86543, #7330, #126482 ) ;
#126707 = EDGE_CURVE ( 'NONE', #47870, #101225, #100179, .T. ) ;
#126708 = AXIS2_PLACEMENT_3D ( 'NONE', #87138, #117223, #77968 ) ;
#126709 = VERTEX_POINT ( 'NONE', #79260 ) ;
#126710 = ORIENTED_EDGE ( 'NONE', *, *, #94932, .F. ) ;
#126711 = EDGE_LOOP ( 'NONE', ( #41002, #3870, #116143, #129433 ) ) ;
#126712 = VERTEX_POINT ( 'NONE', #59635 ) ;
#126713 = EDGE_LOOP ( 'NONE', ( #111052, #13607, #54833, #43816 ) ) ;
#126714 = CARTESIAN_POINT ( 'NONE',  ( -10.84999999999999964, 2.500000000000000000, 2.957883832488649389 ) ) ;
#126715 = CARTESIAN_POINT ( 'NONE',  ( 0.6499999999999561684, 2.500000000000000000, -2.611473670974877592 ) ) ;
#126716 = VERTEX_POINT ( 'NONE', #108056 ) ;
#126717 = FACE_BOUND ( 'NONE', #13407, .T. ) ;
#126718 = CARTESIAN_POINT ( 'NONE',  ( 5.849999999999934808, 12.50000000000000000, -5.867463478539787225 ) ) ;
#126719 = CARTESIAN_POINT ( 'NONE',  ( -13.09999999999999254, 2.500000000000000000, -0.2464101615137741230 ) ) ;
#126720 = DIRECTION ( 'NONE',  ( 0.000000000000000000, 0.000000000000000000, 1.000000000000000000 ) ) ;
#126721 = CARTESIAN_POINT ( 'NONE',  ( -1.650000000000034772, 12.50000000000000000, 1.472243186433545459 ) ) ;
#126722 = CARTESIAN_POINT ( 'NONE',  ( -0.8500000000000386136, 12.50000000000000000, 2.857883832488649301 ) ) ;
#126724 = ORIENTED_EDGE ( 'NONE', *, *, #43516, .F. ) ;
#126723 = AXIS2_PLACEMENT_3D ( 'NONE', #12253, #53494, #23359 ) ;
#126725 = CARTESIAN_POINT ( 'NONE',  ( 17.46224679592722495, -2.499999999999374278, 5.244174652594745467 ) ) ;
#126726 = ORIENTED_EDGE ( 'NONE', *, *, #92085, .F. ) ;
#126727 = PRODUCT ( 'Magnetic Levitation Sonic Motor Unit', 'Magnetic Levitation Sonic Motor Unit', '', ( #47723 ) ) ;
#126728 = VECTOR ( 'NONE', #86018, 1000.000000000000000 ) ;
#126729 = VERTEX_POINT ( 'NONE', #99543 ) ;
#126730 = ORIENTED_EDGE ( 'NONE', *, *, #89155, .F. ) ;
#126731 = FACE_OUTER_BOUND ( 'NONE', #40610, .T. ) ;
#126732 = DIRECTION ( 'NONE',  ( 0.000000000000000000, 0.000000000000000000, 1.000000000000000000 ) ) ;
#126733 = CARTESIAN_POINT ( 'NONE',  ( 8.749999999999923617, 12.50000000000000000, -7.122917578226816815 ) ) ;
#126734 = EDGE_CURVE ( 'NONE', #11709, #113, #65364, .T. ) ;
#126735 = EDGE_LOOP ( 'NONE', ( #1681, #111403 ) ) ;
#126736 = CARTESIAN_POINT ( 'NONE',  ( 13.92826132181788346, 2.499999999999999556, -6.790916467785696575 ) ) ;
#126737 = VECTOR ( 'NONE', #72139, 1000.000000000000000 ) ;
#126738 = EDGE_CURVE ( 'NONE', #71628, #127250, #123861, .T. ) ;
#126739 = AXIS2_PLACEMENT_3D ( 'NONE', #112708, #11914, #119948 ) ;
#126740 = DIRECTION ( 'NONE',  ( -0.000000000000000000, 1.000000000000000000, -0.000000000000000000 ) ) ;
#126741 = CIRCLE ( 'NONE', #76649, 0.06509327318403745899 ) ;
#126742 = ADVANCED_FACE ( 'NONE', ( #58335 ), #70074, .T. ) ;
#126743 = DIRECTION ( 'NONE',  ( 0.000000000000000000, -0.9999939076577903929, 0.003490651415223739937 ) ) ;
#126744 = CARTESIAN_POINT ( 'NONE',  ( 185.0312500006828031, 9.429780353434619030E-16, -7.700000000000000178 ) ) ;
#126745 = CARTESIAN_POINT ( 'NONE',  ( 12.29999999999990479, 12.50000000000000000, 4.741630453620009789 ) ) ;
#126746 = DIRECTION ( 'NONE',  ( 0.000000000000000000, 0.000000000000000000, 1.000000000000000000 ) ) ;
#126747 = DIRECTION ( 'NONE',  ( -4.274815082592931898E-19, -0.9999939076577903929, -0.003490651415223739937 ) ) ;
#126748 = EDGE_CURVE ( 'NONE', #102161, #26161, #107135, .T. ) ;
#126749 = VERTEX_POINT ( 'NONE', #102732 ) ;
#126750 = CARTESIAN_POINT ( 'NONE',  ( 11.64999999999990443, 2.500000000000000000, 1.472243186433545459 ) ) ;
#126751 = CIRCLE ( 'NONE', #118328, 0.1000000000000002554 ) ;
#126752 = ADVANCED_FACE ( 'NONE', ( #91640 ), #32743, .F. ) ;
#126753 = VERTEX_POINT ( 'NONE', #40639 ) ;
#126756 = EDGE_CURVE ( 'NONE', #31984, #11223, #111253, .T. ) ;
#126755 = CIRCLE ( 'NONE', #43150, 0.06509327318403745899 ) ;
#126754 = AXIS2_PLACEMENT_3D ( 'NONE', #93432, #94075, #111106 ) ;
#126757 = ORIENTED_EDGE ( 'NONE', *, *, #48388, .F. ) ;
#126758 = DIRECTION ( 'NONE',  ( 0.000000000000000000, -0.000000000000000000, 1.000000000000000000 ) ) ;
#126759 = CARTESIAN_POINT ( 'NONE',  ( 0.3999999999999619971, 2.500000000000000000, 0.09999999999999989453 ) ) ;
#126760 = DIRECTION ( 'NONE',  ( 0.000000000000000000, 1.000000000000000000, 0.000000000000000000 ) ) ;
#126761 = ORIENTED_EDGE ( 'NONE', *, *, #73616, .F. ) ;
#126762 = ADVANCED_FACE ( 'NONE', ( #92943 ), #122402, .T. ) ;
#126763 = ORIENTED_EDGE ( 'NONE', *, *, #104379, .T. ) ;
#126764 = DIRECTION ( 'NONE',  ( 0.000000000000000000, 1.000000000000000000, 0.000000000000000000 ) ) ;
#126765 = CARTESIAN_POINT ( 'NONE',  ( -1.650000000000034772, 2.500000000000000000, 6.595190528383296780 ) ) ;
#126766 = CARTESIAN_POINT ( 'NONE',  ( -5.000000000000022204, 12.50000000000000000, 3.572213422710607489 ) ) ;
#126767 = ORIENTED_EDGE ( 'NONE', *, *, #90846, .T. ) ;
#126768 = ORIENTED_EDGE ( 'NONE', *, *, #114447, .F. ) ;
#126769 = DIRECTION ( 'NONE',  ( 0.000000000000000000, 1.000000000000000000, 0.000000000000000000 ) ) ;
#126770 = ORIENTED_EDGE ( 'NONE', *, *, #40718, .T. ) ;
#126771 = DIRECTION ( 'NONE',  ( -4.274815082592931898E-19, -0.9999939076577903929, -0.003490651415223739937 ) ) ;
#126772 = DIRECTION ( 'NONE',  ( -0.000000000000000000, -1.000000000000000000, -0.000000000000000000 ) ) ;
#126773 = ORIENTED_EDGE ( 'NONE', *, *, #35361, .F. ) ;
#126774 = PLANE ( 'NONE',  #6369 ) ;
#126775 = CARTESIAN_POINT ( 'NONE',  ( -5.850000000000018296, 12.50000000000000000, 2.857883832488649301 ) ) ;
#126776 = DIRECTION ( 'NONE',  ( 0.000000000000000000, 0.000000000000000000, 1.000000000000000000 ) ) ;
#126777 = EDGE_CURVE ( 'NONE', #74876, #10395, #22911, .T. ) ;
#126778 = DIRECTION ( 'NONE',  ( 0.000000000000000000, -0.000000000000000000, 1.000000000000000000 ) ) ;
#126779 = VERTEX_POINT ( 'NONE', #3265 ) ;
#126780 = DIRECTION ( 'NONE',  ( 0.000000000000000000, -0.000000000000000000, 1.000000000000000000 ) ) ;
#126781 = VECTOR ( 'NONE', #64110, 1000.000000000000000 ) ;
#126782 = CIRCLE ( 'NONE', #39068, 0.06509327318403745899 ) ;
#126783 = DIRECTION ( 'NONE',  ( -0.000000000000000000, -1.000000000000000000, -0.000000000000000000 ) ) ;
#126784 = ORIENTED_EDGE ( 'NONE', *, *, #64636, .T. ) ;
#126785 = ORIENTED_EDGE ( 'NONE', *, *, #58208, .F. ) ;
#126786 = CARTESIAN_POINT ( 'NONE',  ( 183.9218750003414016, 0.000000000000000000, 7.564683531250000925 ) ) ;
#126787 = DIRECTION ( 'NONE',  ( 0.000000000000000000, 0.000000000000000000, -1.000000000000000000 ) ) ;
#126788 = LINE ( 'NONE', #46279, #74030 ) ;
#126789 = CARTESIAN_POINT ( 'NONE',  ( 4.199999999999941558, 2.500000000000000000, -4.330127018922201643 ) ) ;
#126790 = CARTESIAN_POINT ( 'NONE',  ( 2.499999999999981792, 2.500000000000000000, 4.430127018922196847 ) ) ;
#126793 = AXIS2_PLACEMENT_3D ( 'NONE', #76316, #26571, #35745 ) ;
#126792 = CARTESIAN_POINT ( 'NONE',  ( -1.050000000000037792, 12.50000000000000000, 6.148780366869520009 ) ) ;
#126791 = AXIS2_PLACEMENT_3D ( 'NONE', #74652, #74018, #34097 ) ;
#126795 = EDGE_CURVE ( 'NONE', #103176, #31133, #62830, .T. ) ;
#126794 = FACE_OUTER_BOUND ( 'NONE', #56508, .T. ) ;
#126796 = DIRECTION ( 'NONE',  ( 0.000000000000000000, 1.000000000000000000, 0.000000000000000000 ) ) ;
#126797 = DIRECTION ( 'NONE',  ( -0.000000000000000000, -1.000000000000000000, -0.000000000000000000 ) ) ;
#126798 = DIRECTION ( 'NONE',  ( 0.000000000000000000, 1.000000000000000000, 0.000000000000000000 ) ) ;
#126800 = CONICAL_SURFACE ( 'NONE', #13910, 0.1000000000000002554, 0.003490658503988666988 ) ;
#126799 = AXIS2_PLACEMENT_3D ( 'NONE', #82541, #122466, #32804 ) ;
#126801 = CIRCLE ( 'NONE', #124657, 0.1000000000000002554 ) ;
#126802 = ORIENTED_EDGE ( 'NONE', *, *, #73218, .F. ) ;
#126803 = DIRECTION ( 'NONE',  ( 0.000000000000000000, 0.000000000000000000, 1.000000000000000000 ) ) ;
#126804 = ADVANCED_FACE ( 'NONE', ( #81809 ), #25667, .T. ) ;
#126805 = DIRECTION ( 'NONE',  ( 0.000000000000000000, 1.000000000000000000, 0.000000000000000000 ) ) ;
#126806 = CARTESIAN_POINT ( 'NONE',  ( 9.349999999999916156, 12.50000000000000000, 6.906693963081109722 ) ) ;
#126807 = DIRECTION ( 'NONE',  ( -0.000000000000000000, 1.000000000000000000, -0.000000000000000000 ) ) ;
#126808 = ORIENTED_EDGE ( 'NONE', *, *, #84249, .F. ) ;
#126809 = DIRECTION ( 'NONE',  ( -0.000000000000000000, 1.000000000000000000, -0.000000000000000000 ) ) ;
#126810 = CARTESIAN_POINT ( 'NONE',  ( 185.5000000000000000, 0.000000000000000000, 7.700000000000000178 ) ) ;
#126812 = EDGE_LOOP ( 'NONE', ( #91851, #11002 ) ) ;
#126811 = DIRECTION ( 'NONE',  ( 0.000000000000000000, -0.9999939076577903929, 0.003490651415223739937 ) ) ;
#126813 = AXIS2_PLACEMENT_3D ( 'NONE', #22115, #62023, #52195 ) ;
#126814 = ORIENTED_EDGE ( 'NONE', *, *, #91458, .F. ) ;
#126815 = AXIS2_PLACEMENT_3D ( 'NONE', #36269, #115426, #125904 ) ;
#126816 = CIRCLE ( 'NONE', #30696, 0.06509327318403745899 ) ;
#126817 = ORIENTED_EDGE ( 'NONE', *, *, #85616, .T. ) ;
#126818 = ORIENTED_EDGE ( 'NONE', *, *, #109843, .T. ) ;
#126819 = ORIENTED_EDGE ( 'NONE', *, *, #5073, .F. ) ;
#126820 = DIRECTION ( 'NONE',  ( 0.000000000000000000, -0.000000000000000000, 1.000000000000000000 ) ) ;
#126821 = VECTOR ( 'NONE', #75663, 1000.000000000000000 ) ;
#126822 = CARTESIAN_POINT ( 'NONE',  ( -17.50000000000000000, 1.500000000000000000, 1.734723475976807094E-15 ) ) ;
#126823 = CARTESIAN_POINT ( 'NONE',  ( 2.499999999999948930, 12.50000000000000000, -5.022947341949754119 ) ) ;
#126824 = CIRCLE ( 'NONE', #28631, 0.1000000000000002554 ) ;
#126825 = CARTESIAN_POINT ( 'NONE',  ( 0.7999999999999553024, 2.500000000000000000, -4.430127018922202176 ) ) ;
#126826 = VERTEX_POINT ( 'NONE', #43206 ) ;
#126827 = CIRCLE ( 'NONE', #93476, 0.09999999999999999167 ) ;
#126828 = ADVANCED_FACE ( 'NONE', ( #30812 ), #80054, .T. ) ;
#126829 = CARTESIAN_POINT ( 'NONE',  ( 10.39999999999990976, 2.500000000000000000, 4.230127018922196669 ) ) ;
#126830 = ORIENTED_EDGE ( 'NONE', *, *, #83718, .T. ) ;
#126831 = DIRECTION ( 'NONE',  ( -4.274815082592931898E-19, -0.9999939076577903929, -0.003490651415223739937 ) ) ;
#126832 = CARTESIAN_POINT ( 'NONE',  ( -6.050000000000022027, 2.500000000000000000, -6.148780366869526226 ) ) ;
#126833 = FACE_OUTER_BOUND ( 'NONE', #120818, .T. ) ;
#126834 = CARTESIAN_POINT ( 'NONE',  ( 10.84999999999991260, 12.50000000000000000, -1.472243186433550122 ) ) ;
#126835 = AXIS2_PLACEMENT_3D ( 'NONE', #53655, #43213, #20972 ) ;
#126836 = EDGE_CURVE ( 'NONE', #125502, #16131, #17232, .T. ) ;
#126837 = VERTEX_POINT ( 'NONE', #31445 ) ;
#126839 = AXIS2_PLACEMENT_3D ( 'NONE', #3890, #53006, #90987 ) ;
#126838 = AXIS2_PLACEMENT_3D ( 'NONE', #88085, #100509, #127404 ) ;
#126840 = ORIENTED_EDGE ( 'NONE', *, *, #12761, .F. ) ;
#126841 = ORIENTED_EDGE ( 'NONE', *, *, #79165, .T. ) ;
#126842 = ORIENTED_EDGE ( 'NONE', *, *, #18256, .F. ) ;
#126843 = CARTESIAN_POINT ( 'NONE',  ( 9.199999999999915801, 2.500000000000000000, 4.430127018922196847 ) ) ;
#126844 = CARTESIAN_POINT ( 'NONE',  ( 6.249999999999967137, 2.500000000000000000, 6.395190528383296602 ) ) ;
#126845 = EDGE_CURVE ( 'NONE', #119064, #104360, #22279, .T. ) ;
#126846 = EDGE_CURVE ( 'NONE', #80874, #91490, #100873, .T. ) ;
#126847 = LINE ( 'NONE', #86251, #115075 ) ;
#126848 = ADVANCED_FACE ( 'NONE', ( #33387 ), #11130, .T. ) ;
#126849 = FACE_BOUND ( 'NONE', #124282, .T. ) ;
#126850 = EDGE_CURVE ( 'NONE', #33917, #31361, #40362, .T. ) ;
#126851 = CARTESIAN_POINT ( 'NONE',  ( 12.49999999999990052, 12.50000000000000000, 0.6277270498435120194 ) ) ;
#126852 = DIRECTION ( 'NONE',  ( 0.000000000000000000, 1.000000000000000000, 0.000000000000000000 ) ) ;
#126853 = DIRECTION ( 'NONE',  ( 0.000000000000000000, 0.000000000000000000, -1.000000000000000000 ) ) ;
#126854 = CARTESIAN_POINT ( 'NONE',  ( -10.65000000000000391, 12.50000000000000000, -6.841600689897075149 ) ) ;
#126855 = EDGE_CURVE ( 'NONE', #61868, #1183, #42409, .T. ) ;
#126856 = ADVANCED_FACE ( 'NONE', ( #72015 ), #21617, .T. ) ;
#126857 = CARTESIAN_POINT ( 'NONE',  ( 184.0885416670080872, -6.551208109652273848, -3.782341765625003571 ) ) ;
#126858 = CARTESIAN_POINT ( 'NONE',  ( -8.350000000000008527, 2.500000000000000000, 5.802370205355744659 ) ) ;
#126860 = ADVANCED_FACE ( 'NONE', ( #121735 ), #2664, .T. ) ;
#126859 = AXIS2_PLACEMENT_3D ( 'NONE', #10950, #90830, #50921 ) ;
#126861 = CARTESIAN_POINT ( 'NONE',  ( -0.8500000000000395017, 12.50000000000000000, 6.495190528383297135 ) ) ;
#126862 = EDGE_CURVE ( 'NONE', #111547, #126431, #75831, .T. ) ;
#126863 = EDGE_CURVE ( 'NONE', #79758, #32478, #16906, .T. ) ;
#126864 = CARTESIAN_POINT ( 'NONE',  ( -11.05000000000000071, 2.500000000000000000, 6.841600689897072485 ) ) ;
#126865 = VERTEX_POINT ( 'NONE', #26130 ) ;
#126866 = ORIENTED_EDGE ( 'NONE', *, *, #80522, .F. ) ;
#126867 = ORIENTED_EDGE ( 'NONE', *, *, #49447, .F. ) ;
#126868 = ORIENTED_EDGE ( 'NONE', *, *, #122813, .F. ) ;
#126869 = DIRECTION ( 'NONE',  ( 0.000000000000000000, 1.000000000000000000, 0.000000000000000000 ) ) ;
#126870 = FACE_BOUND ( 'NONE', #36863, .T. ) ;
#126871 = ADVANCED_FACE ( 'NONE', ( #113865 ), #54292, .T. ) ;
#126872 = DIRECTION ( 'NONE',  ( -0.000000000000000000, 1.000000000000000000, -0.000000000000000000 ) ) ;
#126873 = DIRECTION ( 'NONE',  ( -0.000000000000000000, 1.000000000000000000, -0.000000000000000000 ) ) ;
#126874 = VECTOR ( 'NONE', #12901, 1000.000000000000000 ) ;
#126875 = AXIS2_PLACEMENT_3D ( 'NONE', #126655, #63383, #103311 ) ;
#126876 = EDGE_LOOP ( 'NONE', ( #70216, #102831 ) ) ;
#126877 = DIRECTION ( 'NONE',  ( 0.000000000000000000, 0.000000000000000000, 1.000000000000000000 ) ) ;
#126878 = FACE_OUTER_BOUND ( 'NONE', #9816, .T. ) ;
#126879 = ORIENTED_EDGE ( 'NONE', *, *, #126901, .T. ) ;
#126880 = DIRECTION ( 'NONE',  ( 1.000000000000000000, 0.000000000000000000, 0.000000000000000000 ) ) ;
#126881 = DIRECTION ( 'NONE',  ( -4.274815082592931898E-19, -0.9999939076577903929, -0.003490651415223739937 ) ) ;
#126883 = AXIS2_PLACEMENT_3D ( 'NONE', #33294, #112486, #1231 ) ;
#126882 = AXIS2_PLACEMENT_3D ( 'NONE', #36023, #75935, #115867 ) ;
#126884 = ORIENTED_EDGE ( 'NONE', *, *, #86370, .F. ) ;
#126885 = DIRECTION ( 'NONE',  ( 0.000000000000000000, 0.000000000000000000, -1.000000000000000000 ) ) ;
#126886 = DIRECTION ( 'NONE',  ( 0.000000000000000000, 0.000000000000000000, 1.000000000000000000 ) ) ;
#126888 = AXIS2_PLACEMENT_3D ( 'NONE', #115218, #104146, #14454 ) ;
#126887 = AXIS2_PLACEMENT_3D ( 'NONE', #60652, #122153, #50821 ) ;
#126889 = VERTEX_POINT ( 'NONE', #6441 ) ;
#126890 = AXIS2_PLACEMENT_3D ( 'NONE', #92583, #42199, #112227 ) ;
#126891 = DIRECTION ( 'NONE',  ( 0.000000000000000000, 0.000000000000000000, 1.000000000000000000 ) ) ;
#126892 = DIRECTION ( 'NONE',  ( 0.000000000000000000, 0.000000000000000000, -1.000000000000000000 ) ) ;
#126893 = ORIENTED_EDGE ( 'NONE', *, *, #121981, .T. ) ;
#126894 = FACE_OUTER_BOUND ( 'NONE', #84969, .T. ) ;
#126895 = VERTEX_POINT ( 'NONE', #64750 ) ;
#126896 = EDGE_LOOP ( 'NONE', ( #124492, #66880 ) ) ;
#126897 = DIRECTION ( 'NONE',  ( 0.000000000000000000, 0.000000000000000000, 1.000000000000000000 ) ) ;
#126898 = ORIENTED_EDGE ( 'NONE', *, *, #100947, .T. ) ;
#126899 = DIRECTION ( 'NONE',  ( -0.000000000000000000, -1.000000000000000000, -0.000000000000000000 ) ) ;
#126900 = DIRECTION ( 'NONE',  ( 0.000000000000000000, 0.000000000000000000, 1.000000000000000000 ) ) ;
#126901 = EDGE_CURVE ( 'NONE', #120397, #63967, #64108, .T. ) ;
#126902 = EDGE_LOOP ( 'NONE', ( #47372, #95911 ) ) ;
#126904 = EDGE_CURVE ( 'NONE', #2089, #129059, #23613, .T. ) ;
#126903 = DIRECTION ( 'NONE',  ( 0.000000000000000000, 0.000000000000000000, -1.000000000000000000 ) ) ;
#126905 = ORIENTED_EDGE ( 'NONE', *, *, #105334, .T. ) ;
#126906 = DIRECTION ( 'NONE',  ( -0.000000000000000000, -1.000000000000000000, -0.000000000000000000 ) ) ;
#126907 = CARTESIAN_POINT ( 'NONE',  ( 11.44999999999991047, 2.500000000000000000, -2.511473670974877948 ) ) ;
#126908 = DIRECTION ( 'NONE',  ( 0.000000000000000000, 0.000000000000000000, -1.000000000000000000 ) ) ;
#126909 = CARTESIAN_POINT ( 'NONE',  ( -6.850000000000017408, 2.500000000000000000, -6.148780366869526226 ) ) ;
#126911 = CIRCLE ( 'NONE', #91389, 0.06509327318403741736 ) ;
#126910 = CARTESIAN_POINT ( 'NONE',  ( 17.49101023696816881, 2.144674160806442575, -4.220798295113491250 ) ) ;
#126912 = CONICAL_SURFACE ( 'NONE', #7763, 0.1000000000000002554, 0.003490658503988666988 ) ;
#126913 = ADVANCED_FACE ( 'NONE', ( #5176 ), #29881, .T. ) ;
#126914 = ORIENTED_EDGE ( 'NONE', *, *, #34431, .F. ) ;
#126915 = VERTEX_POINT ( 'NONE', #126258 ) ;
#126916 = CARTESIAN_POINT ( 'NONE',  ( -0.6500000000000394351, 2.500000000000000000, 6.941600689897073018 ) ) ;
#126917 = AXIS2_PLACEMENT_3D ( 'NONE', #85297, #26401, #125235 ) ;
#126918 = CARTESIAN_POINT ( 'NONE',  ( -7.499999999999980460, 12.50000000000000000, -4.265033745738164406 ) ) ;
#126919 = LINE ( 'NONE', #16914, #24963 ) ;
#126921 = EDGE_LOOP ( 'NONE', ( #71223, #116146, #128643, #81197 ) ) ;
#126920 = VERTEX_POINT ( 'NONE', #36611 ) ;
#126922 = VERTEX_POINT ( 'NONE', #85679 ) ;
#126923 = CARTESIAN_POINT ( 'NONE',  ( -9.800000000000006040, 2.500000000000000000, -4.576537180435973795 ) ) ;
#126924 = CIRCLE ( 'NONE', #129093, 0.06509327318403745899 ) ;
#126925 = AXIS2_PLACEMENT_3D ( 'NONE', #43666, #124133, #12237 ) ;
#126926 = PLANE ( 'NONE',  #98767 ) ;
#126927 = CARTESIAN_POINT ( 'NONE',  ( 9.149999999999916866, 12.50000000000000000, 5.867463478539781896 ) ) ;
#126928 = AXIS2_PLACEMENT_3D ( 'NONE', #26846, #87689, #66757 ) ;
#126929 = APPLICATION_PROTOCOL_DEFINITION ( 'draft international standard', 'automotive_design', 1998, #60581 ) ;
#126930 = FACE_OUTER_BOUND ( 'NONE', #50272, .T. ) ;
#126931 = CARTESIAN_POINT ( 'NONE',  ( 187.0000000000000000, 0.000000000000000000, 7.700000000000000178 ) ) ;
#126932 = DIRECTION ( 'NONE',  ( -4.274815082592931898E-19, -0.9999939076577903929, -0.003490651415223739937 ) ) ;
#126933 = CARTESIAN_POINT ( 'NONE',  ( 12.69999999999990159, 12.50000000000000000, 4.676537180435972552 ) ) ;
#126934 = DIRECTION ( 'NONE',  ( -0.000000000000000000, -1.000000000000000000, -0.000000000000000000 ) ) ;
#126935 = CIRCLE ( 'NONE', #35010, 0.09999999999999999167 ) ;
#126936 = DIRECTION ( 'NONE',  ( 0.000000000000000000, 0.000000000000000000, 1.000000000000000000 ) ) ;
#126937 = ORIENTED_EDGE ( 'NONE', *, *, #39596, .F. ) ;
#126939 = CIRCLE ( 'NONE', #47518, 0.09999999999999999167 ) ;
#126938 = CONICAL_SURFACE ( 'NONE', #91417, 0.1000000000000002554, 0.003490658503988666988 ) ;
#126940 = PLANE ( 'NONE',  #48665 ) ;
#126941 = ORIENTED_EDGE ( 'NONE', *, *, #34862, .T. ) ;
#126942 = ORIENTED_EDGE ( 'NONE', *, *, #51958, .T. ) ;
#126943 = DIRECTION ( 'NONE',  ( 0.000000000000000000, 0.000000000000000000, -1.000000000000000000 ) ) ;
#126944 = DIRECTION ( 'NONE',  ( -0.000000000000000000, 1.000000000000000000, -0.000000000000000000 ) ) ;
#126945 = LINE ( 'NONE', #47103, #125951 ) ;
#126946 = DIRECTION ( 'NONE',  ( -0.000000000000000000, -1.000000000000000000, -0.000000000000000000 ) ) ;
#126947 = DIRECTION ( 'NONE',  ( 0.000000000000000000, 0.000000000000000000, 1.000000000000000000 ) ) ;
#126948 = FACE_OUTER_BOUND ( 'NONE', #125338, .T. ) ;
#126949 = CARTESIAN_POINT ( 'NONE',  ( 3.349999999999941913, 2.500000000000000000, 5.902370205355745192 ) ) ;
#126950 = ORIENTED_EDGE ( 'NONE', *, *, #121927, .T. ) ;
#126951 = DIRECTION ( 'NONE',  ( 0.000000000000000000, 0.000000000000000000, 1.000000000000000000 ) ) ;
#126952 = VECTOR ( 'NONE', #36589, 1000.000000000000000 ) ;
#126953 = DIRECTION ( 'NONE',  ( 0.000000000000000000, 1.000000000000000000, 0.000000000000000000 ) ) ;
#126954 = ORIENTED_EDGE ( 'NONE', *, *, #129080, .T. ) ;
#126955 = ORIENTED_EDGE ( 'NONE', *, *, #47381, .T. ) ;
#126956 = EDGE_CURVE ( 'NONE', #30920, #9494, #3897, .T. ) ;
#126957 = ORIENTED_EDGE ( 'NONE', *, *, #25363, .F. ) ;
#126959 = ORIENTED_EDGE ( 'NONE', *, *, #81010, .T. ) ;
#126958 = ADVANCED_FACE ( 'NONE', ( #96145 ), #46392, .T. ) ;
#126960 = CARTESIAN_POINT ( 'NONE',  ( -8.150000000000012790, 2.500000000000000000, 2.411473670974873862 ) ) ;
#126961 = DIRECTION ( 'NONE',  ( 0.000000000000000000, 0.000000000000000000, 1.000000000000000000 ) ) ;
#126962 = EDGE_LOOP ( 'NONE', ( #56459, #100495, #51469, #50528 ) ) ;
#126963 = CONICAL_SURFACE ( 'NONE', #1558, 0.09999999999999982514, 0.003490658503988666988 ) ;
#126964 = CARTESIAN_POINT ( 'NONE',  ( -0.4000000000000331624, 2.500000000000000000, -0.6928203230275519209 ) ) ;
#126966 = CARTESIAN_POINT ( 'NONE',  ( 2.899999999999944844, 2.500000000000000000, 3.637306695894644726 ) ) ;
#126965 = AXIS2_PLACEMENT_3D ( 'NONE', #113450, #43445, #4123 ) ;
#126967 = DIRECTION ( 'NONE',  ( 0.000000000000000000, 0.000000000000000000, 1.000000000000000000 ) ) ;
#126968 = EDGE_LOOP ( 'NONE', ( #56623, #76873, #119238, #106157 ) ) ;
#126969 = EDGE_CURVE ( 'NONE', #98359, #20666, #119752, .T. ) ;
#126970 = DIRECTION ( 'NONE',  ( 0.000000000000000000, 1.000000000000000000, 0.000000000000000000 ) ) ;
#126972 = AXIS2_PLACEMENT_3D ( 'NONE', #83668, #81098, #33916 ) ;
#126971 = VECTOR ( 'NONE', #85608, 1000.000000000000000 ) ;
#126973 = CARTESIAN_POINT ( 'NONE',  ( 3.549999999999942091, 12.50000000000000000, 2.511473670974873507 ) ) ;
#126974 = ORIENTED_EDGE ( 'NONE', *, *, #25323, .F. ) ;
#126975 = AXIS2_PLACEMENT_3D ( 'NONE', #9883, #77330, #97613 ) ;
#126976 = ORIENTED_EDGE ( 'NONE', *, *, #103206, .T. ) ;
#126977 = EDGE_LOOP ( 'NONE', ( #9199, #30705, #94059, #7428 ) ) ;
#126978 = FACE_OUTER_BOUND ( 'NONE', #109852, .T. ) ;
#126980 = CONICAL_SURFACE ( 'NONE', #70535, 0.1000000000000000472, 0.003490658503988666988 ) ;
#126979 = AXIS2_PLACEMENT_3D ( 'NONE', #95260, #63210, #14728 ) ;
#126981 = CARTESIAN_POINT ( 'NONE',  ( 2.099999999999947686, 12.50000000000000000, 5.022947341949748790 ) ) ;
#126982 = VECTOR ( 'NONE', #4653, 1000.000000000000000 ) ;
#126983 = EDGE_CURVE ( 'NONE', #127177, #65511, #10979, .T. ) ;
#126984 = ORIENTED_EDGE ( 'NONE', *, *, #66515, .T. ) ;
#126985 = DIRECTION ( 'NONE',  ( 0.000000000000000000, 0.000000000000000000, 1.000000000000000000 ) ) ;
#126986 = CARTESIAN_POINT ( 'NONE',  ( 1.899999999999951283, 2.500000000000000000, -3.883716857408426648 ) ) ;
#126987 = FACE_OUTER_BOUND ( 'NONE', #5201, .T. ) ;
#126988 = CARTESIAN_POINT ( 'NONE',  ( 7.699999999999922018, 12.50000000000000000, 0.3464101615137735735 ) ) ;
#126989 = EDGE_CURVE ( 'NONE', #124287, #7788, #123656, .T. ) ;
#126990 = ORIENTED_EDGE ( 'NONE', *, *, #81181, .F. ) ;
#126991 = CONICAL_SURFACE ( 'NONE', #87265, 0.09999999999999999167, 0.003490658503988666988 ) ;
#126992 = CARTESIAN_POINT ( 'NONE',  ( -8.750000000000010658, 12.50000000000000000, -7.122917578226811486 ) ) ;
#126993 = CONICAL_SURFACE ( 'NONE', #14105, 0.1000000000000000472, 0.003490658503988666988 ) ;
#126994 = EDGE_LOOP ( 'NONE', ( #95376, #52144 ) ) ;
#126995 = ORIENTED_EDGE ( 'NONE', *, *, #110564, .T. ) ;
#126996 = ADVANCED_FACE ( 'NONE', ( #4513 ), #21467, .T. ) ;
#126997 = VERTEX_POINT ( 'NONE', #24835 ) ;
#126998 = ADVANCED_FACE ( 'NONE', ( #94863 ), #54905, .T. ) ;
#126999 = FACE_OUTER_BOUND ( 'NONE', #80788, .T. ) ;
#127000 = EDGE_CURVE ( 'NONE', #97467, #104697, #71639, .T. ) ;
#127001 = FACE_BOUND ( 'NONE', #96141, .T. ) ;
#127002 = CIRCLE ( 'NONE', #87274, 0.06509327318403745899 ) ;
#127003 = EDGE_CURVE ( 'NONE', #48809, #89954, #84241, .T. ) ;
#127004 = DIRECTION ( 'NONE',  ( 0.000000000000000000, 1.000000000000000000, 0.000000000000000000 ) ) ;
#127005 = FACE_OUTER_BOUND ( 'NONE', #85659, .T. ) ;
#127006 = VECTOR ( 'NONE', #67904, 1000.000000000000000 ) ;
#127007 = PLANE ( 'NONE',  #85705 ) ;
#127008 = AXIS2_PLACEMENT_3D ( 'NONE', #82056, #1562, #70958 ) ;
#127009 = EDGE_CURVE ( 'NONE', #87918, #24428, #29980, .T. ) ;
#127010 = ORIENTED_EDGE ( 'NONE', *, *, #119044, .F. ) ;
#127011 = CARTESIAN_POINT ( 'NONE',  ( -7.050000000000013145, 2.500000000000000000, 2.265063509461097357 ) ) ;
#127012 = CARTESIAN_POINT ( 'NONE',  ( 7.099999999999928590, 12.50000000000000000, -5.022947341949754119 ) ) ;
#127013 = ADVANCED_FACE ( 'NONE', ( #115787 ), #27808, .T. ) ;
#127015 = CARTESIAN_POINT ( 'NONE',  ( 12.89999999999990088, 2.500000000000000000, -4.330127018922201643 ) ) ;
#127014 = AXIS2_PLACEMENT_3D ( 'NONE', #100962, #51250, #118025 ) ;
#127017 = DIRECTION ( 'NONE',  ( -0.000000000000000000, -1.000000000000000000, -0.000000000000000000 ) ) ;
#127016 = AXIS2_PLACEMENT_3D ( 'NONE', #90000, #120127, #107722 ) ;
#127018 = ORIENTED_EDGE ( 'NONE', *, *, #120394, .F. ) ;
#127019 = DIRECTION ( 'NONE',  ( -0.000000000000000000, 1.000000000000000000, -0.000000000000000000 ) ) ;
#127020 = ADVANCED_FACE ( 'NONE', ( #38550 ), #34088, .T. ) ;
#127021 = AXIS2_PLACEMENT_3D ( 'NONE', #43891, #54973, #123695 ) ;
#127022 = AXIS2_PLACEMENT_3D ( 'NONE', #5258, #35384, #55657 ) ;
#127023 = EDGE_CURVE ( 'NONE', #117617, #24882, #67298, .T. ) ;
#127024 = DIRECTION ( 'NONE',  ( -0.000000000000000000, 1.000000000000000000, -0.000000000000000000 ) ) ;
#127025 = VERTEX_POINT ( 'NONE', #17576 ) ;
#127026 = DIRECTION ( 'NONE',  ( -0.000000000000000000, -1.000000000000000000, -0.000000000000000000 ) ) ;
#127027 = CIRCLE ( 'NONE', #89449, 0.1000000000000000472 ) ;
#127028 = ADVANCED_FACE ( 'NONE', ( #128865 ), #61282, .T. ) ;
#127029 = CARTESIAN_POINT ( 'NONE',  ( -8.350000000000013856, 12.50000000000000000, -7.188010851410848723 ) ) ;
#127030 = FACE_BOUND ( 'NONE', #68042, .T. ) ;
#127031 = ADVANCED_FACE ( 'NONE', ( #57525 ), #11075, .T. ) ;
#127032 = DIRECTION ( 'NONE',  ( 0.000000000000000000, 0.000000000000000000, 1.000000000000000000 ) ) ;
#127034 = AXIS2_PLACEMENT_3D ( 'NONE', #97682, #55829, #66292 ) ;
#127033 = VECTOR ( 'NONE', #21820, 1000.000000000000000 ) ;
#127035 = EDGE_LOOP ( 'NONE', ( #64154, #83921, #73055, #85120 ) ) ;
#127036 = CARTESIAN_POINT ( 'NONE',  ( -5.850000000000018296, 2.500000000000000000, 1.572243186433545548 ) ) ;
#127037 = ORIENTED_EDGE ( 'NONE', *, *, #74662, .F. ) ;
#127038 =( BOUNDED_CURVE ( )  B_SPLINE_CURVE ( 2, ( #45392, #54534, #94464, #4788, #125231, #44748, #84661 ),
 .UNSPECIFIED., .F., .F. ) 
 B_SPLINE_CURVE_WITH_KNOTS ( ( 3, 2, 2, 3 ),
 ( 0.4285714285714289362, 0.4523809523809527722, 0.4761904761904766081, 0.5000000000000004441 ),
 .UNSPECIFIED. ) 
 CURVE ( )  GEOMETRIC_REPRESENTATION_ITEM ( )  RATIONAL_B_SPLINE_CURVE ( ( 0.9999999999999977796, 0.8660254037844409281, 1.000000000000000000, 0.8660254037844387076, 1.000000000000000000, 0.8660254037844361541, 1.000000000000002442 ) ) 
 REPRESENTATION_ITEM ( '' )  );
#127039 = VERTEX_POINT ( 'NONE', #7759 ) ;
#127040 = CARTESIAN_POINT ( 'NONE',  ( -5.400000000000023448, 2.500000000000000000, -5.022947341949754119 ) ) ;
#127041 = CARTESIAN_POINT ( 'NONE',  ( 186.1666666666666856, -6.668395609140176816, -3.850000000000003642 ) ) ;
#127042 = EDGE_LOOP ( 'NONE', ( #115641, #21487, #63976, #30578 ) ) ;
#127043 = LINE ( 'NONE', #20941, #36561 ) ;
#127044 = CARTESIAN_POINT ( 'NONE',  ( -8.550000000000013145, 12.50000000000000000, -6.776507416713036136 ) ) ;
#127045 = DIRECTION ( 'NONE',  ( -0.000000000000000000, -1.000000000000000000, -0.000000000000000000 ) ) ;
#127046 = CIRCLE ( 'NONE', #93589, 2.250000000000001776 ) ;
#127047 = ORIENTED_EDGE ( 'NONE', *, *, #106401, .F. ) ;
#127048 = FACE_OUTER_BOUND ( 'NONE', #73287, .T. ) ;
#127049 = CARTESIAN_POINT ( 'NONE',  ( -13.09999999999999254, 2.500000000000000000, -4.576537180435974683 ) ) ;
#127050 = CARTESIAN_POINT ( 'NONE',  ( -3.350000000000032507, 2.500000000000000000, -6.495190528383302464 ) ) ;
#127051 = CARTESIAN_POINT ( 'NONE',  ( 16.55712542098053319, 0.2763552092525495829, -6.093697598455521280 ) ) ;
#127052 = ORIENTED_EDGE ( 'NONE', *, *, #639, .T. ) ;
#127053 = DIRECTION ( 'NONE',  ( 0.000000000000000000, -0.000000000000000000, 1.000000000000000000 ) ) ;
#127054 = ORIENTED_EDGE ( 'NONE', *, *, #7565, .F. ) ;
#127055 = FACE_OUTER_BOUND ( 'NONE', #80481, .T. ) ;
#127056 = CARTESIAN_POINT ( 'NONE',  ( -12.09999999999999432, 2.500000000000000000, 5.022947341949748790 ) ) ;
#127057 = ORIENTED_EDGE ( 'NONE', *, *, #84900, .T. ) ;
#127058 = CARTESIAN_POINT ( 'NONE',  ( -7.700000000000014388, 12.50000000000000000, -4.676537180435977881 ) ) ;
#127059 = PLANE ( 'NONE',  #68241 ) ;
#127060 = ADVANCED_FACE ( 'NONE', ( #96776 ), #19494, .T. ) ;
#127061 = DIRECTION ( 'NONE',  ( 0.000000000000000000, 0.000000000000000000, 1.000000000000000000 ) ) ;
#127062 = AXIS2_PLACEMENT_3D ( 'NONE', #85906, #125837, #66282 ) ;
#127063 = DIRECTION ( 'NONE',  ( 0.000000000000000000, -0.000000000000000000, 1.000000000000000000 ) ) ;
#127064 = EDGE_LOOP ( 'NONE', ( #94224, #43696 ) ) ;
#127066 = EDGE_CURVE ( 'NONE', #124332, #28942, #109385, .T. ) ;
#127065 = DIRECTION ( 'NONE',  ( 0.000000000000000000, 1.000000000000000000, 0.000000000000000000 ) ) ;
#127067 = CARTESIAN_POINT ( 'NONE',  ( 5.399999999999936406, 12.50000000000000000, -3.637306695894650055 ) ) ;
#127068 = CARTESIAN_POINT ( 'NONE',  ( 184.9843750003414016, -8.734944146203032389, -1.604583208406767949E-15 ) ) ;
#127069 = CARTESIAN_POINT ( 'NONE',  ( -8.350000000000012079, 2.500000000000000000, 2.857883832488649301 ) ) ;
#127070 = DIRECTION ( 'NONE',  ( 0.000000000000000000, -0.9999939076577903929, 0.003490651415223739937 ) ) ;
#127071 = AXIS2_PLACEMENT_3D ( 'NONE', #127896, #78162, #28414 ) ;
#127072 = ORIENTED_EDGE ( 'NONE', *, *, #86154, .F. ) ;
#127073 = AXIS2_PLACEMENT_3D ( 'NONE', #696, #90358, #11807 ) ;
#127075 = ORIENTED_EDGE ( 'NONE', *, *, #111446, .T. ) ;
#127074 = CONICAL_SURFACE ( 'NONE', #123145, 0.1000000000000002554, 0.003490658503988666988 ) ;
#127076 = DIRECTION ( 'NONE',  ( -0.000000000000000000, 1.000000000000000000, -0.000000000000000000 ) ) ;
#127077 = EDGE_LOOP ( 'NONE', ( #76267, #88518, #129112, #14595 ) ) ;
#127078 = DIRECTION ( 'NONE',  ( 0.000000000000000000, 0.000000000000000000, 1.000000000000000000 ) ) ;
#127080 = ORIENTED_EDGE ( 'NONE', *, *, #79153, .F. ) ;
#127079 = EDGE_LOOP ( 'NONE', ( #90658, #32491, #65977, #86208 ) ) ;
#127081 = ORIENTED_EDGE ( 'NONE', *, *, #45469, .F. ) ;
#127082 = CARTESIAN_POINT ( 'NONE',  ( -0.8500000000000390576, 12.50000000000000000, -6.495190528383302464 ) ) ;
#127084 = DIRECTION ( 'NONE',  ( 0.000000000000000000, 1.000000000000000000, 0.000000000000000000 ) ) ;
#127083 = VECTOR ( 'NONE', #85177, 1000.000000000000000 ) ;
#127085 = DIRECTION ( 'NONE',  ( 0.000000000000000000, 0.000000000000000000, -1.000000000000000000 ) ) ;
#127086 =( LENGTH_UNIT ( ) NAMED_UNIT ( * ) SI_UNIT ( .MILLI., .METRE. ) );
#127087 = DIRECTION ( 'NONE',  ( -0.000000000000000000, -1.000000000000000000, -0.000000000000000000 ) ) ;
#127088 = LINE ( 'NONE', #37421, #96109 ) ;
#127089 = CARTESIAN_POINT ( 'NONE',  ( 149.5981739382431783, 2.500000000000000000, 1.703575533167231537 ) ) ;
#127090 = CIRCLE ( 'NONE', #104092, 0.09999999999999982514 ) ;
#127091 = VERTEX_POINT ( 'NONE', #9707 ) ;
#127092 = PLANE ( 'NONE',  #95751 ) ;
#127093 = VERTEX_POINT ( 'NONE', #87609 ) ;
#127094 = AXIS2_PLACEMENT_3D ( 'NONE', #12526, #82583, #122499 ) ;
#127095 = EDGE_LOOP ( 'NONE', ( #88157, #107369 ) ) ;
#127096 = EDGE_LOOP ( 'NONE', ( #8553, #81955, #83840, #41079 ) ) ;
#127097 = ORIENTED_EDGE ( 'NONE', *, *, #74116, .T. ) ;
#127098 = CONICAL_SURFACE ( 'NONE', #60203, 0.09999999999999982514, 0.003490658503988666988 ) ;
#127099 = DIRECTION ( 'NONE',  ( -0.000000000000000000, -1.000000000000000000, -0.000000000000000000 ) ) ;
#127100 = EDGE_LOOP ( 'NONE', ( #18003, #81535, #61690, #34424 ) ) ;
#127101 = EDGE_LOOP ( 'NONE', ( #73071, #42332 ) ) ;
#127102 = CONICAL_SURFACE ( 'NONE', #87360, 0.09999999999999982514, 0.003490658503988666988 ) ;
#127103 = CIRCLE ( 'NONE', #22555, 0.1000000000000002554 ) ;
#127104 = ADVANCED_FACE ( 'NONE', ( #58181 ), #77781, .T. ) ;
#127105 = DIRECTION ( 'NONE',  ( 0.000000000000000000, -0.000000000000000000, 1.000000000000000000 ) ) ;
#127107 = AXIS2_PLACEMENT_3D ( 'NONE', #21873, #120702, #2860 ) ;
#127106 = CARTESIAN_POINT ( 'NONE',  ( 2.499999999999981792, 2.500000000000000000, 4.330127018922196314 ) ) ;
#127108 = LINE ( 'NONE', #37440, #63170 ) ;
#127109 = DIRECTION ( 'NONE',  ( 0.000000000000000000, 0.000000000000000000, 1.000000000000000000 ) ) ;
#127110 = CARTESIAN_POINT ( 'NONE',  ( -10.45000000000000107, 12.50000000000000000, 6.430097255199259010 ) ) ;
#127111 = ORIENTED_EDGE ( 'NONE', *, *, #34273, .F. ) ;
#127112 = AXIS2_PLACEMENT_3D ( 'NONE', #23057, #33534, #74089 ) ;
#127114 = AXIS2_PLACEMENT_3D ( 'NONE', #65707, #123976, #75517 ) ;
#127113 = CARTESIAN_POINT ( 'NONE',  ( 2.299999999999946976, 2.500000000000000000, 4.776537180435972196 ) ) ;
#127115 = EDGE_LOOP ( 'NONE', ( #39105, #127536 ) ) ;
#127116 = AXIS2_PLACEMENT_3D ( 'NONE', #9781, #88993, #89639 ) ;
#127117 = CARTESIAN_POINT ( 'NONE',  ( 2.500000000000002220, 1.500000000000000444, -9.999999999999998224 ) ) ;
#127118 = EDGE_LOOP ( 'NONE', ( #35714, #111055 ) ) ;
#127119 = DIRECTION ( 'NONE',  ( 0.000000000000000000, 0.000000000000000000, -1.000000000000000000 ) ) ;
#127120 = EDGE_LOOP ( 'NONE', ( #32972, #30857, #57037, #38736 ) ) ;
#127121 = ADVANCED_FACE ( 'NONE', ( #7109 ), #9022, .T. ) ;
#127122 = AXIS2_PLACEMENT_3D ( 'NONE', #46359, #128160, #56810 ) ;
#127123 = EDGE_CURVE ( 'NONE', #47068, #77555, #618, .T. ) ;
#127124 = EDGE_LOOP ( 'NONE', ( #124535, #96011, #21385, #52093 ) ) ;
#127125 = CARTESIAN_POINT ( 'NONE',  ( -1.900000000000034994, 2.500000000000000000, -0.3464101615137783474 ) ) ;
#127126 = CARTESIAN_POINT ( 'NONE',  ( 6.899999999999926636, 12.50000000000000000, 0.4115034346978110880 ) ) ;
#127128 = CONICAL_SURFACE ( 'NONE', #1710, 0.1000000000000002554, 0.003490658503988666988 ) ;
#127127 = CIRCLE ( 'NONE', #66552, 0.1000000000000002554 ) ;
#127129 = PLANE ( 'NONE',  #94761 ) ;
#127130 = CARTESIAN_POINT ( 'NONE',  ( 3.349999999999943689, 2.500000000000000000, 2.165063509461097713 ) ) ;
#127131 = CARTESIAN_POINT ( 'NONE',  ( -13.14999999999999147, 2.500000000000000000, -2.511473670974875727 ) ) ;
#127132 = ORIENTED_EDGE ( 'NONE', *, *, #92188, .T. ) ;
#127133 = DIRECTION ( 'NONE',  ( 0.000000000000000000, 0.000000000000000000, -1.000000000000000000 ) ) ;
#127134 = CARTESIAN_POINT ( 'NONE',  ( -1.050000000000038236, 2.500000000000000000, -6.148780366869526226 ) ) ;
#127135 = ADVANCED_FACE ( 'NONE', ( #48340 ), #18870, .T. ) ;
#127136 = CARTESIAN_POINT ( 'NONE',  ( 9.399999999999918643, 2.500000000000000000, 0.3464101615137736845 ) ) ;
#127137 = DIRECTION ( 'NONE',  ( 0.000000000000000000, -0.000000000000000000, 1.000000000000000000 ) ) ;
#127138 = CARTESIAN_POINT ( 'NONE',  ( -1.850000000000033840, 2.500000000000000000, 6.841600689897072485 ) ) ;
#127139 = EDGE_LOOP ( 'NONE', ( #42789, #118299 ) ) ;
#127140 = ORIENTED_EDGE ( 'NONE', *, *, #88885, .F. ) ;
#127141 = LINE ( 'NONE', #59038, #113535 ) ;
#127142 = ORIENTED_EDGE ( 'NONE', *, *, #83995, .F. ) ;
#127143 = DIRECTION ( 'NONE',  ( -0.000000000000000000, -1.000000000000000000, -0.000000000000000000 ) ) ;
#127144 = CARTESIAN_POINT ( 'NONE',  ( 3.949999999999941558, 12.50000000000000000, -6.148780366869526226 ) ) ;
#127145 = AXIS2_PLACEMENT_3D ( 'NONE', #3263, #85677, #83753 ) ;
#127146 = VECTOR ( 'NONE', #48352, 1000.000000000000000 ) ;
#127148 = ORIENTED_EDGE ( 'NONE', *, *, #48554, .F. ) ;
#127147 = CIRCLE ( 'NONE', #70698, 0.1000000000000002554 ) ;
#127149 = CARTESIAN_POINT ( 'NONE',  ( 184.9166666666666856, 6.668395609140176816, 3.850000000000000977 ) ) ;
#127150 = CARTESIAN_POINT ( 'NONE',  ( 7.049999999999928768, 2.500000000000000000, -2.165063509461101710 ) ) ;
#127151 = DIRECTION ( 'NONE',  ( -0.000000000000000000, 1.000000000000000000, -0.000000000000000000 ) ) ;
#127152 = FACE_OUTER_BOUND ( 'NONE', #62521, .T. ) ;
#127153 = ORIENTED_EDGE ( 'NONE', *, *, #14231, .F. ) ;
#127154 = VECTOR ( 'NONE', #21642, 1000.000000000000000 ) ;
#127155 = EDGE_CURVE ( 'NONE', #35157, #37472, #4811, .T. ) ;
#127156 = AXIS2_PLACEMENT_3D ( 'NONE', #103264, #22145, #62060 ) ;
#127157 = CARTESIAN_POINT ( 'NONE',  ( -5.650000000000023448, 12.50000000000000000, -2.511473670974877948 ) ) ;
#127158 = DIRECTION ( 'NONE',  ( 0.000000000000000000, 0.000000000000000000, 1.000000000000000000 ) ) ;
#127159 = VERTEX_POINT ( 'NONE', #28061 ) ;
#127160 = EDGE_CURVE ( 'NONE', #88991, #29584, #86389, .T. ) ;
#127161 = DIRECTION ( 'NONE',  ( -0.000000000000000000, 1.000000000000000000, -0.000000000000000000 ) ) ;
#127162 = DIRECTION ( 'NONE',  ( -4.274815082592931898E-19, -0.9999939076577903929, -0.003490651415223739937 ) ) ;
#127164 = EDGE_CURVE ( 'NONE', #61588, #2220, #111428, .T. ) ;
#127163 = CIRCLE ( 'NONE', #91642, 0.06509327318403745899 ) ;
#127165 = CARTESIAN_POINT ( 'NONE',  ( -5.800000000000022027, 2.500000000000000000, -4.330127018922201643 ) ) ;
#127166 = CIRCLE ( 'NONE', #60283, 0.06509327318403741736 ) ;
#127167 = ORIENTED_EDGE ( 'NONE', *, *, #109250, .T. ) ;
#127168 = CARTESIAN_POINT ( 'NONE',  ( 11.24999999999994316, 12.50000000000000000, -6.495190528383302464 ) ) ;
#127169 = ADVANCED_FACE ( 'NONE', ( #89552 ), #79106, .T. ) ;
#127170 = ADVANCED_FACE ( 'NONE', ( #109175 ), #69671, .T. ) ;
#127171 = VERTEX_POINT ( 'NONE', #90172 ) ;
#127172 = DIRECTION ( 'NONE',  ( -0.000000000000000000, 1.000000000000000000, -0.000000000000000000 ) ) ;
#127173 = CARTESIAN_POINT ( 'NONE',  ( 9.149999999999915090, 12.50000000000000000, -2.165063509461101710 ) ) ;
#127174 = ADVANCED_FACE ( 'NONE', ( #20169 ), #128175, .T. ) ;
#127175 = ADVANCED_FACE ( 'NONE', ( #80392 ), #98923, .T. ) ;
#127176 = CARTESIAN_POINT ( 'NONE',  ( 6.249999999999928946, 2.500000000000000000, 2.757883832488649656 ) ) ;
#127177 = VERTEX_POINT ( 'NONE', #60743 ) ;
#127178 = AXIS2_PLACEMENT_3D ( 'NONE', #54912, #13039, #25437 ) ;
#127179 = DIRECTION ( 'NONE',  ( 0.000000000000000000, 0.000000000000000000, 1.000000000000000000 ) ) ;
#127180 = ADVANCED_FACE ( 'NONE', ( #2442 ), #60117, .T. ) ;
#127181 = PLANE ( 'NONE',  #101785 ) ;
#127182 = AXIS2_PLACEMENT_3D ( 'NONE', #124551, #25050, #3475 ) ;
#127183 = VERTEX_POINT ( 'NONE', #52213 ) ;
#127184 = CARTESIAN_POINT ( 'NONE',  ( 12.09999999999990195, 12.50000000000000000, -2.276824562219559311E-15 ) ) ;
#127185 = ORIENTED_EDGE ( 'NONE', *, *, #15711, .T. ) ;
#127186 = EDGE_CURVE ( 'NONE', #104669, #43749, #103128, .T. ) ;
#127187 = LINE ( 'NONE', #6714, #74514 ) ;
#127188 = AXIS2_PLACEMENT_3D ( 'NONE', #119688, #90221, #92833 ) ;
#127189 = ORIENTED_EDGE ( 'NONE', *, *, #61515, .F. ) ;
#127190 = CARTESIAN_POINT ( 'NONE',  ( -3.100000000000028511, 12.50000000000000000, -3.918623584224389056 ) ) ;
#127191 = FACE_OUTER_BOUND ( 'NONE', #105684, .T. ) ;
#127192 = ORIENTED_EDGE ( 'NONE', *, *, #58992, .F. ) ;
#127193 = ORIENTED_EDGE ( 'NONE', *, *, #9778, .T. ) ;
#127194 = CARTESIAN_POINT ( 'NONE',  ( 5.649999999999936406, 2.500000000000000000, -6.741600689897077281 ) ) ;
#127195 = DIRECTION ( 'NONE',  ( 0.000000000000000000, 1.000000000000000000, 0.000000000000000000 ) ) ;
#127196 = VERTEX_POINT ( 'NONE', #92786 ) ;
#127197 = DIRECTION ( 'NONE',  ( -4.274815082592931898E-19, -0.9999939076577903929, -0.003490651415223739937 ) ) ;
#127198 = CARTESIAN_POINT ( 'NONE',  ( -2.100000000000033840, 12.50000000000000000, 3.637306695894644726 ) ) ;
#127199 = VECTOR ( 'NONE', #34761, 1000.000000000000000 ) ;
#127200 = CARTESIAN_POINT ( 'NONE',  ( 5.649999999999936406, 12.50000000000000000, -6.841600689897077814 ) ) ;
#127201 = DIRECTION ( 'NONE',  ( -0.000000000000000000, 1.000000000000000000, -0.000000000000000000 ) ) ;
#127202 = CARTESIAN_POINT ( 'NONE',  ( -5.800000000000018474, 12.50000000000000000, 4.265033745738159077 ) ) ;
#127203 = CARTESIAN_POINT ( 'NONE',  ( -3.550000000000027356, 12.50000000000000000, 1.818653347947321475 ) ) ;
#127204 = ORIENTED_EDGE ( 'NONE', *, *, #112665, .F. ) ;
#127205 = ORIENTED_EDGE ( 'NONE', *, *, #54700, .F. ) ;
#127206 = VERTEX_POINT ( 'NONE', #82323 ) ;
#127207 = ORIENTED_EDGE ( 'NONE', *, *, #17796, .T. ) ;
#127208 = PLANE ( 'NONE',  #45419 ) ;
#127209 = CARTESIAN_POINT ( 'NONE',  ( 4.149999999999939959, 2.500000000000000000, -2.065063509461102065 ) ) ;
#127210 = CARTESIAN_POINT ( 'NONE',  ( -10.60000000000000142, 2.500000000000000000, 3.883716857408421319 ) ) ;
#127211 = VECTOR ( 'NONE', #31257, 1000.000000000000000 ) ;
#127212 = EDGE_LOOP ( 'NONE', ( #51492, #120156 ) ) ;
#127213 = FACE_BOUND ( 'NONE', #77444, .T. ) ;
#127214 = FACE_OUTER_BOUND ( 'NONE', #81408, .T. ) ;
#127215 = CARTESIAN_POINT ( 'NONE',  ( 3.349999999999943689, 2.500000000000000000, 1.372243186433545370 ) ) ;
#127216 = DIRECTION ( 'NONE',  ( 0.000000000000000000, -0.000000000000000000, 1.000000000000000000 ) ) ;
#127218 = CONICAL_SURFACE ( 'NONE', #39500, 0.09999999999999982514, 0.003490658503988666988 ) ;
#127217 = CONICAL_SURFACE ( 'NONE', #14314, 0.1000000000000002554, 0.003490658503988666988 ) ;
#127219 = ADVANCED_FACE ( 'NONE', ( #511 ), #61393, .T. ) ;
#127220 = DIRECTION ( 'NONE',  ( 0.000000000000000000, -0.9999939076577903929, 0.003490651415223739937 ) ) ;
#127221 = DIRECTION ( 'NONE',  ( 0.000000000000000000, 0.000000000000000000, -1.000000000000000000 ) ) ;
#127222 = LINE ( 'NONE', #87902, #81049 ) ;
#127223 = DIRECTION ( 'NONE',  ( 0.000000000000000000, -0.9999939076577903929, 0.003490651415223739937 ) ) ;
#127224 = DIRECTION ( 'NONE',  ( 0.000000000000000000, 0.000000000000000000, 1.000000000000000000 ) ) ;
#127225 = CARTESIAN_POINT ( 'NONE',  ( -5.200000000000020606, 2.500000000000000000, 3.883716857408421319 ) ) ;
#127226 = DIRECTION ( 'NONE',  ( 0.000000000000000000, 0.000000000000000000, 1.000000000000000000 ) ) ;
#127227 = ADVANCED_FACE ( 'NONE', ( #22770 ), #62686, .T. ) ;
#127228 = ORIENTED_EDGE ( 'NONE', *, *, #78571, .T. ) ;
#127229 = ORIENTED_EDGE ( 'NONE', *, *, #6445, .T. ) ;
#127230 = ORIENTED_EDGE ( 'NONE', *, *, #39169, .T. ) ;
#127231 = ORIENTED_EDGE ( 'NONE', *, *, #70563, .T. ) ;
#127232 = DIRECTION ( 'NONE',  ( 0.000000000000000000, 0.000000000000000000, 1.000000000000000000 ) ) ;
#127233 = AXIS2_PLACEMENT_3D ( 'NONE', #52328, #105299, #92917 ) ;
#127234 = DIRECTION ( 'NONE',  ( -0.000000000000000000, 1.000000000000000000, -0.000000000000000000 ) ) ;
#127236 = EDGE_LOOP ( 'NONE', ( #24999, #106929 ) ) ;
#127235 = ORIENTED_EDGE ( 'NONE', *, *, #79401, .T. ) ;
#127237 = ORIENTED_EDGE ( 'NONE', *, *, #116091, .T. ) ;
#127238 = DIRECTION ( 'NONE',  ( 0.000000000000000000, -0.9999939076577903929, 0.003490651415223739937 ) ) ;
#127239 = AXIS2_PLACEMENT_3D ( 'NONE', #70286, #89274, #79467 ) ;
#127240 = DIRECTION ( 'NONE',  ( -0.000000000000000000, -1.000000000000000000, -0.000000000000000000 ) ) ;
#127242 = CARTESIAN_POINT ( 'NONE',  ( 9.599999999999914380, 2.500000000000000000, -4.922947341949753586 ) ) ;
#127241 = AXIS2_PLACEMENT_3D ( 'NONE', #109862, #108565, #18884 ) ;
#127243 = DIRECTION ( 'NONE',  ( 1.000000000000000000, -0.000000000000000000, -0.000000000000000000 ) ) ;
#127244 = CARTESIAN_POINT ( 'NONE',  ( 187.0312500006828031, 9.429780353434619030E-16, -7.700000000000000178 ) ) ;
#127245 = CARTESIAN_POINT ( 'NONE',  ( 11.04999999999991189, 12.50000000000000000, 6.213873640053559022 ) ) ;
#127246 = EDGE_LOOP ( 'NONE', ( #22324, #11274 ) ) ;
#127247 = DIRECTION ( 'NONE',  ( -0.000000000000000000, 1.000000000000000000, -0.000000000000000000 ) ) ;
#127248 = ORIENTED_EDGE ( 'NONE', *, *, #81897, .T. ) ;
#127249 = CIRCLE ( 'NONE', #129417, 0.06509327318403745899 ) ;
#127250 = VERTEX_POINT ( 'NONE', #122250 ) ;
#127251 = ORIENTED_EDGE ( 'NONE', *, *, #78306, .F. ) ;
#127252 = CIRCLE ( 'NONE', #87508, 0.06509327318403745899 ) ;
#127253 = CARTESIAN_POINT ( 'NONE',  ( 9.149999999999916866, 2.500000000000000000, 5.802370205355744659 ) ) ;
#127254 = ORIENTED_EDGE ( 'NONE', *, *, #20860, .T. ) ;
#127255 = ORIENTED_EDGE ( 'NONE', *, *, #87568, .T. ) ;
#127256 = CIRCLE ( 'NONE', #31205, 0.06509327318403745899 ) ;
#127257 = CARTESIAN_POINT ( 'NONE',  ( 1.049999999999953637, 2.500000000000000000, -1.818653347947326138 ) ) ;
#127259 = ADVANCED_FACE ( 'NONE', ( #62040 ), #32598, .T. ) ;
#127258 = AXIS2_PLACEMENT_3D ( 'NONE', #87024, #26826, #106029 ) ;
#127260 = CARTESIAN_POINT ( 'NONE',  ( 11.84999999999990727, 2.500000000000000000, -1.818653347947326138 ) ) ;
#127261 = FACE_OUTER_BOUND ( 'NONE', #47916, .T. ) ;
#127262 = DIRECTION ( 'NONE',  ( -1.224646799147352221E-16, 0.000000000000000000, -1.000000000000000000 ) ) ;
#127263 = DIRECTION ( 'NONE',  ( 0.000000000000000000, 0.000000000000000000, 1.000000000000000000 ) ) ;
#127264 = EDGE_LOOP ( 'NONE', ( #24201, #57644, #125348, #76677 ) ) ;
#127265 = DIRECTION ( 'NONE',  ( -0.000000000000000000, 1.000000000000000000, -0.000000000000000000 ) ) ;
#127267 = EDGE_CURVE ( 'NONE', #16136, #60318, #88446, .T. ) ;
#127266 = AXIS2_PLACEMENT_3D ( 'NONE', #118996, #79719, #70538 ) ;
#127268 = ORIENTED_EDGE ( 'NONE', *, *, #3678, .F. ) ;
#127269 = CARTESIAN_POINT ( 'NONE',  ( 2.899999999999944844, 2.500000000000000000, 5.122947341949749323 ) ) ;
#127270 = ORIENTED_EDGE ( 'NONE', *, *, #106648, .F. ) ;
#127271 = CARTESIAN_POINT ( 'NONE',  ( 0.7999999999999612976, 2.500000000000000000, -0.1000000000000001166 ) ) ;
#127272 = CARTESIAN_POINT ( 'NONE',  ( -9.600000000000006750, 12.50000000000000000, 3.702399969078682407 ) ) ;
#127273 = CIRCLE ( 'NONE', #70815, 0.09999999999999982514 ) ;
#127274 = ORIENTED_EDGE ( 'NONE', *, *, #89462, .F. ) ;
#127276 = EDGE_CURVE ( 'NONE', #36888, #95931, #102584, .T. ) ;
#127275 = FACE_OUTER_BOUND ( 'NONE', #48632, .T. ) ;
#127277 = LINE ( 'NONE', #47425, #89571 ) ;
#127278 = EDGE_CURVE ( 'NONE', #2822, #91444, #90502, .T. ) ;
#127279 = ORIENTED_EDGE ( 'NONE', *, *, #101142, .T. ) ;
#127280 = EDGE_CURVE ( 'NONE', #20773, #101675, #107232, .T. ) ;
#127281 = CARTESIAN_POINT ( 'NONE',  ( -3.749999999999994671, 2.500000000000000000, -6.495190528383302464 ) ) ;
#127282 = ORIENTED_EDGE ( 'NONE', *, *, #21784, .F. ) ;
#127283 = ORIENTED_EDGE ( 'NONE', *, *, #47388, .T. ) ;
#127284 = CARTESIAN_POINT ( 'NONE',  ( 5.649999999999932854, 12.50000000000000000, 1.818653347947321475 ) ) ;
#127285 = DIRECTION ( 'NONE',  ( 0.000000000000000000, -0.000000000000000000, 1.000000000000000000 ) ) ;
#127286 = ADVANCED_FACE ( 'NONE', ( #33235 ), #115632, .T. ) ;
#127287 = CARTESIAN_POINT ( 'NONE',  ( 185.9635416670080872, -4.367472073101519747, 7.564683531249999149 ) ) ;
#127288 = DIRECTION ( 'NONE',  ( -0.000000000000000000, 1.000000000000000000, -0.000000000000000000 ) ) ;
#127289 = CIRCLE ( 'NONE', #18609, 0.1000000000000002554 ) ;
#127290 = DIRECTION ( 'NONE',  ( 0.000000000000000000, 0.000000000000000000, 1.000000000000000000 ) ) ;
#127291 = CARTESIAN_POINT ( 'NONE',  ( 10.64999999999990976, 12.50000000000000000, 1.818653347947321475 ) ) ;
#127292 = CIRCLE ( 'NONE', #121020, 8.699999999999999289 ) ;
#127293 = ORIENTED_EDGE ( 'NONE', *, *, #5632, .T. ) ;
#127294 = CARTESIAN_POINT ( 'NONE',  ( 8.749999999999957367, 12.50000000000000000, 2.165063509461097713 ) ) ;
#127295 = CARTESIAN_POINT ( 'NONE',  ( 5.649999999999934630, 2.500000000000000000, 6.741600689897071952 ) ) ;
#127296 = ORIENTED_EDGE ( 'NONE', *, *, #50853, .F. ) ;
#127298 = VECTOR ( 'NONE', #14297, 1000.000000000000000 ) ;
#127297 = AXIS2_PLACEMENT_3D ( 'NONE', #112641, #13775, #2656 ) ;
#127299 = CIRCLE ( 'NONE', #14403, 0.06509327318403745899 ) ;
#127300 = PLANE ( 'NONE',  #24285 ) ;
#127301 = CARTESIAN_POINT ( 'NONE',  ( 129.5000000000000000, -1.500000000000000000, -2.598076211353316900 ) ) ;
#127302 = CARTESIAN_POINT ( 'NONE',  ( 1.449999999999949551, 12.50000000000000000, 6.906693963081109722 ) ) ;
#127303 = CARTESIAN_POINT ( 'NONE',  ( 0.5999999999999547917, 2.500000000000000000, 3.983716857408420076 ) ) ;
#127304 = CARTESIAN_POINT ( 'NONE',  ( -9.400000000000007461, 2.500000000000000000, 0.4464101615137735513 ) ) ;
#127305 = ORIENTED_EDGE ( 'NONE', *, *, #4766, .T. ) ;
#127306 = CIRCLE ( 'NONE', #66737, 0.06509327318403745899 ) ;
#127307 = CARTESIAN_POINT ( 'NONE',  ( -3.750000000000027534, 2.500000000000000000, -1.472243186433550122 ) ) ;
#127308 = FILL_AREA_STYLE_COLOUR ( '', #58060 ) ;
#127309 = ORIENTED_EDGE ( 'NONE', *, *, #4615, .F. ) ;
#127310 = EDGE_CURVE ( 'NONE', #73222, #99644, #80147, .T. ) ;
#127311 = FACE_OUTER_BOUND ( 'NONE', #71811, .T. ) ;
#127312 = VERTEX_POINT ( 'NONE', #71196 ) ;
#127313 = EDGE_LOOP ( 'NONE', ( #45710, #29462, #1970, #123839 ) ) ;
#127314 = DIRECTION ( 'NONE',  ( 0.000000000000000000, 0.000000000000000000, 1.000000000000000000 ) ) ;
#127315 = ADVANCED_FACE ( 'NONE', ( #111098 ), #36347, .T. ) ;
#127316 = CIRCLE ( 'NONE', #24903, 0.1000000000000000472 ) ;
#127317 = EDGE_CURVE ( 'NONE', #84067, #83209, #91483, .T. ) ;
#127318 = ORIENTED_EDGE ( 'NONE', *, *, #49921, .F. ) ;
#127319 = DIRECTION ( 'NONE',  ( -4.274815082592931898E-19, -0.9999939076577903929, -0.003490651415223739937 ) ) ;
#127321 = ADVANCED_FACE ( 'NONE', ( #65885 ), #103888, .T. ) ;
#127320 = FACE_OUTER_BOUND ( 'NONE', #15728, .T. ) ;
#127322 = EDGE_CURVE ( 'NONE', #12969, #59349, #95362, .T. ) ;
#127323 = DIRECTION ( 'NONE',  ( 0.000000000000000000, 0.000000000000000000, 1.000000000000000000 ) ) ;
#127324 = EDGE_LOOP ( 'NONE', ( #116920, #101533 ) ) ;
#127325 = VECTOR ( 'NONE', #69315, 1000.000000000000000 ) ;
#127326 = FACE_BOUND ( 'NONE', #129441, .T. ) ;
#127327 = CONICAL_SURFACE ( 'NONE', #87590, 0.1000000000000002554, 0.003490658503988666988 ) ;
#127328 = EDGE_CURVE ( 'NONE', #2568, #28423, #96951, .T. ) ;
#127330 = ORIENTED_EDGE ( 'NONE', *, *, #17763, .T. ) ;
#127329 = DIRECTION ( 'NONE',  ( 0.000000000000000000, 0.000000000000000000, -1.000000000000000000 ) ) ;
#127331 = CARTESIAN_POINT ( 'NONE',  ( 11.64999999999990443, 12.50000000000000000, -5.867463478539787225 ) ) ;
#127332 = CARTESIAN_POINT ( 'NONE',  ( -3.100000000000028511, 2.500000000000000000, -4.676537180435977881 ) ) ;
#127333 = CIRCLE ( 'NONE', #72951, 0.06509327318403745899 ) ;
#127334 = EDGE_LOOP ( 'NONE', ( #10923, #57065, #88711, #100480 ) ) ;
#127336 = ADVANCED_FACE ( 'NONE', ( #23376 ), #128278, .T. ) ;
#127335 = AXIS2_PLACEMENT_3D ( 'NONE', #6465, #86341, #108574 ) ;
#127337 = AXIS2_PLACEMENT_3D ( 'NONE', #3276, #34024, #22293 ) ;
#127338 = EDGE_CURVE ( 'NONE', #46960, #96127, #75698, .T. ) ;
#127339 = ORIENTED_EDGE ( 'NONE', *, *, #23218, .F. ) ;
#127340 = ORIENTED_EDGE ( 'NONE', *, *, #26339, .T. ) ;
#127341 = CARTESIAN_POINT ( 'NONE',  ( -2.700000000000030820, 2.500000000000000000, -3.983716857408426293 ) ) ;
#127342 = CARTESIAN_POINT ( 'NONE',  ( -12.49999999999995914, 2.500000000000000000, -4.330127018922198978 ) ) ;
#127343 = DIRECTION ( 'NONE',  ( 0.000000000000000000, 0.000000000000000000, -1.000000000000000000 ) ) ;
#127344 = FACE_BOUND ( 'NONE', #1781, .T. ) ;
#127345 = ORIENTED_EDGE ( 'NONE', *, *, #104113, .F. ) ;
#127346 = CARTESIAN_POINT ( 'NONE',  ( -11.44999999999999751, 2.500000000000000000, 1.818653347947321475 ) ) ;
#127347 = CARTESIAN_POINT ( 'NONE',  ( 3.149999999999944400, 12.50000000000000000, 1.883746621131358934 ) ) ;
#127348 = ORIENTED_EDGE ( 'NONE', *, *, #49749, .T. ) ;
#127349 = AXIS2_PLACEMENT_3D ( 'NONE', #60796, #124874, #25357 ) ;
#127350 = DIRECTION ( 'NONE',  ( 0.000000000000000000, 0.000000000000000000, 1.000000000000000000 ) ) ;
#127351 = LINE ( 'NONE', #27195, #71671 ) ;
#127352 = CARTESIAN_POINT ( 'NONE',  ( -2.100000000000033396, 12.50000000000000000, -3.637306695894650055 ) ) ;
#127353 = DIRECTION ( 'NONE',  ( -0.000000000000000000, -1.000000000000000000, -0.000000000000000000 ) ) ;
#127354 = ADVANCED_FACE ( 'NONE', ( #14196 ), #69770, .T. ) ;
#127355 = PLANE ( 'NONE',  #44017 ) ;
#127356 = ORIENTED_EDGE ( 'NONE', *, *, #115744, .T. ) ;
#127357 = ORIENTED_EDGE ( 'NONE', *, *, #30283, .F. ) ;
#127358 = ORIENTED_EDGE ( 'NONE', *, *, #89105, .T. ) ;
#127359 = ORIENTED_EDGE ( 'NONE', *, *, #23083, .F. ) ;
#127360 = ORIENTED_EDGE ( 'NONE', *, *, #21073, .T. ) ;
#127361 = AXIS2_PLACEMENT_3D ( 'NONE', #115445, #47382, #65059 ) ;
#127362 = CARTESIAN_POINT ( 'NONE',  ( 11.44999999999990692, 2.500000000000000000, 1.818653347947321475 ) ) ;
#127363 = DIRECTION ( 'NONE',  ( -4.274815082592931898E-19, -0.9999939076577903929, -0.003490651415223739937 ) ) ;
#127364 = ORIENTED_EDGE ( 'NONE', *, *, #61971, .F. ) ;
#127365 = FACE_BOUND ( 'NONE', #58083, .T. ) ;
#127366 = CARTESIAN_POINT ( 'NONE',  ( 6.249999999999930722, 2.500000000000000000, -1.372243186433550033 ) ) ;
#127367 = DIRECTION ( 'NONE',  ( 0.000000000000000000, 0.000000000000000000, 1.000000000000000000 ) ) ;
#127368 = CARTESIAN_POINT ( 'NONE',  ( 184.5000000000000000, -5.524290953051901099, 5.236943753751942765 ) ) ;
#127369 = DIRECTION ( 'NONE',  ( 0.000000000000000000, 1.000000000000000000, 0.000000000000000000 ) ) ;
#127370 = FACE_OUTER_BOUND ( 'NONE', #29767, .T. ) ;
#127371 = VERTEX_POINT ( 'NONE', #25978 ) ;
#127372 = CONICAL_SURFACE ( 'NONE', #75132, 0.1000000000000000056, 0.003490658503988666988 ) ;
#127373 = CARTESIAN_POINT ( 'NONE',  ( 17.50982737979214932, -2.500000000000000000, 4.074750942089497840 ) ) ;
#127374 = ORIENTED_EDGE ( 'NONE', *, *, #123720, .F. ) ;
#127375 = ADVANCED_FACE ( 'NONE', ( #124822 ), #40550, .T. ) ;
#127376 = VERTEX_POINT ( 'NONE', #36457 ) ;
#127377 = ORIENTED_EDGE ( 'NONE', *, *, #120908, .T. ) ;
#127378 = DIRECTION ( 'NONE',  ( 0.000000000000000000, 1.000000000000000000, 0.000000000000000000 ) ) ;
#127379 = DIRECTION ( 'NONE',  ( 0.000000000000000000, 1.000000000000000000, 0.000000000000000000 ) ) ;
#127380 = CARTESIAN_POINT ( 'NONE',  ( -10.85000000000000142, 12.50000000000000000, -2.165063509461097713 ) ) ;
#127381 = AXIS2_PLACEMENT_3D ( 'NONE', #79434, #81987, #70891 ) ;
#127382 = ORIENTED_EDGE ( 'NONE', *, *, #65797, .T. ) ;
#127383 = CARTESIAN_POINT ( 'NONE',  ( 15.40649769424558180, 2.500000000000000444, -5.817321162632842935 ) ) ;
#127384 = DIRECTION ( 'NONE',  ( 0.000000000000000000, 0.000000000000000000, 1.000000000000000000 ) ) ;
#127387 = CONICAL_SURFACE ( 'NONE', #31246, 0.1000000000000000472, 0.003490658503988666988 ) ;
#127386 = CARTESIAN_POINT ( 'NONE',  ( -10.65000000000000391, 12.50000000000000000, -1.818653347947322141 ) ) ;
#127385 = CONICAL_SURFACE ( 'NONE', #54224, 0.1000000000000002554, 0.003490658503988666988 ) ;
#127388 = CARTESIAN_POINT ( 'NONE',  ( 186.3177083336747160, 4.367472073101515306, 7.564683531250000925 ) ) ;
#127389 = CARTESIAN_POINT ( 'NONE',  ( 12.69999999999990337, 2.500000000000000000, 3.983716857408420076 ) ) ;
#127390 = DIRECTION ( 'NONE',  ( 0.000000000000000000, 0.000000000000000000, 1.000000000000000000 ) ) ;
#127391 = AXIS2_PLACEMENT_3D ( 'NONE', #76327, #28519, #88042 ) ;
#127392 = DIRECTION ( 'NONE',  ( 0.000000000000000000, -0.9999939076577903929, 0.003490651415223739937 ) ) ;
#127393 = EDGE_LOOP ( 'NONE', ( #60705, #69855, #22132, #126608 ) ) ;
#127394 = CARTESIAN_POINT ( 'NONE',  ( -14.99999999999998401, 2.500000000000000000, 0.5928203230275517210 ) ) ;
#127395 = CONICAL_SURFACE ( 'NONE', #129568, 0.1000000000000002554, 0.003490658503988666988 ) ;
#127396 = ORIENTED_EDGE ( 'NONE', *, *, #102182, .T. ) ;
#127397 = ORIENTED_EDGE ( 'NONE', *, *, #94189, .F. ) ;
#127398 = FACE_OUTER_BOUND ( 'NONE', #124557, .T. ) ;
#127399 = DIRECTION ( 'NONE',  ( -0.000000000000000000, -1.000000000000000000, -0.000000000000000000 ) ) ;
#127400 = CARTESIAN_POINT ( 'NONE',  ( 176.5000000000000000, 0.000000000000000000, -4.000000000000000000 ) ) ;
#127401 = ORIENTED_EDGE ( 'NONE', *, *, #57417, .T. ) ;
#127402 = ORIENTED_EDGE ( 'NONE', *, *, #25632, .T. ) ;
#127403 = CARTESIAN_POINT ( 'NONE',  ( 3.149999999999946176, 12.50000000000000000, -6.841600689897077814 ) ) ;
#127404 = DIRECTION ( 'NONE',  ( 0.000000000000000000, 0.000000000000000000, 1.000000000000000000 ) ) ;
#127405 = DIRECTION ( 'NONE',  ( 0.000000000000000000, 0.000000000000000000, -1.000000000000000000 ) ) ;
#127406 = ORIENTED_EDGE ( 'NONE', *, *, #47768, .T. ) ;
#127407 = EDGE_LOOP ( 'NONE', ( #22939, #62012, #65838, #38594 ) ) ;
#127408 = DIRECTION ( 'NONE',  ( 0.000000000000000000, 0.000000000000000000, -1.000000000000000000 ) ) ;
#127409 = EDGE_LOOP ( 'NONE', ( #33561, #102509, #123231, #112514 ) ) ;
#127410 = CARTESIAN_POINT ( 'NONE',  ( -12.04999999999999716, 12.50000000000000000, -2.165063509461097713 ) ) ;
#127411 = CONICAL_SURFACE ( 'NONE', #10331, 0.1000000000000002554, 0.003490658503988666988 ) ;
#127412 = ADVANCED_FACE ( 'NONE', ( #33850 ), #24046, .T. ) ;
#127414 = DIRECTION ( 'NONE',  ( -0.000000000000000000, 1.000000000000000000, -0.000000000000000000 ) ) ;
#127413 = AXIS2_PLACEMENT_3D ( 'NONE', #1214, #32645, #120358 ) ;
#127415 = ORIENTED_EDGE ( 'NONE', *, *, #19270, .F. ) ;
#127416 = CARTESIAN_POINT ( 'NONE',  ( 2.499999999999983569, 12.50000000000000000, -4.395220292106239768 ) ) ;
#127417 = LINE ( 'NONE', #46265, #52490 ) ;
#127418 = DIRECTION ( 'NONE',  ( 1.000000000000000000, 0.000000000000000000, 0.000000000000000000 ) ) ;
#127419 = ADVANCED_FACE ( 'NONE', ( #113709 ), #54144, .T. ) ;
#127420 = CARTESIAN_POINT ( 'NONE',  ( 11.04999999999990834, 2.500000000000000000, 1.718653347947321386 ) ) ;
#127421 = EDGE_CURVE ( 'NONE', #11702, #14788, #13318, .T. ) ;
#127422 = CONICAL_SURFACE ( 'NONE', #2011, 0.1000000000000002554, 0.003490658503988666988 ) ;
#127423 = ORIENTED_EDGE ( 'NONE', *, *, #47504, .T. ) ;
#127424 = AXIS2_PLACEMENT_3D ( 'NONE', #4387, #86838, #98574 ) ;
#127425 = CARTESIAN_POINT ( 'NONE',  ( -8.550000000000014921, 2.500000000000000000, -6.148780366869520897 ) ) ;
#127426 = ADVANCED_FACE ( 'NONE', ( #46245 ), #13557, .T. ) ;
#127427 = ORIENTED_EDGE ( 'NONE', *, *, #39691, .F. ) ;
#127428 = ADVANCED_FACE ( 'NONE', ( #4362 ), #99014, .T. ) ;
#127429 = VERTEX_POINT ( 'NONE', #124167 ) ;
#127430 = ADVANCED_FACE ( 'NONE', ( #35164 ), #90596, .T. ) ;
#127431 = LINE ( 'NONE', #69134, #45801 ) ;
#127433 = EDGE_CURVE ( 'NONE', #120216, #70218, #103218, .T. ) ;
#127432 = CARTESIAN_POINT ( 'NONE',  ( -12.49999999999999467, 2.500000000000000000, 0.6928203230275535862 ) ) ;
#127434 = CARTESIAN_POINT ( 'NONE',  ( 15.59999999999988951, 12.50000000000000000, 0.3464101615137735735 ) ) ;
#127435 = EDGE_CURVE ( 'NONE', #119776, #92740, #34189, .T. ) ;
#127436 = CARTESIAN_POINT ( 'NONE',  ( -6.850000000000013856, 2.500000000000000000, 6.941600689897073018 ) ) ;
#127437 = CONICAL_SURFACE ( 'NONE', #93975, 0.1000000000000000472, 0.003490658503988666988 ) ;
#127438 = DIRECTION ( 'NONE',  ( 0.000000000000000000, -0.9999939076577903929, 0.003490651415223739937 ) ) ;
#127439 = FACE_OUTER_BOUND ( 'NONE', #26203, .T. ) ;
#127440 = AXIS2_PLACEMENT_3D ( 'NONE', #40201, #98450, #80121 ) ;
#127441 = CIRCLE ( 'NONE', #14544, 0.1000000000000002554 ) ;
#127442 = DIRECTION ( 'NONE',  ( 0.000000000000000000, 1.000000000000000000, 0.000000000000000000 ) ) ;
#127443 = DIRECTION ( 'NONE',  ( 0.000000000000000000, 1.000000000000000000, 0.000000000000000000 ) ) ;
#127444 = DIRECTION ( 'NONE',  ( -0.000000000000000000, -1.000000000000000000, -0.000000000000000000 ) ) ;
#127445 = EDGE_CURVE ( 'NONE', #120897, #12970, #115729, .T. ) ;
#127446 = DIRECTION ( 'NONE',  ( 0.000000000000000000, -0.000000000000000000, 1.000000000000000000 ) ) ;
#127447 = ORIENTED_EDGE ( 'NONE', *, *, #64657, .F. ) ;
#127448 = AXIS2_PLACEMENT_3D ( 'NONE', #14519, #61726, #81983 ) ;
#127449 = DIRECTION ( 'NONE',  ( -0.000000000000000000, -1.000000000000000000, -0.000000000000000000 ) ) ;
#127450 = DIRECTION ( 'NONE',  ( 0.000000000000000000, -0.9999939076577903929, 0.003490651415223739937 ) ) ;
#127451 = DIRECTION ( 'NONE',  ( -0.000000000000000000, -1.000000000000000000, -0.000000000000000000 ) ) ;
#127452 = DIRECTION ( 'NONE',  ( 0.000000000000000000, 0.000000000000000000, -1.000000000000000000 ) ) ;
#127453 = LINE ( 'NONE', #77683, #18706 ) ;
#127454 = ORIENTED_EDGE ( 'NONE', *, *, #94284, .F. ) ;
#127455 = CARTESIAN_POINT ( 'NONE',  ( 11.69999999999990870, 2.500000000000000000, -4.430127018922202176 ) ) ;
#127456 = DIRECTION ( 'NONE',  ( 0.000000000000000000, 0.000000000000000000, 1.000000000000000000 ) ) ;
#127458 = ORIENTED_EDGE ( 'NONE', *, *, #93307, .F. ) ;
#127457 = CARTESIAN_POINT ( 'NONE',  ( -12.09999999999999432, 2.500000000000000000, 3.537306695894645081 ) ) ;
#127459 =( REPRESENTATION_RELATIONSHIP ('NONE','NONE', #102928, #1094 ) REPRESENTATION_RELATIONSHIP_WITH_TRANSFORMATION ( #97457 )SHAPE_REPRESENTATION_RELATIONSHIP( ) );
#127460 = VERTEX_POINT ( 'NONE', #128718 ) ;
#127461 = ORIENTED_EDGE ( 'NONE', *, *, #80354, .T. ) ;
#127462 = VERTEX_POINT ( 'NONE', #116270 ) ;
#127463 = ORIENTED_EDGE ( 'NONE', *, *, #11842, .T. ) ;
#127464 = DIRECTION ( 'NONE',  ( -4.274815082592931898E-19, -0.9999939076577903929, -0.003490651415223739937 ) ) ;
#127465 = EDGE_CURVE ( 'NONE', #51670, #8233, #76031, .T. ) ;
#127466 = ADVANCED_FACE ( 'NONE', ( #17415 ), #44644, .T. ) ;
#127467 = CIRCLE ( 'NONE', #71037, 0.09999999999999982514 ) ;
#127468 = CARTESIAN_POINT ( 'NONE',  ( -8.150000000000012790, 2.500000000000000000, 1.918653347947321564 ) ) ;
#127470 = EDGE_CURVE ( 'NONE', #84006, #103567, #42604, .T. ) ;
#127469 = DIRECTION ( 'NONE',  ( 0.000000000000000000, 0.000000000000000000, -1.000000000000000000 ) ) ;
#127471 = DIRECTION ( 'NONE',  ( 0.000000000000000000, -0.9999939076577903929, 0.003490651415223739937 ) ) ;
#127472 = ORIENTED_EDGE ( 'NONE', *, *, #72842, .T. ) ;
#127473 = EDGE_CURVE ( 'NONE', #86071, #101564, #66527, .T. ) ;
#127474 = AXIS2_PLACEMENT_3D ( 'NONE', #113649, #74368, #102533 ) ;
#127475 = DIRECTION ( 'NONE',  ( 0.000000000000000000, -0.000000000000000000, 1.000000000000000000 ) ) ;
#127476 = ORIENTED_EDGE ( 'NONE', *, *, #96981, .F. ) ;
#127477 = CARTESIAN_POINT ( 'NONE',  ( 24.00496409366837369, -0.9037364216029228903, -4.313973893095000456 ) ) ;
#127479 = AXIS2_PLACEMENT_3D ( 'NONE', #110772, #121250, #98369 ) ;
#127478 = CARTESIAN_POINT ( 'NONE',  ( 15.40649769424532245, -2.500000000000000444, -5.817321162632588916 ) ) ;
#127480 = CARTESIAN_POINT ( 'NONE',  ( 9.599999999999914380, 12.50000000000000000, 5.022947341949748790 ) ) ;
#127481 = PLANE ( 'NONE',  #96548 ) ;
#127482 = EDGE_CURVE ( 'NONE', #14578, #72759, #122006, .T. ) ;
#127483 = DIRECTION ( 'NONE',  ( -0.000000000000000000, 1.000000000000000000, -0.000000000000000000 ) ) ;
#127484 = EDGE_CURVE ( 'NONE', #46669, #7958, #716, .T. ) ;
#127485 = ORIENTED_EDGE ( 'NONE', *, *, #24710, .F. ) ;
#127486 = AXIS2_PLACEMENT_3D ( 'NONE', #83344, #13930, #63699 ) ;
#127487 = EDGE_CURVE ( 'NONE', #79310, #114635, #128038, .T. ) ;
#127488 = EDGE_CURVE ( 'NONE', #93002, #78911, #68459, .T. ) ;
#127489 = ORIENTED_EDGE ( 'NONE', *, *, #8794, .F. ) ;
#127490 = ORIENTED_EDGE ( 'NONE', *, *, #16891, .T. ) ;
#127491 = ORIENTED_EDGE ( 'NONE', *, *, #86209, .T. ) ;
#127492 = CARTESIAN_POINT ( 'NONE',  ( -9.999999999999971578, 2.500000000000000000, -4.430127018922197735 ) ) ;
#127493 = LINE ( 'NONE', #126844, #62420 ) ;
#127494 = DIRECTION ( 'NONE',  ( 0.000000000000000000, 1.000000000000000000, 0.000000000000000000 ) ) ;
#127495 = FACE_BOUND ( 'NONE', #1243, .T. ) ;
#127496 = FACE_OUTER_BOUND ( 'NONE', #88548, .T. ) ;
#127497 = CARTESIAN_POINT ( 'NONE',  ( 1.649999999999948841, 12.50000000000000000, 6.495190528383297135 ) ) ;
#127498 = EDGE_CURVE ( 'NONE', #54010, #65711, #46796, .T. ) ;
#127499 = CARTESIAN_POINT ( 'NONE',  ( -6.650000000000018119, 12.50000000000000000, -7.122917578226816815 ) ) ;
#127500 = DIRECTION ( 'NONE',  ( -0.000000000000000000, -1.000000000000000000, -0.000000000000000000 ) ) ;
#127501 = CARTESIAN_POINT ( 'NONE',  ( 185.8385416670080872, 6.551208109652274736, 3.782341765625001351 ) ) ;
#127502 = CARTESIAN_POINT ( 'NONE',  ( 6.849999999999927702, 2.500000000000000000, 2.511473670974873507 ) ) ;
#127503 = DIRECTION ( 'NONE',  ( -0.000000000000000000, -1.000000000000000000, -0.000000000000000000 ) ) ;
#127504 = CONICAL_SURFACE ( 'NONE', #20892, 0.09999999999999982514, 0.003490658503988666988 ) ;
#127505 = VECTOR ( 'NONE', #29030, 1000.000000000000000 ) ;
#127506 = CARTESIAN_POINT ( 'NONE',  ( 8.349999999999919709, 12.50000000000000000, 7.188010851410848723 ) ) ;
#127507 = VERTEX_POINT ( 'NONE', #38390 ) ;
#127508 = ORIENTED_EDGE ( 'NONE', *, *, #19719, .T. ) ;
#127509 = VERTEX_POINT ( 'NONE', #107091 ) ;
#127510 = ORIENTED_EDGE ( 'NONE', *, *, #100296, .T. ) ;
#127511 = PLANE ( 'NONE',  #90406 ) ;
#127512 = EDGE_CURVE ( 'NONE', #118058, #27024, #57364, .T. ) ;
#127513 = FACE_BOUND ( 'NONE', #17762, .T. ) ;
#127514 = CIRCLE ( 'NONE', #27158, 0.1000000000000000056 ) ;
#127515 = CARTESIAN_POINT ( 'NONE',  ( 145.7653593504141725, 2.500000000000000000, -3.576063159858998475 ) ) ;
#127516 = ORIENTED_EDGE ( 'NONE', *, *, #79002, .F. ) ;
#127517 = FACE_OUTER_BOUND ( 'NONE', #113012, .T. ) ;
#127518 = DIRECTION ( 'NONE',  ( 0.000000000000000000, 0.000000000000000000, -1.000000000000000000 ) ) ;
#127519 = DIRECTION ( 'NONE',  ( 0.000000000000000000, 1.000000000000000000, 0.000000000000000000 ) ) ;
#127520 = AXIS2_PLACEMENT_3D ( 'NONE', #103197, #93383, #120899 ) ;
#127521 = ORIENTED_EDGE ( 'NONE', *, *, #459, .F. ) ;
#127522 = CARTESIAN_POINT ( 'NONE',  ( 187.5000000000000000, 0.000000000000000000, 7.700000000000000178 ) ) ;
#127523 = CARTESIAN_POINT ( 'NONE',  ( 19.01901804971389609, 2.576149587736915159, -2.431039412660902510 ) ) ;
#127524 = AXIS2_PLACEMENT_3D ( 'NONE', #3360, #65492, #13807 ) ;
#127525 = ADVANCED_FACE ( 'NONE', ( #56690 ), #80245, .T. ) ;
#127526 = ORIENTED_EDGE ( 'NONE', *, *, #21939, .T. ) ;
#127527 = CARTESIAN_POINT ( 'NONE',  ( -10.84999999999999964, 2.500000000000000000, 1.472243186433545459 ) ) ;
#127528 = DIRECTION ( 'NONE',  ( 0.000000000000000000, 0.000000000000000000, -1.000000000000000000 ) ) ;
#127529 = AXIS2_PLACEMENT_3D ( 'NONE', #117144, #55021, #27478 ) ;
#127530 = VERTEX_POINT ( 'NONE', #7608 ) ;
#127531 = DIRECTION ( 'NONE',  ( -0.000000000000000000, 1.000000000000000000, -0.000000000000000000 ) ) ;
#127532 = CARTESIAN_POINT ( 'NONE',  ( 9.799999999999915445, 12.50000000000000000, -4.676537180435977881 ) ) ;
#127533 = ORIENTED_EDGE ( 'NONE', *, *, #30711, .F. ) ;
#127534 = CARTESIAN_POINT ( 'NONE',  ( -4.250072516143177381E-14, 2.500000000000000000, -3.637306695894650055 ) ) ;
#127535 = AXIS2_PLACEMENT_3D ( 'NONE', #30770, #1918, #81145 ) ;
#127536 = ORIENTED_EDGE ( 'NONE', *, *, #13783, .F. ) ;
#127537 = EDGE_LOOP ( 'NONE', ( #108654, #104630, #8228, #126710 ) ) ;
#127538 = EDGE_CURVE ( 'NONE', #26625, #18141, #73977, .T. ) ;
#127539 = DIRECTION ( 'NONE',  ( -0.000000000000000000, -1.000000000000000000, -0.000000000000000000 ) ) ;
#127540 = ORIENTED_EDGE ( 'NONE', *, *, #40950, .T. ) ;
#127541 = DIRECTION ( 'NONE',  ( 0.000000000000000000, 1.000000000000000000, 0.000000000000000000 ) ) ;
#127542 = FACE_BOUND ( 'NONE', #65395, .T. ) ;
#127543 = ORIENTED_EDGE ( 'NONE', *, *, #55468, .F. ) ;
#127544 = CARTESIAN_POINT ( 'NONE',  ( 112.7275879503070115, 7.525284458381443109, -1.660393549188459383 ) ) ;
#127545 = ORIENTED_EDGE ( 'NONE', *, *, #54881, .F. ) ;
#127546 = DIRECTION ( 'NONE',  ( 1.000000000000000000, 0.000000000000000000, 0.000000000000000000 ) ) ;
#127547 = DIRECTION ( 'NONE',  ( 0.000000000000000000, 0.000000000000000000, 1.000000000000000000 ) ) ;
#127548 = DIRECTION ( 'NONE',  ( 0.000000000000000000, 0.000000000000000000, 1.000000000000000000 ) ) ;
#127549 = DIRECTION ( 'NONE',  ( 0.000000000000000000, 1.000000000000000000, 0.000000000000000000 ) ) ;
#127550 = CARTESIAN_POINT ( 'NONE',  ( -5.400000000000023448, 12.50000000000000000, -4.957854068765716882 ) ) ;
#127551 = ORIENTED_EDGE ( 'NONE', *, *, #96124, .F. ) ;
#127552 = VERTEX_POINT ( 'NONE', #29213 ) ;
#127553 = CARTESIAN_POINT ( 'NONE',  ( 1.049999999999954081, 2.500000000000000000, -6.148780366869526226 ) ) ;
#127554 = CARTESIAN_POINT ( 'NONE',  ( 16.86635082839108080, -0.4716143926291173072, 5.778906370536277315 ) ) ;
#127556 = CARTESIAN_POINT ( 'NONE',  ( 7.949999999999922018, 12.50000000000000000, 6.560283801567334372 ) ) ;
#127555 = AXIS2_PLACEMENT_3D ( 'NONE', #47566, #117551, #116921 ) ;
#127558 = VERTEX_POINT ( 'NONE', #26614 ) ;
#127557 = VERTEX_POINT ( 'NONE', #126759 ) ;
#127559 = EDGE_LOOP ( 'NONE', ( #49663, #86155, #24110, #54367 ) ) ;
#127560 = CONICAL_SURFACE ( 'NONE', #41891, 0.09999999999999982514, 0.003490658503988666988 ) ;
#127561 = CARTESIAN_POINT ( 'NONE',  ( 13.94999999999989448, 2.500000000000000000, -2.411473670974877859 ) ) ;
#127562 = CARTESIAN_POINT ( 'NONE',  ( -4.150000000000024336, 2.500000000000000000, -2.857883832488653741 ) ) ;
#127563 = EDGE_CURVE ( 'NONE', #97855, #107047, #7053, .T. ) ;
#127565 = AXIS2_PLACEMENT_3D ( 'NONE', #72923, #113483, #23167 ) ;
#127564 = AXIS2_PLACEMENT_3D ( 'NONE', #19927, #120694, #71593 ) ;
#127566 = CARTESIAN_POINT ( 'NONE',  ( -9.400000000000009237, 2.500000000000000000, -4.083716857408422385 ) ) ;
#127567 = DIRECTION ( 'NONE',  ( 0.000000000000000000, 0.000000000000000000, 1.000000000000000000 ) ) ;
#127568 = DIRECTION ( 'NONE',  ( -0.000000000000000000, -1.000000000000000000, -0.000000000000000000 ) ) ;
#127569 = CARTESIAN_POINT ( 'NONE',  ( 6.249999999999932498, 2.500000000000000000, -5.802370205355749988 ) ) ;
#127570 = CARTESIAN_POINT ( 'NONE',  ( 2.699999999999944666, 2.500000000000000000, 4.676537180435972552 ) ) ;
#127571 = CARTESIAN_POINT ( 'NONE',  ( 184.6145833340161175, 6.668395609140177704, -3.849999999999998312 ) ) ;
#127572 = ADVANCED_FACE ( 'NONE', ( #69108 ), #804, .T. ) ;
#127573 = ORIENTED_EDGE ( 'NONE', *, *, #115858, .T. ) ;
#127574 = VERTEX_POINT ( 'NONE', #47553 ) ;
#127575 = FACE_OUTER_BOUND ( 'NONE', #7904, .T. ) ;
#127576 = DIRECTION ( 'NONE',  ( 1.000000000000000000, 0.000000000000000000, 0.000000000000000000 ) ) ;
#127577 = ADVANCED_FACE ( 'NONE', ( #37729 ), #77631, .T. ) ;
#127578 = ORIENTED_EDGE ( 'NONE', *, *, #49029, .T. ) ;
#127579 = EDGE_CURVE ( 'NONE', #53467, #25412, #9130, .T. ) ;
#127580 = ORIENTED_EDGE ( 'NONE', *, *, #4481, .T. ) ;
#127581 = EDGE_CURVE ( 'NONE', #67817, #71756, #98549, .T. ) ;
#127582 = CARTESIAN_POINT ( 'NONE',  ( 186.9843750003414300, -8.734944146203032389, -1.604583208406768146E-15 ) ) ;
#127584 = ADVANCED_FACE ( 'NONE', ( #20670 ), #111633, .T. ) ;
#127583 = DIRECTION ( 'NONE',  ( 0.000000000000000000, -0.9999939076577903929, 0.003490651415223739937 ) ) ;
#127585 = DIRECTION ( 'NONE',  ( 0.000000000000000000, -0.9999939076577903929, 0.003490651415223739937 ) ) ;
#127586 = DIRECTION ( 'NONE',  ( 0.000000000000000000, 0.000000000000000000, -1.000000000000000000 ) ) ;
#127587 = LINE ( 'NONE', #37911, #109221 ) ;
#127588 = DIRECTION ( 'NONE',  ( 0.000000000000000000, 0.000000000000000000, 1.000000000000000000 ) ) ;
#127589 = LINE ( 'NONE', #68663, #84480 ) ;
#127590 = ORIENTED_EDGE ( 'NONE', *, *, #39093, .F. ) ;
#127591 = CARTESIAN_POINT ( 'NONE',  ( -9.150000000000009237, 2.500000000000000000, -6.395190528383296602 ) ) ;
#127592 = EDGE_CURVE ( 'NONE', #12208, #21305, #113781, .T. ) ;
#127594 = EDGE_CURVE ( 'NONE', #105260, #98489, #117875, .T. ) ;
#127593 = CARTESIAN_POINT ( 'NONE',  ( 11.44999999999990514, 12.50000000000000000, -6.148780366869526226 ) ) ;
#127595 = CIRCLE ( 'NONE', #96184, 0.5000000000000000000 ) ;
#127596 = EDGE_CURVE ( 'NONE', #76681, #3042, #121428, .T. ) ;
#127598 = VERTEX_POINT ( 'NONE', #109695 ) ;
#127597 = AXIS2_PLACEMENT_3D ( 'NONE', #73161, #74449, #112450 ) ;
#127599 = ORIENTED_EDGE ( 'NONE', *, *, #38193, .F. ) ;
#127600 = ORIENTED_EDGE ( 'NONE', *, *, #38427, .F. ) ;
#127601 = ORIENTED_EDGE ( 'NONE', *, *, #120188, .T. ) ;
#127602 = DIRECTION ( 'NONE',  ( 0.000000000000000000, 0.000000000000000000, -1.000000000000000000 ) ) ;
#127603 = DIRECTION ( 'NONE',  ( 0.000000000000000000, 1.000000000000000000, 0.000000000000000000 ) ) ;
#127604 = VECTOR ( 'NONE', #52935, 1000.000000000000000 ) ;
#127605 = ORIENTED_EDGE ( 'NONE', *, *, #92829, .T. ) ;
#127606 = DIRECTION ( 'NONE',  ( -0.000000000000000000, -1.000000000000000000, -0.000000000000000000 ) ) ;
#127607 = CARTESIAN_POINT ( 'NONE',  ( 2.500000000000002220, -0.9166666666666694052, -9.999999999999998224 ) ) ;
#127608 = DIRECTION ( 'NONE',  ( 0.000000000000000000, 0.000000000000000000, 1.000000000000000000 ) ) ;
#127610 = ORIENTED_EDGE ( 'NONE', *, *, #127433, .F. ) ;
#127609 = CARTESIAN_POINT ( 'NONE',  ( -14.54999999999998472, 12.50000000000000000, -2.099970236277062252 ) ) ;
#127611 = DIRECTION ( 'NONE',  ( 0.000000000000000000, -0.9999939076577903929, 0.003490651415223739937 ) ) ;
#127612 = DIRECTION ( 'NONE',  ( 0.000000000000000000, 0.000000000000000000, -1.000000000000000000 ) ) ;
#127613 = ORIENTED_EDGE ( 'NONE', *, *, #127066, .F. ) ;
#127614 = AXIS2_PLACEMENT_3D ( 'NONE', #68867, #43153, #69503 ) ;
#127615 = ORIENTED_EDGE ( 'NONE', *, *, #7997, .F. ) ;
#127616 = ORIENTED_EDGE ( 'NONE', *, *, #107949, .T. ) ;
#127617 = DIRECTION ( 'NONE',  ( 0.000000000000000000, 1.000000000000000000, 0.000000000000000000 ) ) ;
#127618 = AXIS2_PLACEMENT_3D ( 'NONE', #118452, #8487, #38639 ) ;
#127619 = DIRECTION ( 'NONE',  ( 0.000000000000000000, 1.000000000000000000, 0.000000000000000000 ) ) ;
#127620 = CIRCLE ( 'NONE', #89961, 0.1000000000000002554 ) ;
#127621 = ORIENTED_EDGE ( 'NONE', *, *, #104778, .T. ) ;
#127622 = FACE_OUTER_BOUND ( 'NONE', #46799, .T. ) ;
#127623 = DIRECTION ( 'NONE',  ( -0.000000000000000000, -1.000000000000000000, -0.000000000000000000 ) ) ;
#127624 = FACE_OUTER_BOUND ( 'NONE', #111526, .T. ) ;
#127625 = CARTESIAN_POINT ( 'NONE',  ( 105.6184301395928031, 8.500000000000000000, 1.375000000000001110 ) ) ;
#127626 = ADVANCED_FACE ( 'NONE', ( #119495 ), #84441, .T. ) ;
#127627 = EDGE_CURVE ( 'NONE', #26903, #110184, #69760, .T. ) ;
#127628 = VERTEX_POINT ( 'NONE', #100501 ) ;
#127629 = DIRECTION ( 'NONE',  ( -0.000000000000000000, 1.000000000000000000, -0.000000000000000000 ) ) ;
#127630 = ADVANCED_FACE ( 'NONE', ( #40971 ), #44739, .T. ) ;
#127631 = ORIENTED_EDGE ( 'NONE', *, *, #64795, .T. ) ;
#127632 = ORIENTED_EDGE ( 'NONE', *, *, #76212, .T. ) ;
#127633 = DIRECTION ( 'NONE',  ( 0.000000000000000000, 0.000000000000000000, 1.000000000000000000 ) ) ;
#127634 = FACE_OUTER_BOUND ( 'NONE', #9636, .T. ) ;
#127635 = FACE_BOUND ( 'NONE', #62890, .T. ) ;
#127636 = CARTESIAN_POINT ( 'NONE',  ( -13.74999999999998757, 12.50000000000000000, -2.857883832488651521 ) ) ;
#127637 = PLANE ( 'NONE',  #123852 ) ;
#127638 = EDGE_CURVE ( 'NONE', #66996, #27297, #120790, .T. ) ;
#127639 = DIRECTION ( 'NONE',  ( 0.000000000000000000, 0.000000000000000000, -1.000000000000000000 ) ) ;
#127640 = VECTOR ( 'NONE', #54003, 1000.000000000000000 ) ;
#127642 = ORIENTED_EDGE ( 'NONE', *, *, #45471, .F. ) ;
#127641 = CONICAL_SURFACE ( 'NONE', #94192, 0.1000000000000002554, 0.003490658503988666988 ) ;
#127644 = CIRCLE ( 'NONE', #92133, 0.06509327318403745899 ) ;
#127643 = CARTESIAN_POINT ( 'NONE',  ( -9.350000000000006750, 2.500000000000000000, -2.511473670974877948 ) ) ;
#127645 = DIRECTION ( 'NONE',  ( -4.274815082592931898E-19, -0.9999939076577903929, -0.003490651415223739937 ) ) ;
#127646 = FACE_OUTER_BOUND ( 'NONE', #30726, .T. ) ;
#127647 = DIRECTION ( 'NONE',  ( -0.000000000000000000, 1.000000000000000000, -0.000000000000000000 ) ) ;
#127648 = ORIENTED_EDGE ( 'NONE', *, *, #107484, .T. ) ;
#127649 = DIRECTION ( 'NONE',  ( 0.000000000000000000, 0.000000000000000000, 1.000000000000000000 ) ) ;
#127650 = CONICAL_SURFACE ( 'NONE', #81680, 0.1000000000000002554, 0.003490658503988666988 ) ;
#127651 = DIRECTION ( 'NONE',  ( 0.000000000000000000, 0.000000000000000000, 1.000000000000000000 ) ) ;
#127652 = ORIENTED_EDGE ( 'NONE', *, *, #83984, .T. ) ;
#127653 = ORIENTED_EDGE ( 'NONE', *, *, #110806, .F. ) ;
#127654 = DIRECTION ( 'NONE',  ( -4.274815082592931898E-19, -0.9999939076577903929, -0.003490651415223739937 ) ) ;
#127655 = CARTESIAN_POINT ( 'NONE',  ( 9.999999999999948486, 12.50000000000000000, -4.330127018922201643 ) ) ;
#127656 = ADVANCED_FACE ( 'NONE', ( #21295 ), #120153, .T. ) ;
#127657 = FACE_BOUND ( 'NONE', #20865, .T. ) ;
#127658 = CARTESIAN_POINT ( 'NONE',  ( 4.999999999999935163, 2.500000000000000000, 3.637306695894644726 ) ) ;
#127659 = EDGE_LOOP ( 'NONE', ( #72131, #74081, #86424, #9350 ) ) ;
#127660 = DIRECTION ( 'NONE',  ( 0.000000000000000000, -0.9999939076577903929, 0.003490651415223739937 ) ) ;
#127661 = EDGE_LOOP ( 'NONE', ( #61212, #50856, #82422, #6188 ) ) ;
#127662 = VERTEX_POINT ( 'NONE', #30507 ) ;
#127663 = DIRECTION ( 'NONE',  ( -0.000000000000000000, -1.000000000000000000, -0.000000000000000000 ) ) ;
#127664 = CARTESIAN_POINT ( 'NONE',  ( 186.2500000000000000, 9.429780353434619030E-16, -7.700000000000000178 ) ) ;
#127665 = ORIENTED_EDGE ( 'NONE', *, *, #53007, .F. ) ;
#127666 = DIRECTION ( 'NONE',  ( -0.000000000000000000, -1.000000000000000000, -0.000000000000000000 ) ) ;
#127667 = DIRECTION ( 'NONE',  ( -0.000000000000000000, 1.000000000000000000, -0.000000000000000000 ) ) ;
#127668 = EDGE_CURVE ( 'NONE', #50344, #57584, #110330, .T. ) ;
#127669 = FACE_OUTER_BOUND ( 'NONE', #66797, .T. ) ;
#127670 = LINE ( 'NONE', #119145, #11266 ) ;
#127671 = CIRCLE ( 'NONE', #18909, 0.1000000000000000472 ) ;
#127672 = EDGE_CURVE ( 'NONE', #62361, #1969, #61473, .T. ) ;
#127673 = CIRCLE ( 'NONE', #123555, 0.09999999999999982514 ) ;
#127674 = ORIENTED_EDGE ( 'NONE', *, *, #53101, .T. ) ;
#127675 = DIRECTION ( 'NONE',  ( 0.000000000000000000, 1.000000000000000000, 0.000000000000000000 ) ) ;
#127676 = DIRECTION ( 'NONE',  ( 0.000000000000000000, 1.000000000000000000, 0.000000000000000000 ) ) ;
#127677 = CARTESIAN_POINT ( 'NONE',  ( -5.600000000000023626, 12.50000000000000000, -4.676537180435977881 ) ) ;
#127678 = CARTESIAN_POINT ( 'NONE',  ( -6.250000000000019540, 2.500000000000000000, -2.757883832488654097 ) ) ;
#127679 = VERTEX_POINT ( 'NONE', #354 ) ;
#127680 = DIRECTION ( 'NONE',  ( 0.000000000000000000, 0.000000000000000000, 1.000000000000000000 ) ) ;
#127681 = EDGE_LOOP ( 'NONE', ( #24638, #96004, #62339, #115991 ) ) ;
#127682 = EDGE_CURVE ( 'NONE', #59852, #37316, #32230, .T. ) ;
#127683 = DIRECTION ( 'NONE',  ( -0.000000000000000000, 1.000000000000000000, -0.000000000000000000 ) ) ;
#127684 = CIRCLE ( 'NONE', #100497, 0.09999999999999982514 ) ;
#127685 = VERTEX_POINT ( 'NONE', #89175 ) ;
#127686 = CARTESIAN_POINT ( 'NONE',  ( -10.65000000000000391, 2.500000000000000000, -6.148780366869522673 ) ) ;
#127687 = CIRCLE ( 'NONE', #58743, 0.06509327318403745899 ) ;
#127688 = DIRECTION ( 'NONE',  ( 0.000000000000000000, 0.000000000000000000, -1.000000000000000000 ) ) ;
#127689 = CARTESIAN_POINT ( 'NONE',  ( 154.1524742528378056, 2.500000000000000000, -1.703575533167231537 ) ) ;
#127690 = LINE ( 'NONE', #68118, #36131 ) ;
#127691 = ORIENTED_EDGE ( 'NONE', *, *, #33778, .F. ) ;
#127692 = DIRECTION ( 'NONE',  ( 0.000000000000000000, 0.000000000000000000, 1.000000000000000000 ) ) ;
#127693 = CARTESIAN_POINT ( 'NONE',  ( 1.249999999999953815, 2.500000000000000000, -2.857883832488653741 ) ) ;
#127694 = EDGE_CURVE ( 'NONE', #58594, #91328, #59425, .T. ) ;
#127695 = FACE_OUTER_BOUND ( 'NONE', #13363, .T. ) ;
#127696 = DIRECTION ( 'NONE',  ( 0.000000000000000000, 0.000000000000000000, 1.000000000000000000 ) ) ;
#127697 = DIRECTION ( 'NONE',  ( -4.274815082592931898E-19, -0.9999939076577903929, -0.003490651415223739937 ) ) ;
#127698 = CIRCLE ( 'NONE', #85830, 0.06509327318403745899 ) ;
#127699 = ORIENTED_EDGE ( 'NONE', *, *, #103376, .F. ) ;
#127700 = ORIENTED_EDGE ( 'NONE', *, *, #16430, .F. ) ;
#127701 = CARTESIAN_POINT ( 'NONE',  ( 2.899999999999946620, 2.500000000000000000, -3.637306695894650055 ) ) ;
#127702 = ORIENTED_EDGE ( 'NONE', *, *, #36732, .F. ) ;
#127703 = CARTESIAN_POINT ( 'NONE',  ( 1.249999999999952038, 2.500000000000000000, 2.857883832488649301 ) ) ;
#127705 = ORIENTED_EDGE ( 'NONE', *, *, #72342, .T. ) ;
#127704 = EDGE_LOOP ( 'NONE', ( #100994, #14909 ) ) ;
#127706 = ORIENTED_EDGE ( 'NONE', *, *, #92685, .T. ) ;
#127707 = DIRECTION ( 'NONE',  ( 0.000000000000000000, 1.000000000000000000, 0.000000000000000000 ) ) ;
#127708 = AXIS2_PLACEMENT_3D ( 'NONE', #103346, #82427, #83700 ) ;
#127709 = CARTESIAN_POINT ( 'NONE',  ( 11.64999999999990443, 2.500000000000000000, 2.957883832488649389 ) ) ;
#127710 = DIRECTION ( 'NONE',  ( -4.274815082592931898E-19, -0.9999939076577903929, -0.003490651415223739937 ) ) ;
#127711 = EDGE_CURVE ( 'NONE', #27444, #2801, #86574, .T. ) ;
#127712 = DIRECTION ( 'NONE',  ( -0.000000000000000000, -1.000000000000000000, -0.000000000000000000 ) ) ;
#127713 = AXIS2_PLACEMENT_3D ( 'NONE', #103694, #23843, #2241 ) ;
#127714 = CARTESIAN_POINT ( 'NONE',  ( -4.150000000000025224, 2.500000000000000000, -1.372243186433550033 ) ) ;
#127715 = FACE_OUTER_BOUND ( 'NONE', #52683, .T. ) ;
#127716 = CARTESIAN_POINT ( 'NONE',  ( -5.800000000000018474, 2.500000000000000000, 4.230127018922196669 ) ) ;
#127717 = CARTESIAN_POINT ( 'NONE',  ( -9.150000000000011013, 12.50000000000000000, -5.802370205355744659 ) ) ;
#127718 = ORIENTED_EDGE ( 'NONE', *, *, #65031, .T. ) ;
#127719 = EDGE_CURVE ( 'NONE', #31303, #7039, #30169, .T. ) ;
#127720 = ORIENTED_EDGE ( 'NONE', *, *, #82875, .F. ) ;
#127721 = VERTEX_POINT ( 'NONE', #98335 ) ;
#127722 = EDGE_LOOP ( 'NONE', ( #39019, #86454, #92491, #47221 ) ) ;
#127723 = LINE ( 'NONE', #106159, #27717 ) ;
#127724 = EDGE_CURVE ( 'NONE', #101537, #73886, #117306, .T. ) ;
#127725 = EDGE_LOOP ( 'NONE', ( #108322, #119070, #96467, #27206 ) ) ;
#127726 = ADVANCED_FACE ( 'NONE', ( #27037 ), #17619, .T. ) ;
#127727 = ORIENTED_EDGE ( 'NONE', *, *, #73753, .T. ) ;
#127728 = EDGE_CURVE ( 'NONE', #73897, #39360, #127807, .T. ) ;
#127729 = EDGE_CURVE ( 'NONE', #67328, #36126, #38144, .T. ) ;
#127730 = PLANE ( 'NONE',  #74887 ) ;
#127731 = CARTESIAN_POINT ( 'NONE',  ( -7.500000000000011546, 2.500000000000000000, 3.737306695894644371 ) ) ;
#127732 = CARTESIAN_POINT ( 'NONE',  ( -4.350000000000027178, 2.500000000000000000, -6.148780366869526226 ) ) ;
#127733 = DIRECTION ( 'NONE',  ( -0.000000000000000000, -1.000000000000000000, -0.000000000000000000 ) ) ;
#127734 = ADVANCED_FACE ( 'NONE', ( #129126 ), #94905, .T. ) ;
#127735 = CIRCLE ( 'NONE', #62987, 0.06509327318403745899 ) ;
#127736 = DIRECTION ( 'NONE',  ( -0.000000000000000000, -1.000000000000000000, -0.000000000000000000 ) ) ;
#127737 = ORIENTED_EDGE ( 'NONE', *, *, #123717, .T. ) ;
#127738 = CONICAL_SURFACE ( 'NONE', #29544, 0.1000000000000000472, 0.003490658503988666988 ) ;
#127739 = CIRCLE ( 'NONE', #121467, 0.09999999999999982514 ) ;
#127740 = EDGE_CURVE ( 'NONE', #103358, #1125, #103315, .T. ) ;
#127741 = EDGE_CURVE ( 'NONE', #117845, #51418, #19694, .T. ) ;
#127742 = DIRECTION ( 'NONE',  ( -0.000000000000000000, 1.000000000000000000, -0.000000000000000000 ) ) ;
#127743 = EDGE_CURVE ( 'NONE', #95554, #55527, #109580, .T. ) ;
#127744 = ORIENTED_EDGE ( 'NONE', *, *, #120851, .T. ) ;
#127745 = DIRECTION ( 'NONE',  ( 0.000000000000000000, 0.000000000000000000, -1.000000000000000000 ) ) ;
#127747 = ADVANCED_FACE ( 'NONE', ( #106862 ), #49270, .T. ) ;
#127746 = CONICAL_SURFACE ( 'NONE', #71299, 0.1000000000000000472, 0.003490658503988666988 ) ;
#127748 = EDGE_LOOP ( 'NONE', ( #102747, #3779 ) ) ;
#127749 = CARTESIAN_POINT ( 'NONE',  ( 3.349999999999945466, 2.500000000000000000, -6.595190528383302109 ) ) ;
#127750 = ORIENTED_EDGE ( 'NONE', *, *, #113217, .T. ) ;
#127751 = AXIS2_PLACEMENT_3D ( 'NONE', #62535, #91334, #71056 ) ;
#127752 = ORIENTED_EDGE ( 'NONE', *, *, #67135, .T. ) ;
#127753 = EDGE_CURVE ( 'NONE', #104203, #35289, #51007, .T. ) ;
#127754 = DIRECTION ( 'NONE',  ( 0.000000000000000000, 1.000000000000000000, 0.000000000000000000 ) ) ;
#127755 = DIRECTION ( 'NONE',  ( 0.000000000000000000, -0.9999939076577903929, 0.003490651415223739937 ) ) ;
#127756 = DIRECTION ( 'NONE',  ( 0.000000000000000000, -0.000000000000000000, 1.000000000000000000 ) ) ;
#127757 = CARTESIAN_POINT ( 'NONE',  ( -10.84999999999999964, 2.500000000000000000, 7.288010851410849256 ) ) ;
#127758 = CARTESIAN_POINT ( 'NONE',  ( 127.5000000000000000, 2.000000000000000000, -4.999999999999998224 ) ) ;
#127759 = ORIENTED_EDGE ( 'NONE', *, *, #61935, .T. ) ;
#127760 = DIRECTION ( 'NONE',  ( 0.000000000000000000, 0.000000000000000000, 1.000000000000000000 ) ) ;
#127761 = DIRECTION ( 'NONE',  ( 0.000000000000000000, 0.000000000000000000, -1.000000000000000000 ) ) ;
#127762 = CARTESIAN_POINT ( 'NONE',  ( 3.099999999999945022, 2.500000000000000000, -4.576537180435978236 ) ) ;
#127763 = DIRECTION ( 'NONE',  ( 0.000000000000000000, 0.000000000000000000, 1.000000000000000000 ) ) ;
#127764 = DIRECTION ( 'NONE',  ( 0.000000000000000000, -0.000000000000000000, 1.000000000000000000 ) ) ;
#127765 = ORIENTED_EDGE ( 'NONE', *, *, #45852, .T. ) ;
#127766 = VECTOR ( 'NONE', #26767, 1000.000000000000000 ) ;
#127767 = ORIENTED_EDGE ( 'NONE', *, *, #56068, .F. ) ;
#127768 = CARTESIAN_POINT ( 'NONE',  ( -8.350000000000008527, 2.500000000000000000, 5.802370205355744659 ) ) ;
#127769 = ORIENTED_EDGE ( 'NONE', *, *, #17340, .F. ) ;
#127770 = DIRECTION ( 'NONE',  ( 0.000000000000000000, 0.000000000000000000, 1.000000000000000000 ) ) ;
#127771 = CONICAL_SURFACE ( 'NONE', #102630, 0.1000000000000000472, 0.003490658503988666988 ) ;
#127772 = DIRECTION ( 'NONE',  ( 0.000000000000000000, -0.9999939076577903929, 0.003490651415223739937 ) ) ;
#127773 = AXIS2_PLACEMENT_3D ( 'NONE', #36952, #25836, #76872 ) ;
#127774 = EDGE_LOOP ( 'NONE', ( #120859, #71706 ) ) ;
#127775 = CARTESIAN_POINT ( 'NONE',  ( 185.2500000000000000, 9.429780353434619030E-16, -7.700000000000000178 ) ) ;
#127776 = CARTESIAN_POINT ( 'NONE',  ( 6.249999999999934275, 12.50000000000000000, -7.188010851410854052 ) ) ;
#127777 = FILL_AREA_STYLE ('',( #6057 ) ) ;
#127778 = CARTESIAN_POINT ( 'NONE',  ( 12.04999999999990834, 12.50000000000000000, -2.165063509461101710 ) ) ;
#127779 = EDGE_LOOP ( 'NONE', ( #91810, #70540, #50507, #15305 ) ) ;
#127780 = VECTOR ( 'NONE', #123439, 1000.000000000000000 ) ;
#127781 = VECTOR ( 'NONE', #87006, 1000.000000000000000 ) ;
#127782 = EDGE_CURVE ( 'NONE', #70962, #111188, #77420, .T. ) ;
#127783 = CARTESIAN_POINT ( 'NONE',  ( 13.09999999999989839, 2.500000000000000000, -0.4464101615137783252 ) ) ;
#127784 = FACE_OUTER_BOUND ( 'NONE', #105913, .T. ) ;
#127785 = EDGE_CURVE ( 'NONE', #33867, #73941, #128379, .T. ) ;
#127786 = ORIENTED_EDGE ( 'NONE', *, *, #78420, .F. ) ;
#127787 = DIRECTION ( 'NONE',  ( -0.000000000000000000, -1.000000000000000000, -0.000000000000000000 ) ) ;
#127788 = DIRECTION ( 'NONE',  ( 0.000000000000000000, -0.9999939076577903929, 0.003490651415223739937 ) ) ;
#127789 = FACE_OUTER_BOUND ( 'NONE', #96554, .T. ) ;
#127790 = CIRCLE ( 'NONE', #98524, 0.1000000000000000472 ) ;
#127791 = ADVANCED_FACE ( 'NONE', ( #57790 ), #92859, .T. ) ;
#127792 = CONICAL_SURFACE ( 'NONE', #117291, 0.09999999999999999167, 0.003490658503988666988 ) ;
#127793 = ORIENTED_EDGE ( 'NONE', *, *, #30858, .F. ) ;
#127794 = FACE_OUTER_BOUND ( 'NONE', #66614, .T. ) ;
#127795 = AXIS2_PLACEMENT_3D ( 'NONE', #22028, #101858, #112327 ) ;
#127796 = VERTEX_POINT ( 'NONE', #108158 ) ;
#127797 = CARTESIAN_POINT ( 'NONE',  ( -12.89999999999999147, 2.500000000000000000, -5.022947341949751454 ) ) ;
#127798 = DIRECTION ( 'NONE',  ( 0.000000000000000000, 0.000000000000000000, 1.000000000000000000 ) ) ;
#127799 = AXIS2_PLACEMENT_3D ( 'NONE', #124750, #84169, #124100 ) ;
#127800 = LINE ( 'NONE', #47966, #16197 ) ;
#127801 = ORIENTED_EDGE ( 'NONE', *, *, #84589, .T. ) ;
#127802 = DIRECTION ( 'NONE',  ( 0.000000000000000000, 0.000000000000000000, 1.000000000000000000 ) ) ;
#127803 = DIRECTION ( 'NONE',  ( 0.000000000000000000, 0.000000000000000000, -1.000000000000000000 ) ) ;
#127804 = CIRCLE ( 'NONE', #52588, 0.1000000000000002554 ) ;
#127805 = CIRCLE ( 'NONE', #102665, 0.09999999999999982514 ) ;
#127806 = ORIENTED_EDGE ( 'NONE', *, *, #72490, .T. ) ;
#127807 = LINE ( 'NONE', #130, #78192 ) ;
#127808 = ORIENTED_EDGE ( 'NONE', *, *, #9680, .F. ) ;
#127809 = DIRECTION ( 'NONE',  ( -0.000000000000000000, -1.000000000000000000, -0.000000000000000000 ) ) ;
#127810 = EDGE_LOOP ( 'NONE', ( #40797, #120461 ) ) ;
#127811 = LINE ( 'NONE', #97065, #117392 ) ;
#127812 = LINE ( 'NONE', #8030, #58399 ) ;
#127813 = ORIENTED_EDGE ( 'NONE', *, *, #110002, .T. ) ;
#127814 = EDGE_LOOP ( 'NONE', ( #107072, #127691, #35231, #121033 ) ) ;
#127815 = DIRECTION ( 'NONE',  ( 0.000000000000000000, 1.000000000000000000, 0.000000000000000000 ) ) ;
#127816 = CARTESIAN_POINT ( 'NONE',  ( 12.89999999999989910, 12.50000000000000000, -0.6928203230275542523 ) ) ;
#127817 = VERTEX_POINT ( 'NONE', #18495 ) ;
#127819 = EDGE_CURVE ( 'NONE', #116265, #34015, #48946, .T. ) ;
#127818 = FACE_OUTER_BOUND ( 'NONE', #126247, .T. ) ;
#127820 = DIRECTION ( 'NONE',  ( -0.000000000000000000, -1.000000000000000000, -0.000000000000000000 ) ) ;
#127821 = AXIS2_PLACEMENT_3D ( 'NONE', #7207, #89018, #47159 ) ;
#127822 = CARTESIAN_POINT ( 'NONE',  ( -10.20000000000000284, 12.50000000000000000, 3.983716857408420964 ) ) ;
#127823 = DIRECTION ( 'NONE',  ( 0.000000000000000000, 1.000000000000000000, 0.000000000000000000 ) ) ;
#127824 = AXIS2_PLACEMENT_3D ( 'NONE', #65926, #6987, #27287 ) ;
#127825 = AXIS2_PLACEMENT_3D ( 'NONE', #51293, #61753, #110820 ) ;
#127826 = DIRECTION ( 'NONE',  ( -0.000000000000000000, 1.000000000000000000, -0.000000000000000000 ) ) ;
#127827 = ADVANCED_FACE ( 'NONE', ( #98993 ), #115828, .T. ) ;
#127828 = DIRECTION ( 'NONE',  ( -0.000000000000000000, 1.000000000000000000, -0.000000000000000000 ) ) ;
#127829 = AXIS2_PLACEMENT_3D ( 'NONE', #100730, #28793, #58256 ) ;
#127830 = ORIENTED_EDGE ( 'NONE', *, *, #116951, .T. ) ;
#127832 = ORIENTED_EDGE ( 'NONE', *, *, #32013, .F. ) ;
#127831 = AXIS2_PLACEMENT_3D ( 'NONE', #24678, #46241, #14189 ) ;
#127833 = VERTEX_POINT ( 'NONE', #60384 ) ;
#127834 = VERTEX_POINT ( 'NONE', #120568 ) ;
#127835 = DIRECTION ( 'NONE',  ( -0.000000000000000000, 1.000000000000000000, -0.000000000000000000 ) ) ;
#127836 = CARTESIAN_POINT ( 'NONE',  ( 3.349999999999941025, 12.50000000000000000, 7.253104124594885960 ) ) ;
#127838 = ADVANCED_FACE ( 'NONE', ( #31547 ), #99119, .T. ) ;
#127837 = AXIS2_PLACEMENT_3D ( 'NONE', #117387, #38897, #67663 ) ;
#127839 = PLANE ( 'NONE',  #78194 ) ;
#127840 = VERTEX_POINT ( 'NONE', #782 ) ;
#127841 = FACE_BOUND ( 'NONE', #78, .T. ) ;
#127842 = ORIENTED_EDGE ( 'NONE', *, *, #71686, .T. ) ;
#127843 = CARTESIAN_POINT ( 'NONE',  ( -4.550000000000022915, 2.500000000000000000, 2.165063509461097713 ) ) ;
#127844 = PLANE ( 'NONE',  #54320 ) ;
#127845 = PLANE ( 'NONE',  #93177 ) ;
#127846 = DIRECTION ( 'NONE',  ( 0.000000000000000000, 0.000000000000000000, -1.000000000000000000 ) ) ;
#127847 = DIRECTION ( 'NONE',  ( 1.000000000000000000, 0.000000000000000000, 0.000000000000000000 ) ) ;
#127848 = CARTESIAN_POINT ( 'NONE',  ( -9.400000000000007461, 2.500000000000000000, -0.2464101615137783419 ) ) ;
#127849 = CARTESIAN_POINT ( 'NONE',  ( 3.749999999999978684, 12.50000000000000000, -6.495190528383302464 ) ) ;
#127850 = DIRECTION ( 'NONE',  ( -0.000000000000000000, -1.000000000000000000, -0.000000000000000000 ) ) ;
#127851 = EDGE_CURVE ( 'NONE', #114403, #93012, #110737, .T. ) ;
#127852 = FACE_OUTER_BOUND ( 'NONE', #122107, .T. ) ;
#127853 = FACE_OUTER_BOUND ( 'NONE', #64178, .T. ) ;
#127854 = ORIENTED_EDGE ( 'NONE', *, *, #96867, .T. ) ;
#127855 = ORIENTED_EDGE ( 'NONE', *, *, #174, .T. ) ;
#127856 = ORIENTED_EDGE ( 'NONE', *, *, #53653, .T. ) ;
#127857 = ORIENTED_EDGE ( 'NONE', *, *, #47323, .T. ) ;
#127858 = CARTESIAN_POINT ( 'NONE',  ( -12.09999999999999432, 2.500000000000000000, 4.922947341949748257 ) ) ;
#127859 = FACE_OUTER_BOUND ( 'NONE', #114825, .T. ) ;
#127861 = ORIENTED_EDGE ( 'NONE', *, *, #108026, .F. ) ;
#127860 = ORIENTED_EDGE ( 'NONE', *, *, #33005, .T. ) ;
#127862 = ORIENTED_EDGE ( 'NONE', *, *, #87524, .F. ) ;
#127863 = LINE ( 'NONE', #6773, #119042 ) ;
#127864 = AXIS2_PLACEMENT_3D ( 'NONE', #122942, #65286, #114394 ) ;
#127865 = CIRCLE ( 'NONE', #56822, 0.06509327318403745899 ) ;
#127866 = CARTESIAN_POINT ( 'NONE',  ( -10.85000000000000142, 2.500000000000000000, -2.857883832488649745 ) ) ;
#127867 = DIRECTION ( 'NONE',  ( 0.000000000000000000, 0.000000000000000000, 1.000000000000000000 ) ) ;
#127868 = CARTESIAN_POINT ( 'NONE',  ( 11.64999999999990798, 2.500000000000000000, 7.188010851410848723 ) ) ;
#127869 = DIRECTION ( 'NONE',  ( -0.000000000000000000, 1.000000000000000000, -0.000000000000000000 ) ) ;
#127870 = DIRECTION ( 'NONE',  ( 0.000000000000000000, 0.000000000000000000, 1.000000000000000000 ) ) ;
#127871 = CARTESIAN_POINT ( 'NONE',  ( 108.0000000000000142, 8.500000000000000000, 0.000000000000000000 ) ) ;
#127872 = VERTEX_POINT ( 'NONE', #72121 ) ;
#127873 = AXIS2_PLACEMENT_3D ( 'NONE', #56925, #7192, #55011 ) ;
#127874 = FACE_OUTER_BOUND ( 'NONE', #20495, .T. ) ;
#127875 = ORIENTED_EDGE ( 'NONE', *, *, #74047, .T. ) ;
#127877 = ADVANCED_FACE ( 'NONE', ( #62306 ), #40744, .T. ) ;
#127876 = AXIS2_PLACEMENT_3D ( 'NONE', #122608, #23109, #1526 ) ;
#127878 = ORIENTED_EDGE ( 'NONE', *, *, #76474, .T. ) ;
#127879 = AXIS2_PLACEMENT_3D ( 'NONE', #39086, #98599, #76414 ) ;
#127880 = ORIENTED_EDGE ( 'NONE', *, *, #1382, .T. ) ;
#127881 = AXIS2_PLACEMENT_3D ( 'NONE', #80043, #81968, #121899 ) ;
#127882 = CARTESIAN_POINT ( 'NONE',  ( 10.64999999999990976, 12.50000000000000000, -6.841600689897077814 ) ) ;
#127883 = ORIENTED_EDGE ( 'NONE', *, *, #37139, .T. ) ;
#127884 = EDGE_CURVE ( 'NONE', #27857, #378, #82589, .T. ) ;
#127885 = ORIENTED_EDGE ( 'NONE', *, *, #61977, .F. ) ;
#127886 = EDGE_CURVE ( 'NONE', #13317, #408, #21066, .T. ) ;
#127887 = CIRCLE ( 'NONE', #52668, 0.1000000000000002554 ) ;
#127888 = CARTESIAN_POINT ( 'NONE',  ( 12.69999999999990337, 2.500000000000000000, 3.883716857408420431 ) ) ;
#127889 = DIRECTION ( 'NONE',  ( 0.000000000000000000, -0.9999939076577903929, 0.003490651415223739937 ) ) ;
#127890 = DIRECTION ( 'NONE',  ( 0.000000000000000000, 1.000000000000000000, 0.000000000000000000 ) ) ;
#127891 = DIRECTION ( 'NONE',  ( 0.000000000000000000, 0.000000000000000000, -1.000000000000000000 ) ) ;
#127892 = CIRCLE ( 'NONE', #69389, 0.1000000000000000472 ) ;
#127893 = VECTOR ( 'NONE', #100967, 1000.000000000000000 ) ;
#127894 = ADVANCED_FACE ( 'NONE', ( #61660 ), #78287, .T. ) ;
#127895 = EDGE_CURVE ( 'NONE', #114782, #127312, #12534, .T. ) ;
#127896 = CARTESIAN_POINT ( 'NONE',  ( -5.450000000000023270, 2.500000000000000000, -2.165063509461101710 ) ) ;
#127897 = EDGE_CURVE ( 'NONE', #52697, #11241, #76224, .T. ) ;
#127898 = AXIS2_PLACEMENT_3D ( 'NONE', #30441, #11415, #62474 ) ;
#127899 = ORIENTED_EDGE ( 'NONE', *, *, #66831, .F. ) ;
#127900 = DIRECTION ( 'NONE',  ( 0.000000000000000000, 1.000000000000000000, 0.000000000000000000 ) ) ;
#127901 = VERTEX_POINT ( 'NONE', #121205 ) ;
#127902 = PLANE ( 'NONE',  #90193 ) ;
#127903 = EDGE_CURVE ( 'NONE', #5697, #78167, #113871, .T. ) ;
#127904 = VERTEX_POINT ( 'NONE', #41381 ) ;
#127905 = FACE_OUTER_BOUND ( 'NONE', #38516, .T. ) ;
#127906 = VECTOR ( 'NONE', #62326, 1000.000000000000000 ) ;
#127907 = DIRECTION ( 'NONE',  ( 0.000000000000000000, 0.000000000000000000, 1.000000000000000000 ) ) ;
#127908 = ORIENTED_EDGE ( 'NONE', *, *, #12627, .T. ) ;
#127909 = DIRECTION ( 'NONE',  ( 0.000000000000000000, 0.000000000000000000, 1.000000000000000000 ) ) ;
#127910 = CARTESIAN_POINT ( 'NONE',  ( 13.14999999999989733, 12.50000000000000000, -2.511473670974877948 ) ) ;
#127911 = ORIENTED_EDGE ( 'NONE', *, *, #66211, .T. ) ;
#127912 = EDGE_CURVE ( 'NONE', #14309, #119361, #32331, .T. ) ;
#127913 = DIRECTION ( 'NONE',  ( 0.000000000000000000, 1.000000000000000000, 0.000000000000000000 ) ) ;
#127914 = ORIENTED_EDGE ( 'NONE', *, *, #81120, .F. ) ;
#127915 = VERTEX_POINT ( 'NONE', #42008 ) ;
#127916 = DIRECTION ( 'NONE',  ( -0.000000000000000000, 1.000000000000000000, -0.000000000000000000 ) ) ;
#127917 = DIRECTION ( 'NONE',  ( -1.000000000000000000, 0.000000000000000000, 0.000000000000000000 ) ) ;
#127918 = CARTESIAN_POINT ( 'NONE',  ( 184.2343750003414016, 8.734944146203032389, 5.348610694689227483E-16 ) ) ;
#127919 = LINE ( 'NONE', #89920, #124445 ) ;
#127920 = CARTESIAN_POINT ( 'NONE',  ( -7.950000000000012612, 12.50000000000000000, 2.165063509461097713 ) ) ;
#127921 = FACE_OUTER_BOUND ( 'NONE', #117783, .T. ) ;
#127922 = AXIS2_PLACEMENT_3D ( 'NONE', #52793, #103186, #52157 ) ;
#127923 = VECTOR ( 'NONE', #38432, 1000.000000000000000 ) ;
#127924 = AXIS2_PLACEMENT_3D ( 'NONE', #19048, #86513, #47260 ) ;
#127925 = VERTEX_POINT ( 'NONE', #3370 ) ;
#127926 = CARTESIAN_POINT ( 'NONE',  ( -0.8500000000000382805, 2.500000000000000000, -7.188010851410854052 ) ) ;
#127927 = DIRECTION ( 'NONE',  ( 0.000000000000000000, -0.9999939076577903929, 0.003490651415223739937 ) ) ;
#127928 = AXIS2_PLACEMENT_3D ( 'NONE', #74196, #123291, #64365 ) ;
#127929 = AXIS2_PLACEMENT_3D ( 'NONE', #85732, #85092, #64809 ) ;
#127930 = AXIS2_PLACEMENT_3D ( 'NONE', #2285, #100496, #40967 ) ;
#127931 = VERTEX_POINT ( 'NONE', #2716 ) ;
#127932 = VECTOR ( 'NONE', #6281, 1000.000000000000000 ) ;
#127933 = CONICAL_SURFACE ( 'NONE', #115379, 0.1000000000000000472, 0.003490658503988666988 ) ;
#127934 = DIRECTION ( 'NONE',  ( 0.000000000000000000, 0.000000000000000000, 1.000000000000000000 ) ) ;
#127935 = CARTESIAN_POINT ( 'NONE',  ( 1.649999999999949729, 2.500000000000000000, 7.088010851410848190 ) ) ;
#127936 = DIRECTION ( 'NONE',  ( -0.000000000000000000, -1.000000000000000000, -0.000000000000000000 ) ) ;
#127937 = CARTESIAN_POINT ( 'NONE',  ( -2.950000000000033484, 2.500000000000000000, -6.595190528383302109 ) ) ;
#127938 = DIRECTION ( 'NONE',  ( 0.000000000000000000, -0.9999939076577903929, 0.003490651415223739937 ) ) ;
#127939 = EDGE_LOOP ( 'NONE', ( #104243, #124043, #42541, #636 ) ) ;
#127940 = AXIS2_PLACEMENT_3D ( 'NONE', #8848, #98512, #129313 ) ;
#127941 = EDGE_CURVE ( 'NONE', #90263, #56748, #61560, .T. ) ;
#127942 = CARTESIAN_POINT ( 'NONE',  ( 0.7999999999999548583, 12.50000000000000000, 4.265033745738159077 ) ) ;
#127943 = CARTESIAN_POINT ( 'NONE',  ( -3.350000000000028955, 2.500000000000000000, 2.065063509461097624 ) ) ;
#127944 = VERTEX_POINT ( 'NONE', #11894 ) ;
#127945 = CARTESIAN_POINT ( 'NONE',  ( -6.050000000000020250, 2.500000000000000000, -2.511473670974877948 ) ) ;
#127946 = EDGE_CURVE ( 'NONE', #113860, #47295, #101252, .T. ) ;
#127947 = VERTEX_POINT ( 'NONE', #91750 ) ;
#127948 = VERTEX_POINT ( 'NONE', #92385 ) ;
#127949 = CARTESIAN_POINT ( 'NONE',  ( 8.299999999999922551, 2.500000000000000000, -4.330127018922201643 ) ) ;
#127950 = VERTEX_POINT ( 'NONE', #81920 ) ;
#127951 = FACE_OUTER_BOUND ( 'NONE', #24376, .T. ) ;
#127952 = DIRECTION ( 'NONE',  ( -4.274815082592931898E-19, -0.9999939076577903929, -0.003490651415223739937 ) ) ;
#127953 = FACE_OUTER_BOUND ( 'NONE', #8053, .T. ) ;
#127954 = AXIS2_PLACEMENT_3D ( 'NONE', #19407, #59378, #99282 ) ;
#127955 = VERTEX_POINT ( 'NONE', #110102 ) ;
#127956 = LINE ( 'NONE', #8173, #111530 ) ;
#127958 = VERTEX_POINT ( 'NONE', #112689 ) ;
#127957 = DIRECTION ( 'NONE',  ( 0.000000000000000000, 1.000000000000000000, 0.000000000000000000 ) ) ;
#127959 = CARTESIAN_POINT ( 'NONE',  ( 1.649999999999951505, 12.50000000000000000, -2.792790559304616504 ) ) ;
#127960 = DIRECTION ( 'NONE',  ( 0.000000000000000000, 0.000000000000000000, -1.000000000000000000 ) ) ;
#127961 = ORIENTED_EDGE ( 'NONE', *, *, #49500, .F. ) ;
#127962 = CONICAL_SURFACE ( 'NONE', #71421, 0.1000000000000000472, 0.003490658503988666988 ) ;
#127963 = VECTOR ( 'NONE', #127755, 1000.000000000000000 ) ;
#127964 = VECTOR ( 'NONE', #42960, 1000.000000000000000 ) ;
#127965 = EDGE_LOOP ( 'NONE', ( #39448, #54473 ) ) ;
#127966 = ORIENTED_EDGE ( 'NONE', *, *, #88403, .F. ) ;
#127967 = DIRECTION ( 'NONE',  ( 0.000000000000000000, 0.000000000000000000, -1.000000000000000000 ) ) ;
#127968 = CARTESIAN_POINT ( 'NONE',  ( -11.64999999999999680, 2.500000000000000000, -7.288010851410851032 ) ) ;
#127969 = PLANE ( 'NONE',  #42232 ) ;
#127970 = FACE_BOUND ( 'NONE', #129335, .T. ) ;
#127971 = VERTEX_POINT ( 'NONE', #23016 ) ;
#127972 = CARTESIAN_POINT ( 'NONE',  ( -5.800000000000018474, 2.500000000000000000, -2.276824562219559311E-15 ) ) ;
#127973 = FACE_OUTER_BOUND ( 'NONE', #76048, .T. ) ;
#127974 = AXIS2_PLACEMENT_3D ( 'NONE', #31070, #53108, #61151 ) ;
#127975 = ORIENTED_EDGE ( 'NONE', *, *, #116766, .F. ) ;
#127976 = AXIS2_PLACEMENT_3D ( 'NONE', #109465, #59747, #49924 ) ;
#127978 = EDGE_CURVE ( 'NONE', #41506, #35443, #53124, .T. ) ;
#127977 = CARTESIAN_POINT ( 'NONE',  ( 5.449999999999936229, 2.500000000000000000, -2.165063509461101710 ) ) ;
#127979 = CARTESIAN_POINT ( 'NONE',  ( -8.350000000000012079, 2.500000000000000000, -1.372243186433550033 ) ) ;
#127980 = AXIS2_PLACEMENT_3D ( 'NONE', #6096, #127195, #125247 ) ;
#127981 = AXIS2_PLACEMENT_3D ( 'NONE', #68810, #108725, #19042 ) ;
#127982 = AXIS2_PLACEMENT_3D ( 'NONE', #76021, #56374, #46549 ) ;
#127983 = DIRECTION ( 'NONE',  ( 0.000000000000000000, -0.9999939076577903929, 0.003490651415223739937 ) ) ;
#127984 = DIRECTION ( 'NONE',  ( 0.000000000000000000, 1.000000000000000000, 0.000000000000000000 ) ) ;
#127985 = CARTESIAN_POINT ( 'NONE',  ( 2.099999999999948574, 12.50000000000000000, 4.395220292106234439 ) ) ;
#127986 = CARTESIAN_POINT ( 'NONE',  ( -12.69999999999999396, 2.500000000000000000, -4.083716857408424161 ) ) ;
#127987 = CARTESIAN_POINT ( 'NONE',  ( -4.400000000000025224, 2.500000000000000000, 4.776537180435972196 ) ) ;
#127988 = EDGE_CURVE ( 'NONE', #97598, #118985, #72023, .T. ) ;
#127989 = ORIENTED_EDGE ( 'NONE', *, *, #69173, .T. ) ;
#127990 = EDGE_LOOP ( 'NONE', ( #34995, #26824 ) ) ;
#127991 = ORIENTED_EDGE ( 'NONE', *, *, #43113, .F. ) ;
#127992 = VERTEX_POINT ( 'NONE', #100288 ) ;
#127993 = EDGE_LOOP ( 'NONE', ( #103131, #129026 ) ) ;
#127994 = CARTESIAN_POINT ( 'NONE',  ( -12.69999999999999041, 12.50000000000000000, 3.918623584224383727 ) ) ;
#127995 = EDGE_CURVE ( 'NONE', #52320, #108189, #19783, .T. ) ;
#127996 = DIRECTION ( 'NONE',  ( -4.274815082592931898E-19, -0.9999939076577903929, -0.003490651415223739937 ) ) ;
#127997 = ORIENTED_EDGE ( 'NONE', *, *, #48023, .F. ) ;
#127998 = FACE_BOUND ( 'NONE', #40435, .T. ) ;
#127999 = EDGE_CURVE ( 'NONE', #95824, #72203, #56027, .T. ) ;
#128000 = CARTESIAN_POINT ( 'NONE',  ( 6.849999999999929479, 2.500000000000000000, 6.148780366869520009 ) ) ;
#128001 = EDGE_CURVE ( 'NONE', #70303, #125468, #105461, .T. ) ;
#128002 = FACE_OUTER_BOUND ( 'NONE', #60070, .T. ) ;
#128003 = DIRECTION ( 'NONE',  ( 0.000000000000000000, 1.000000000000000000, 0.000000000000000000 ) ) ;
#128004 = DIRECTION ( 'NONE',  ( 0.000000000000000000, 0.000000000000000000, 1.000000000000000000 ) ) ;
#128005 = EDGE_CURVE ( 'NONE', #121848, #16531, #57434, .T. ) ;
#128006 = DIRECTION ( 'NONE',  ( 0.000000000000000000, 1.000000000000000000, 0.000000000000000000 ) ) ;
#128007 = EDGE_LOOP ( 'NONE', ( #28148, #73185, #102362, #120785 ) ) ;
#128008 = CARTESIAN_POINT ( 'NONE',  ( 7.499999999999925393, 2.500000000000000000, -0.6928203230275541413 ) ) ;
#128009 = ORIENTED_EDGE ( 'NONE', *, *, #26286, .F. ) ;
#128010 = EDGE_LOOP ( 'NONE', ( #31250, #41080 ) ) ;
#128011 = AXIS2_PLACEMENT_3D ( 'NONE', #110425, #91432, #40422 ) ;
#128012 = EDGE_LOOP ( 'NONE', ( #109612, #95312 ) ) ;
#128013 = CONICAL_SURFACE ( 'NONE', #73623, 0.1000000000000002554, 0.003490658503988666988 ) ;
#128014 = DIRECTION ( 'NONE',  ( 0.000000000000000000, 0.000000000000000000, 1.000000000000000000 ) ) ;
#128015 = CIRCLE ( 'NONE', #84179, 0.09999999999999982514 ) ;
#128016 = CARTESIAN_POINT ( 'NONE',  ( 14.69113575804733429, 2.499999999999999112, 6.337000356224947950 ) ) ;
#128017 = CARTESIAN_POINT ( 'NONE',  ( 11.89999999999990798, 2.500000000000000000, -3.983716857408426293 ) ) ;
#128018 = VERTEX_POINT ( 'NONE', #84198 ) ;
#128019 = DIRECTION ( 'NONE',  ( -0.000000000000000000, -1.000000000000000000, -0.000000000000000000 ) ) ;
#128020 = CARTESIAN_POINT ( 'NONE',  ( 2.499999999999981792, 12.50000000000000000, 4.395220292106234439 ) ) ;
#128021 = AXIS2_PLACEMENT_3D ( 'NONE', #55618, #106013, #66073 ) ;
#128022 = AXIS2_PLACEMENT_3D ( 'NONE', #51633, #41823, #12960 ) ;
#128023 = CIRCLE ( 'NONE', #44397, 0.1000000000000000472 ) ;
#128024 = DIRECTION ( 'NONE',  ( 0.000000000000000000, 0.000000000000000000, 1.000000000000000000 ) ) ;
#128025 = CARTESIAN_POINT ( 'NONE',  ( 185.9010416670080303, -4.367472073101519747, 7.564683531249999149 ) ) ;
#128026 = CARTESIAN_POINT ( 'NONE',  ( -6.249999999999984901, 2.500000000000000000, -6.395190528383301931 ) ) ;
#128027 = FACE_OUTER_BOUND ( 'NONE', #24887, .T. ) ;
#128028 = VECTOR ( 'NONE', #40800, 1000.000000000000000 ) ;
#128029 = CONICAL_SURFACE ( 'NONE', #71589, 0.1000000000000002554, 0.003490658503988666988 ) ;
#128030 = CARTESIAN_POINT ( 'NONE',  ( -5.650000000000023448, 12.50000000000000000, -6.148780366869526226 ) ) ;
#128031 = VERTEX_POINT ( 'NONE', #96586 ) ;
#128032 = LINE ( 'NONE', #129349, #113257 ) ;
#128033 = CIRCLE ( 'NONE', #67355, 0.06509327318403745899 ) ;
#128034 = VERTEX_POINT ( 'NONE', #124129 ) ;
#128035 = EDGE_CURVE ( 'NONE', #26403, #69417, #6908, .T. ) ;
#128036 = ORIENTED_EDGE ( 'NONE', *, *, #16426, .T. ) ;
#128037 = CARTESIAN_POINT ( 'NONE',  ( -11.44999999999999751, 2.500000000000000000, 6.841600689897072485 ) ) ;
#128038 = LINE ( 'NONE', #27903, #107327 ) ;
#128039 = CARTESIAN_POINT ( 'NONE',  ( 13.74999999999989697, 2.500000000000000000, 2.857883832488649301 ) ) ;
#128040 = EDGE_LOOP ( 'NONE', ( #7137, #36840 ) ) ;
#128042 = ADVANCED_FACE ( 'NONE', ( #34485 ), #115913, .T. ) ;
#128041 = VERTEX_POINT ( 'NONE', #66493 ) ;
#128043 = AXIS2_PLACEMENT_3D ( 'NONE', #97355, #48255, #67213 ) ;
#128044 = DIRECTION ( 'NONE',  ( 0.000000000000000000, -0.9999939076577903929, 0.003490651415223739937 ) ) ;
#128045 = CARTESIAN_POINT ( 'NONE',  ( 3.749999999999938716, 12.50000000000000000, 7.188010851410848723 ) ) ;
#128046 = DIRECTION ( 'NONE',  ( 0.000000000000000000, 1.000000000000000000, 0.000000000000000000 ) ) ;
#128047 = ORIENTED_EDGE ( 'NONE', *, *, #20125, .F. ) ;
#128048 = ORIENTED_EDGE ( 'NONE', *, *, #100581, .F. ) ;
#128049 = EDGE_CURVE ( 'NONE', #31868, #31765, #105129, .T. ) ;
#128050 = CARTESIAN_POINT ( 'NONE',  ( -13.09999999999999254, 2.500000000000000000, -3.983716857408423628 ) ) ;
#128051 = EDGE_CURVE ( 'NONE', #20148, #24253, #124784, .T. ) ;
#128052 = EDGE_CURVE ( 'NONE', #70878, #99834, #28099, .T. ) ;
#128054 = EDGE_LOOP ( 'NONE', ( #81280, #56323 ) ) ;
#128053 = CONICAL_SURFACE ( 'NONE', #84122, 0.09999999999999982514, 0.003490658503988666988 ) ;
#128055 = DIRECTION ( 'NONE',  ( 0.000000000000000000, 0.000000000000000000, 1.000000000000000000 ) ) ;
#128056 = AXIS2_PLACEMENT_3D ( 'NONE', #21096, #13199, #32879 ) ;
#128057 = DIRECTION ( 'NONE',  ( 0.000000000000000000, 1.000000000000000000, 0.000000000000000000 ) ) ;
#128058 = EDGE_LOOP ( 'NONE', ( #109172, #41879, #7317, #104479 ) ) ;
#128059 = CARTESIAN_POINT ( 'NONE',  ( -8.950000000000004619, 12.50000000000000000, 6.213873640053559022 ) ) ;
#128060 = EDGE_CURVE ( 'NONE', #2830, #57084, #69963, .T. ) ;
#128061 = DIRECTION ( 'NONE',  ( 0.000000000000000000, -0.000000000000000000, 1.000000000000000000 ) ) ;
#128062 = FACE_OUTER_BOUND ( 'NONE', #12714, .T. ) ;
#128064 = CIRCLE ( 'NONE', #40231, 0.06509327318403743123 ) ;
#128063 = DIRECTION ( 'NONE',  ( 0.000000000000000000, 0.000000000000000000, 1.000000000000000000 ) ) ;
#128065 = EDGE_LOOP ( 'NONE', ( #94223, #36540, #40953, #70013 ) ) ;
#128066 = VECTOR ( 'NONE', #36939, 1000.000000000000000 ) ;
#128067 = EDGE_CURVE ( 'NONE', #13197, #59055, #80431, .T. ) ;
#128068 = CIRCLE ( 'NONE', #107115, 0.1000000000000002554 ) ;
#128069 = CARTESIAN_POINT ( 'NONE',  ( -3.350000000000028511, 2.500000000000000000, -2.857883832488653741 ) ) ;
#128070 = ADVANCED_FACE ( 'NONE', ( #44938 ), #15554, .T. ) ;
#128071 = CONICAL_SURFACE ( 'NONE', #19380, 0.1000000000000002554, 0.003490658503988666988 ) ;
#128072 = ORIENTED_EDGE ( 'NONE', *, *, #116653, .F. ) ;
#128073 = VERTEX_POINT ( 'NONE', #86777 ) ;
#128074 = DIRECTION ( 'NONE',  ( 0.000000000000000000, -0.9999939076577903929, 0.003490651415223739937 ) ) ;
#128075 = PLANE ( 'NONE',  #84659 ) ;
#128076 = LINE ( 'NONE', #17451, #90749 ) ;
#128077 = DIRECTION ( 'NONE',  ( 0.000000000000000000, 0.000000000000000000, 1.000000000000000000 ) ) ;
#128078 = DIRECTION ( 'NONE',  ( 0.000000000000000000, -0.9999939076577903929, 0.003490651415223739937 ) ) ;
#128079 = DIRECTION ( 'NONE',  ( 0.000000000000000000, 1.000000000000000000, 0.000000000000000000 ) ) ;
#128080 = AXIS2_PLACEMENT_3D ( 'NONE', #19651, #119135, #89675 ) ;
#128081 = CARTESIAN_POINT ( 'NONE',  ( 6.849999999999929479, 2.500000000000000000, -1.918653347947326004 ) ) ;
#128082 = AXIS2_PLACEMENT_3D ( 'NONE', #86336, #47088, #114511 ) ;
#128083 = FACE_OUTER_BOUND ( 'NONE', #38739, .T. ) ;
#128084 = AXIS2_PLACEMENT_3D ( 'NONE', #82183, #13426, #101825 ) ;
#128085 = AXIS2_PLACEMENT_3D ( 'NONE', #24196, #66041, #14351 ) ;
#128086 = DIRECTION ( 'NONE',  ( 0.000000000000000000, 0.000000000000000000, 1.000000000000000000 ) ) ;
#128087 = CONICAL_SURFACE ( 'NONE', #88345, 0.1000000000000002554, 0.003490658503988666988 ) ;
#128088 = FACE_OUTER_BOUND ( 'NONE', #70209, .T. ) ;
#128089 = CIRCLE ( 'NONE', #31955, 0.1000000000000002554 ) ;
#128090 = ORIENTED_EDGE ( 'NONE', *, *, #120257, .T. ) ;
#128091 = DIRECTION ( 'NONE',  ( 0.000000000000000000, 0.000000000000000000, 1.000000000000000000 ) ) ;
#128092 = DIRECTION ( 'NONE',  ( 0.000000000000000000, 1.000000000000000000, 0.000000000000000000 ) ) ;
#128093 = DIRECTION ( 'NONE',  ( 0.000000000000000000, 0.000000000000000000, 1.000000000000000000 ) ) ;
#128094 = DIRECTION ( 'NONE',  ( 0.000000000000000000, 0.000000000000000000, 1.000000000000000000 ) ) ;
#128095 = DIRECTION ( 'NONE',  ( -0.000000000000000000, 1.000000000000000000, -0.000000000000000000 ) ) ;
#128096 = VERTEX_POINT ( 'NONE', #16090 ) ;
#128097 = DIRECTION ( 'NONE',  ( -0.000000000000000000, 1.000000000000000000, -0.000000000000000000 ) ) ;
#128098 = CARTESIAN_POINT ( 'NONE',  ( 185.3333333333333144, 6.668395609140177704, -3.849999999999998312 ) ) ;
#128100 = ORIENTED_EDGE ( 'NONE', *, *, #83305, .T. ) ;
#128099 = DIRECTION ( 'NONE',  ( 0.000000000000000000, 1.000000000000000000, 0.000000000000000000 ) ) ;
#128101 = AXIS2_PLACEMENT_3D ( 'NONE', #110027, #9884, #119194 ) ;
#128102 = CIRCLE ( 'NONE', #86313, 0.06509327318403745899 ) ;
#128103 = VERTEX_POINT ( 'NONE', #37060 ) ;
#128104 = DIRECTION ( 'NONE',  ( 0.000000000000000000, -0.000000000000000000, 1.000000000000000000 ) ) ;
#128105 = EDGE_CURVE ( 'NONE', #16630, #109444, #109669, .T. ) ;
#128106 = ORIENTED_EDGE ( 'NONE', *, *, #35914, .T. ) ;
#128107 = ORIENTED_EDGE ( 'NONE', *, *, #106153, .F. ) ;
#128108 = AXIS2_PLACEMENT_3D ( 'NONE', #56005, #66474, #96569 ) ;
#128109 = ORIENTED_EDGE ( 'NONE', *, *, #125363, .F. ) ;
#128110 = DIRECTION ( 'NONE',  ( 0.000000000000000000, 1.000000000000000000, 0.000000000000000000 ) ) ;
#128111 = AXIS2_PLACEMENT_3D ( 'NONE', #34719, #74617, #114527 ) ;
#128112 = CARTESIAN_POINT ( 'NONE',  ( -12.89999999999999325, 12.50000000000000000, 0.6928203230275535862 ) ) ;
#128113 = CARTESIAN_POINT ( 'NONE',  ( -10.65000000000000391, 2.500000000000000000, -6.148780366869522673 ) ) ;
#128114 = CARTESIAN_POINT ( 'NONE',  ( 12.09999999999990195, 2.500000000000000000, 0.7928203230275495672 ) ) ;
#128116 = ORIENTED_EDGE ( 'NONE', *, *, #108057, .F. ) ;
#128115 = AXIS2_PLACEMENT_3D ( 'NONE', #30881, #70781, #91068 ) ;
#128117 = CONICAL_SURFACE ( 'NONE', #115567, 0.1000000000000000472, 0.003490658503988666988 ) ;
#128118 = AXIS2_PLACEMENT_3D ( 'NONE', #18612, #250, #118744 ) ;
#128119 = CARTESIAN_POINT ( 'NONE',  ( -8.950000000000008171, 12.50000000000000000, -2.511473670974877948 ) ) ;
#128121 = ORIENTED_EDGE ( 'NONE', *, *, #122697, .F. ) ;
#128120 = CIRCLE ( 'NONE', #98769, 3.000000000000000444 ) ;
#128122 = DIRECTION ( 'NONE',  ( 0.000000000000000000, 0.000000000000000000, 1.000000000000000000 ) ) ;
#128123 = DIRECTION ( 'NONE',  ( 0.000000000000000000, 0.000000000000000000, 1.000000000000000000 ) ) ;
#128124 = AXIS2_PLACEMENT_3D ( 'NONE', #3130, #71214, #21475 ) ;
#128125 = CARTESIAN_POINT ( 'NONE',  ( 15.05551045036142277, 2.483581587658090228, 4.666934263335511091 ) ) ;
#128126 = DIRECTION ( 'NONE',  ( 0.000000000000000000, -0.9999939076577903929, 0.003490651415223739937 ) ) ;
#128127 = CARTESIAN_POINT ( 'NONE',  ( 4.149999999999941735, 12.50000000000000000, -2.792790559304616504 ) ) ;
#128128 = CONICAL_SURFACE ( 'NONE', #52812, 0.09999999999999999167, 0.003490658503988666988 ) ;
#128129 = ORIENTED_EDGE ( 'NONE', *, *, #56798, .F. ) ;
#128130 = ORIENTED_EDGE ( 'NONE', *, *, #114965, .F. ) ;
#128131 = EDGE_LOOP ( 'NONE', ( #18180, #127767 ) ) ;
#128132 = ORIENTED_EDGE ( 'NONE', *, *, #75766, .T. ) ;
#128133 = ORIENTED_EDGE ( 'NONE', *, *, #69952, .T. ) ;
#128134 = DIRECTION ( 'NONE',  ( 0.000000000000000000, 1.000000000000000000, 0.000000000000000000 ) ) ;
#128135 = CARTESIAN_POINT ( 'NONE',  ( 43.31340625566036096, 2.029328411521368558, 5.113049425667499648 ) ) ;
#128136 = CARTESIAN_POINT ( 'NONE',  ( 10.39999999999991154, 2.500000000000000000, -3.637306695894650055 ) ) ;
#128137 = FACE_BOUND ( 'NONE', #32755, .T. ) ;
#128138 = FACE_OUTER_BOUND ( 'NONE', #101500, .T. ) ;
#128139 = CARTESIAN_POINT ( 'NONE',  ( -5.850000000000018296, 2.500000000000000000, 1.572243186433545548 ) ) ;
#128140 = FACE_OUTER_BOUND ( 'NONE', #107089, .T. ) ;
#128141 = DIRECTION ( 'NONE',  ( 0.000000000000000000, -0.9999939076577903929, 0.003490651415223739937 ) ) ;
#128142 = AXIS2_PLACEMENT_3D ( 'NONE', #30424, #80803, #110248 ) ;
#128143 = DIRECTION ( 'NONE',  ( -4.274815082592931898E-19, -0.9999939076577903929, -0.003490651415223739937 ) ) ;
#128144 = DIRECTION ( 'NONE',  ( 1.000000000000000000, 0.000000000000000000, 0.000000000000000000 ) ) ;
#128145 = CARTESIAN_POINT ( 'NONE',  ( 115.5000000000000000, 0.000000000000000000, -2.000000000000000000 ) ) ;
#128146 = CIRCLE ( 'NONE', #21534, 0.06509327318403745899 ) ;
#128147 = CIRCLE ( 'NONE', #23783, 0.06509327318403745899 ) ;
#128148 = EDGE_CURVE ( 'NONE', #38872, #116591, #67797, .T. ) ;
#128149 = DIRECTION ( 'NONE',  ( 0.000000000000000000, 1.000000000000000000, 0.000000000000000000 ) ) ;
#128150 = VERTEX_POINT ( 'NONE', #126719 ) ;
#128151 = ORIENTED_EDGE ( 'NONE', *, *, #15615, .T. ) ;
#128152 = ORIENTED_EDGE ( 'NONE', *, *, #94490, .F. ) ;
#128153 = ORIENTED_EDGE ( 'NONE', *, *, #70791, .F. ) ;
#128154 = ADVANCED_FACE ( 'NONE', ( #4988 ), #34463, .T. ) ;
#128155 = LINE ( 'NONE', #129472, #123955 ) ;
#128156 = FACE_BOUND ( 'NONE', #59823, .T. ) ;
#128157 = CIRCLE ( 'NONE', #40339, 0.06509327318403745899 ) ;
#128158 = EDGE_CURVE ( 'NONE', #68530, #73774, #25267, .T. ) ;
#128159 = AXIS2_PLACEMENT_3D ( 'NONE', #119676, #109875, #38576 ) ;
#128160 = DIRECTION ( 'NONE',  ( 0.000000000000000000, 1.000000000000000000, 0.000000000000000000 ) ) ;
#128161 = AXIS2_PLACEMENT_3D ( 'NONE', #109339, #90990, #9858 ) ;
#128162 = VECTOR ( 'NONE', #8619, 1000.000000000000000 ) ;
#128163 = EDGE_CURVE ( 'NONE', #73692, #14356, #34376, .T. ) ;
#128164 = ADVANCED_FACE ( 'NONE', ( #17380 ), #59522, .T. ) ;
#128165 = ORIENTED_EDGE ( 'NONE', *, *, #3193, .F. ) ;
#128166 = FACE_OUTER_BOUND ( 'NONE', #91629, .T. ) ;
#128167 = LINE ( 'NONE', #28678, #1333 ) ;
#128168 = FACE_OUTER_BOUND ( 'NONE', #48367, .T. ) ;
#128169 = EDGE_CURVE ( 'NONE', #83800, #8589, #74166, .T. ) ;
#128170 = DIRECTION ( 'NONE',  ( 0.000000000000000000, 1.000000000000000000, 0.000000000000000000 ) ) ;
#128171 = ORIENTED_EDGE ( 'NONE', *, *, #26649, .F. ) ;
#128172 = DIRECTION ( 'NONE',  ( 0.000000000000000000, -0.9999939076577903929, 0.003490651415223739937 ) ) ;
#128173 = LINE ( 'NONE', #109149, #120213 ) ;
#128174 = AXIS2_PLACEMENT_3D ( 'NONE', #47736, #66066, #106004 ) ;
#128175 = CONICAL_SURFACE ( 'NONE', #71741, 0.1000000000000002554, 0.003490658503988666988 ) ;
#128176 = VERTEX_POINT ( 'NONE', #10168 ) ;
#128177 = ORIENTED_EDGE ( 'NONE', *, *, #65966, .T. ) ;
#128178 = FACE_OUTER_BOUND ( 'NONE', #72223, .T. ) ;
#128179 = DIRECTION ( 'NONE',  ( -4.274815082592931898E-19, -0.9999939076577903929, -0.003490651415223739937 ) ) ;
#128180 = AXIS2_PLACEMENT_3D ( 'NONE', #81619, #51537, #82282 ) ;
#128181 = ORIENTED_EDGE ( 'NONE', *, *, #30254, .F. ) ;
#128182 = DIRECTION ( 'NONE',  ( -4.274815082592931898E-19, -0.9999939076577903929, -0.003490651415223739937 ) ) ;
#128183 = VECTOR ( 'NONE', #34179, 1000.000000000000000 ) ;
#128184 = LINE ( 'NONE', #45756, #83255 ) ;
#128185 = ORIENTED_EDGE ( 'NONE', *, *, #56487, .T. ) ;
#128186 = CARTESIAN_POINT ( 'NONE',  ( -9.350000000000004974, 12.50000000000000000, 6.213873640053559022 ) ) ;
#128187 = ORIENTED_EDGE ( 'NONE', *, *, #10966, .T. ) ;
#128188 = DIRECTION ( 'NONE',  ( -0.000000000000000000, 1.000000000000000000, -0.000000000000000000 ) ) ;
#128189 = ORIENTED_EDGE ( 'NONE', *, *, #115763, .F. ) ;
#128190 = DIRECTION ( 'NONE',  ( 0.000000000000000000, -0.000000000000000000, 1.000000000000000000 ) ) ;
#128191 = FACE_BOUND ( 'NONE', #60284, .T. ) ;
#128192 = VERTEX_POINT ( 'NONE', #87422 ) ;
#128193 = CARTESIAN_POINT ( 'NONE',  ( 109.6525664375320304, 6.077905868614581486, 4.730106526360415842 ) ) ;
#128194 = ORIENTED_EDGE ( 'NONE', *, *, #66576, .T. ) ;
#128195 = DIRECTION ( 'NONE',  ( 0.000000000000000000, 0.000000000000000000, -1.000000000000000000 ) ) ;
#128196 = DIRECTION ( 'NONE',  ( -4.274815082592931898E-19, -0.9999939076577903929, -0.003490651415223739937 ) ) ;
#128197 = DIRECTION ( 'NONE',  ( 0.000000000000000000, 1.000000000000000000, 0.000000000000000000 ) ) ;
#128199 = EDGE_CURVE ( 'NONE', #109355, #25435, #86671, .T. ) ;
#128198 = CIRCLE ( 'NONE', #96875, 0.1000000000000002554 ) ;
#128200 = DIRECTION ( 'NONE',  ( 0.000000000000000000, 0.000000000000000000, -1.000000000000000000 ) ) ;
#128201 = CARTESIAN_POINT ( 'NONE',  ( 17.50000000000000711, 2.499999999999961808, -3.093175630837484924 ) ) ;
#128202 = ORIENTED_EDGE ( 'NONE', *, *, #68787, .F. ) ;
#128203 = EDGE_LOOP ( 'NONE', ( #31454, #84225 ) ) ;
#128204 = ORIENTED_EDGE ( 'NONE', *, *, #994, .T. ) ;
#128205 = CARTESIAN_POINT ( 'NONE',  ( 10.59999999999990905, 2.500000000000000000, 3.983716857408420076 ) ) ;
#128206 = VECTOR ( 'NONE', #22680, 1000.000000000000000 ) ;
#128207 = VECTOR ( 'NONE', #118480, 1000.000000000000000 ) ;
#128208 = CARTESIAN_POINT ( 'NONE',  ( -11.89999999999999503, 2.500000000000000000, 4.083716857408420609 ) ) ;
#128209 = CIRCLE ( 'NONE', #61308, 0.1000000000000002554 ) ;
#128212 = ADVANCED_FACE ( 'NONE', ( #80203 ), #46978, .T. ) ;
#128211 = CARTESIAN_POINT ( 'NONE',  ( 5.199999999999933564, 12.50000000000000000, 4.048810130592458201 ) ) ;
#128210 = AXIS2_PLACEMENT_3D ( 'NONE', #66406, #27139, #57901 ) ;
#128214 = ORIENTED_EDGE ( 'NONE', *, *, #21014, .F. ) ;
#128213 = ORIENTED_EDGE ( 'NONE', *, *, #66472, .F. ) ;
#128215 = VERTEX_POINT ( 'NONE', #39013 ) ;
#128216 = EDGE_CURVE ( 'NONE', #45538, #94583, #103408, .T. ) ;
#128217 = DIRECTION ( 'NONE',  ( 0.000000000000000000, 0.000000000000000000, 1.000000000000000000 ) ) ;
#128218 = ADVANCED_FACE ( 'NONE', ( #78279 ), #120122, .T. ) ;
#128219 = FACE_OUTER_BOUND ( 'NONE', #108857, .T. ) ;
#128220 = CIRCLE ( 'NONE', #86425, 0.09999999999999982514 ) ;
#128221 = AXIS2_PLACEMENT_3D ( 'NONE', #90514, #100353, #100985 ) ;
#128222 = AXIS2_PLACEMENT_3D ( 'NONE', #112803, #42126, #1541 ) ;
#128223 = CARTESIAN_POINT ( 'NONE',  ( -12.49999999999995914, 12.50000000000000000, -0.06509327318403558549 ) ) ;
#128224 = DIRECTION ( 'NONE',  ( -0.000000000000000000, -1.000000000000000000, -0.000000000000000000 ) ) ;
#128225 = CARTESIAN_POINT ( 'NONE',  ( -1.050000000000038236, 2.500000000000000000, -1.818653347947326138 ) ) ;
#128226 = CARTESIAN_POINT ( 'NONE',  ( 6.649999999999930189, 2.500000000000000000, -2.857883832488653741 ) ) ;
#128227 = DIRECTION ( 'NONE',  ( -0.000000000000000000, -1.000000000000000000, -0.000000000000000000 ) ) ;
#128228 = EDGE_CURVE ( 'NONE', #11179, #16737, #118064, .T. ) ;
#128229 = CONICAL_SURFACE ( 'NONE', #92707, 0.09999999999999982514, 0.003490658503988666988 ) ;
#128230 = EDGE_CURVE ( 'NONE', #71603, #46014, #78924, .T. ) ;
#128231 = DIRECTION ( 'NONE',  ( -4.274815082592931898E-19, -0.9999939076577903929, -0.003490651415223739937 ) ) ;
#128232 = AXIS2_PLACEMENT_3D ( 'NONE', #71392, #30222, #99596 ) ;
#128233 = ADVANCED_FACE ( 'NONE', ( #37697 ), #9414, .T. ) ;
#128234 = ORIENTED_EDGE ( 'NONE', *, *, #18824, .F. ) ;
#128236 = ORIENTED_EDGE ( 'NONE', *, *, #599, .F. ) ;
#128235 = ADVANCED_FACE ( 'NONE', ( #50109 ), #109758, .T. ) ;
#128237 = FACE_OUTER_BOUND ( 'NONE', #19215, .T. ) ;
#128238 = ADVANCED_FACE ( 'NONE', ( #128002 ), #57984, .T. ) ;
#128239 = DIRECTION ( 'NONE',  ( 0.000000000000000000, 1.000000000000000000, 0.000000000000000000 ) ) ;
#128240 = ORIENTED_EDGE ( 'NONE', *, *, #60971, .T. ) ;
#128241 = VERTEX_POINT ( 'NONE', #8219 ) ;
#128242 = CARTESIAN_POINT ( 'NONE',  ( 185.8593750003413732, 0.000000000000000000, 7.564683531250000925 ) ) ;
#128243 = DIRECTION ( 'NONE',  ( 0.000000000000000000, -0.9999939076577903929, 0.003490651415223739937 ) ) ;
#128244 = DIRECTION ( 'NONE',  ( 0.000000000000000000, -0.000000000000000000, 1.000000000000000000 ) ) ;
#128245 = EDGE_CURVE ( 'NONE', #74234, #116433, #82579, .T. ) ;
#128246 = AXIS2_PLACEMENT_3D ( 'NONE', #17163, #97688, #45388 ) ;
#128247 = CARTESIAN_POINT ( 'NONE',  ( -0.8500000000000395017, 2.500000000000000000, 6.395190528383296602 ) ) ;
#128248 = CARTESIAN_POINT ( 'NONE',  ( 1.649999999999948841, 2.500000000000000000, 6.495190528383297135 ) ) ;
#128249 = CARTESIAN_POINT ( 'NONE',  ( 8.099999999999921485, 12.50000000000000000, 0.3464101615137735735 ) ) ;
#128250 = FACE_OUTER_BOUND ( 'NONE', #77338, .T. ) ;
#128251 = CIRCLE ( 'NONE', #46668, 0.06509327318403745899 ) ;
#128253 = CIRCLE ( 'NONE', #19468, 0.06509327318403741736 ) ;
#128252 = FACE_OUTER_BOUND ( 'NONE', #31918, .T. ) ;
#128254 = UNCERTAINTY_MEASURE_WITH_UNIT (LENGTH_MEASURE( 1.000000000000000082E-05 ), #21635, 'distance_accuracy_value', 'NONE');
#128255 = ORIENTED_EDGE ( 'NONE', *, *, #127310, .F. ) ;
#128256 = EDGE_LOOP ( 'NONE', ( #128940, #102384 ) ) ;
#128257 = VERTEX_POINT ( 'NONE', #88722 ) ;
#128258 = ADVANCED_FACE ( 'NONE', ( #109657 ), #78375, .T. ) ;
#128259 = ORIENTED_EDGE ( 'NONE', *, *, #116089, .T. ) ;
#128260 = CONICAL_SURFACE ( 'NONE', #29963, 0.1000000000000000472, 0.003490658503988666988 ) ;
#128261 = CARTESIAN_POINT ( 'NONE',  ( 11.64999999999990621, 12.50000000000000000, 6.495190528383297135 ) ) ;
#128262 = CARTESIAN_POINT ( 'NONE',  ( -5.000000000000022204, 2.500000000000000000, 3.637306695894644726 ) ) ;
#128263 = CONICAL_SURFACE ( 'NONE', #119835, 0.09999999999999982514, 0.003490658503988666988 ) ;
#128264 = AXIS2_PLACEMENT_3D ( 'NONE', #84874, #124810, #75686 ) ;
#128265 = VERTEX_POINT ( 'NONE', #59933 ) ;
#128266 = DIRECTION ( 'NONE',  ( -4.274815082592931898E-19, -0.9999939076577903929, -0.003490651415223739937 ) ) ;
#128267 = CIRCLE ( 'NONE', #32127, 0.09999999999999982514 ) ;
#128268 = CARTESIAN_POINT ( 'NONE',  ( 17.50000000000000000, -2.750000000000000444, -3.999999999999998224 ) ) ;
#128269 = CARTESIAN_POINT ( 'NONE',  ( 8.749999999999953815, 2.500000000000000000, -2.165063509461101710 ) ) ;
#128271 = ORIENTED_EDGE ( 'NONE', *, *, #9847, .F. ) ;
#128270 = CARTESIAN_POINT ( 'NONE',  ( 9.349999999999919709, 12.50000000000000000, 1.818653347947321475 ) ) ;
#128272 = DIRECTION ( 'NONE',  ( 1.000000000000000000, 0.000000000000000000, 0.000000000000000000 ) ) ;
#128273 = PLANE ( 'NONE',  #20710 ) ;
#128274 = ORIENTED_EDGE ( 'NONE', *, *, #99872, .F. ) ;
#128275 = ADVANCED_FACE ( 'NONE', ( #77598 ), #55379, .T. ) ;
#128276 = VECTOR ( 'NONE', #29757, 1000.000000000000000 ) ;
#128277 = CIRCLE ( 'NONE', #98922, 0.1000000000000002554 ) ;
#128278 = CONICAL_SURFACE ( 'NONE', #25861, 0.1000000000000000472, 0.003490658503988666988 ) ;
#128279 = EDGE_LOOP ( 'NONE', ( #89264, #111859, #57320, #119780 ) ) ;
#128280 = ORIENTED_EDGE ( 'NONE', *, *, #120186, .T. ) ;
#128281 = DIRECTION ( 'NONE',  ( 0.000000000000000000, 0.000000000000000000, 1.000000000000000000 ) ) ;
#128282 = DIRECTION ( 'NONE',  ( 0.000000000000000000, 0.000000000000000000, 1.000000000000000000 ) ) ;
#128283 = VECTOR ( 'NONE', #67596, 1000.000000000000000 ) ;
#128284 = VERTEX_POINT ( 'NONE', #8853 ) ;
#128285 = CARTESIAN_POINT ( 'NONE',  ( -13.09999999999999254, 12.50000000000000000, -3.983716857408423628 ) ) ;
#128286 = FACE_OUTER_BOUND ( 'NONE', #98196, .T. ) ;
#128287 = EDGE_CURVE ( 'NONE', #77998, #45135, #103498, .T. ) ;
#128288 = CARTESIAN_POINT ( 'NONE',  ( 7.699999999999922018, 12.50000000000000000, 0.2813168883297361700 ) ) ;
#128289 = FACE_OUTER_BOUND ( 'NONE', #6939, .T. ) ;
#128290 = ORIENTED_EDGE ( 'NONE', *, *, #121066, .T. ) ;
#128291 = CARTESIAN_POINT ( 'NONE',  ( -1.650000000000035216, 12.50000000000000000, -1.472243186433550122 ) ) ;
#128292 = ORIENTED_EDGE ( 'NONE', *, *, #100439, .T. ) ;
#128293 = ORIENTED_EDGE ( 'NONE', *, *, #10990, .T. ) ;
#128295 = AXIS2_PLACEMENT_3D ( 'NONE', #101982, #123533, #32626 ) ;
#128294 = CARTESIAN_POINT ( 'NONE',  ( -7.900000000000014566, 12.50000000000000000, -0.06509327318403970719 ) ) ;
#128296 = CIRCLE ( 'NONE', #71858, 0.06509327318403745899 ) ;
#128297 = DIRECTION ( 'NONE',  ( 0.000000000000000000, -0.9999939076577903929, 0.003490651415223739937 ) ) ;
#128298 = FACE_BOUND ( 'NONE', #33566, .T. ) ;
#128299 = LINE ( 'NONE', #38642, #63866 ) ;
#128300 = CARTESIAN_POINT ( 'NONE',  ( -7.900000000000014566, 12.50000000000000000, -4.330127018922201643 ) ) ;
#128301 = DIRECTION ( 'NONE',  ( 0.000000000000000000, -0.000000000000000000, 1.000000000000000000 ) ) ;
#128302 = AXIS2_PLACEMENT_3D ( 'NONE', #41532, #80148, #60523 ) ;
#128303 = VECTOR ( 'NONE', #65272, 1000.000000000000000 ) ;
#128304 = VECTOR ( 'NONE', #77749, 1000.000000000000000 ) ;
#128305 = AXIS2_PLACEMENT_3D ( 'NONE', #77001, #46905, #116908 ) ;
#128306 = CIRCLE ( 'NONE', #57189, 0.1000000000000002554 ) ;
#128307 = EDGE_LOOP ( 'NONE', ( #120771, #84355 ) ) ;
#128308 = FACE_OUTER_BOUND ( 'NONE', #24976, .T. ) ;
#128309 = DIRECTION ( 'NONE',  ( 0.000000000000000000, 1.000000000000000000, 0.000000000000000000 ) ) ;
#128310 = DIRECTION ( 'NONE',  ( -4.274815082592931898E-19, -0.9999939076577903929, -0.003490651415223739937 ) ) ;
#128311 = CARTESIAN_POINT ( 'NONE',  ( 186.4062500006828031, -8.891194145520236347, -1.633285867636356299E-15 ) ) ;
#128312 = ORIENTED_EDGE ( 'NONE', *, *, #95051, .T. ) ;
#128314 = CARTESIAN_POINT ( 'NONE',  ( 8.549999999999922551, 12.50000000000000000, -6.148780366869526226 ) ) ;
#128313 = AXIS2_PLACEMENT_3D ( 'NONE', #79181, #108617, #49079 ) ;
#128315 = AXIS2_PLACEMENT_3D ( 'NONE', #32278, #93116, #22454 ) ;
#128317 = EDGE_CURVE ( 'NONE', #4728, #113637, #51292, .T. ) ;
#128316 = AXIS2_PLACEMENT_3D ( 'NONE', #124609, #34954, #56494 ) ;
#128318 = LINE ( 'NONE', #58917, #11854 ) ;
#128319 = VERTEX_POINT ( 'NONE', #29175 ) ;
#128320 = ORIENTED_EDGE ( 'NONE', *, *, #121474, .F. ) ;
#128321 = CONICAL_SURFACE ( 'NONE', #88598, 0.1000000000000002554, 0.003490658503988666988 ) ;
#128322 = CARTESIAN_POINT ( 'NONE',  ( -3.350000000000028955, 2.500000000000000000, 5.802370205355744659 ) ) ;
#128323 = DIRECTION ( 'NONE',  ( -0.000000000000000000, -1.000000000000000000, -0.000000000000000000 ) ) ;
#128324 = FACE_BOUND ( 'NONE', #39900, .T. ) ;
#128325 = EDGE_CURVE ( 'NONE', #123030, #35541, #23194, .T. ) ;
#128326 = CARTESIAN_POINT ( 'NONE',  ( 12.30568799055497564, -2.500000000000000444, -7.490555763477718898 ) ) ;
#128327 = EDGE_LOOP ( 'NONE', ( #20154, #66270, #105597, #92394 ) ) ;
#128328 = DIRECTION ( 'NONE',  ( 0.000000000000000000, 0.000000000000000000, -1.000000000000000000 ) ) ;
#128329 = EDGE_CURVE ( 'NONE', #25124, #97893, #62506, .T. ) ;
#128330 = ORIENTED_EDGE ( 'NONE', *, *, #11734, .F. ) ;
#128331 = EDGE_CURVE ( 'NONE', #102405, #47378, #67883, .T. ) ;
#128332 = ORIENTED_EDGE ( 'NONE', *, *, #80926, .T. ) ;
#128333 = CARTESIAN_POINT ( 'NONE',  ( -10.60000000000000142, 2.500000000000000000, 4.576537180435972019 ) ) ;
#128334 = EDGE_CURVE ( 'NONE', #82736, #21628, #70048, .T. ) ;
#128335 = ADVANCED_FACE ( 'NONE', ( #71024 ), #111823, .T. ) ;
#128336 = CARTESIAN_POINT ( 'NONE',  ( 185.7500000000000000, 9.429780353434619030E-16, -7.700000000000000178 ) ) ;
#128337 = ADVANCED_FACE ( 'NONE', ( #120763 ), #10773, .T. ) ;
#128339 = EDGE_LOOP ( 'NONE', ( #48999, #14910 ) ) ;
#128338 = AXIS2_PLACEMENT_3D ( 'NONE', #45875, #66139, #26869 ) ;
#128340 = CARTESIAN_POINT ( 'NONE',  ( -9.600000000000008527, 12.50000000000000000, -3.572213422710607933 ) ) ;
#128341 = DIRECTION ( 'NONE',  ( 0.000000000000000000, 1.000000000000000000, 0.000000000000000000 ) ) ;
#128342 = DIRECTION ( 'NONE',  ( 0.000000000000000000, 1.000000000000000000, 0.000000000000000000 ) ) ;
#128344 = ADVANCED_FACE ( 'NONE', ( #102416 ), #40828, .T. ) ;
#128343 = PLANE ( 'NONE',  #69769 ) ;
#128345 = CIRCLE ( 'NONE', #775, 0.06509327318403743123 ) ;
#128347 = EDGE_CURVE ( 'NONE', #53973, #60435, #105559, .T. ) ;
#128346 = VECTOR ( 'NONE', #94331, 1000.000000000000000 ) ;
#128348 = EDGE_CURVE ( 'NONE', #30682, #107108, #76309, .T. ) ;
#128349 = ORIENTED_EDGE ( 'NONE', *, *, #66839, .T. ) ;
#128350 = DIRECTION ( 'NONE',  ( 0.000000000000000000, 0.000000000000000000, 1.000000000000000000 ) ) ;
#128351 = DIRECTION ( 'NONE',  ( -0.000000000000000000, -1.000000000000000000, -0.000000000000000000 ) ) ;
#128352 = PLANE ( 'NONE',  #74316 ) ;
#128353 = CARTESIAN_POINT ( 'NONE',  ( 195.0000000000000000, 0.000000000000000000, -7.541925104783893552 ) ) ;
#128354 = ORIENTED_EDGE ( 'NONE', *, *, #121529, .T. ) ;
#128355 = DIRECTION ( 'NONE',  ( 0.000000000000000000, -0.9999939076577903929, 0.003490651415223739937 ) ) ;
#128356 = ORIENTED_EDGE ( 'NONE', *, *, #7889, .F. ) ;
#128357 = AXIS2_PLACEMENT_3D ( 'NONE', #2383, #62634, #102536 ) ;
#128358 = DIRECTION ( 'NONE',  ( 0.000000000000000000, 1.000000000000000000, 0.000000000000000000 ) ) ;
#128359 = VERTEX_POINT ( 'NONE', #110923 ) ;
#128361 = DIRECTION ( 'NONE',  ( 0.000000000000000000, 0.000000000000000000, 1.000000000000000000 ) ) ;
#128360 = AXIS2_PLACEMENT_3D ( 'NONE', #80225, #20017, #99866 ) ;
#128362 = DIRECTION ( 'NONE',  ( -0.000000000000000000, 1.000000000000000000, -0.000000000000000000 ) ) ;
#128363 = AXIS2_PLACEMENT_3D ( 'NONE', #62595, #119554, #101222 ) ;
#128364 = PLANE ( 'NONE',  #9916 ) ;
#128365 = DIRECTION ( 'NONE',  ( 0.000000000000000000, -0.9999939076577903929, 0.003490651415223739937 ) ) ;
#128366 = ORIENTED_EDGE ( 'NONE', *, *, #14185, .F. ) ;
#128367 = DIRECTION ( 'NONE',  ( 0.000000000000000000, 1.000000000000000000, 0.000000000000000000 ) ) ;
#128368 = FACE_OUTER_BOUND ( 'NONE', #93193, .T. ) ;
#128369 = CARTESIAN_POINT ( 'NONE',  ( 179.5000000000000000, -1.375000000000000000, 7.634788798650553154 ) ) ;
#128370 = DIRECTION ( 'NONE',  ( 0.000000000000000000, 0.000000000000000000, 1.000000000000000000 ) ) ;
#128371 = CARTESIAN_POINT ( 'NONE',  ( -8.150000000000009237, 2.500000000000000000, 6.248780366869520542 ) ) ;
#128372 = CARTESIAN_POINT ( 'NONE',  ( -12.89999999999999147, 12.50000000000000000, -5.022947341949751454 ) ) ;
#128373 = ORIENTED_EDGE ( 'NONE', *, *, #111197, .T. ) ;
#128374 = EDGE_LOOP ( 'NONE', ( #73388, #95090 ) ) ;
#128375 = CARTESIAN_POINT ( 'NONE',  ( 9.599999999999914380, 2.500000000000000000, 5.022947341949748790 ) ) ;
#128377 = ORIENTED_EDGE ( 'NONE', *, *, #124484, .T. ) ;
#128376 = AXIS2_PLACEMENT_3D ( 'NONE', #126, #99640, #39456 ) ;
#128378 = CONICAL_SURFACE ( 'NONE', #76030, 0.09999999999999982514, 0.003490658503988666988 ) ;
#128379 = CIRCLE ( 'NONE', #71932, 0.06509327318403745899 ) ;
#128380 = CARTESIAN_POINT ( 'NONE',  ( 8.099999999999923261, 12.50000000000000000, -4.676537180435978769 ) ) ;
#128382 = ORIENTED_EDGE ( 'NONE', *, *, #47768, .F. ) ;
#128381 = ORIENTED_EDGE ( 'NONE', *, *, #41588, .T. ) ;
#128383 = VERTEX_POINT ( 'NONE', #82125 ) ;
#128384 = CIRCLE ( 'NONE', #82406, 0.06509327318403745899 ) ;
#128385 = CARTESIAN_POINT ( 'NONE',  ( 87.50000000000001421, 3.413194297214863671, -6.711110875543777610 ) ) ;
#128386 = AXIS2_PLACEMENT_3D ( 'NONE', #53452, #122828, #101899 ) ;
#128387 = DIRECTION ( 'NONE',  ( -0.000000000000000000, -1.000000000000000000, -0.000000000000000000 ) ) ;
#128388 = LINE ( 'NONE', #107431, #60216 ) ;
#128389 = LINE ( 'NONE', #26308, #122504 ) ;
#128390 = DIRECTION ( 'NONE',  ( 0.000000000000000000, 0.000000000000000000, -1.000000000000000000 ) ) ;
#128391 = DIRECTION ( 'NONE',  ( 0.000000000000000000, 1.000000000000000000, 0.000000000000000000 ) ) ;
#128392 = CARTESIAN_POINT ( 'NONE',  ( 8.949999999999915801, 2.500000000000000000, 6.941600689897073018 ) ) ;
#128393 = ADVANCED_FACE ( 'NONE', ( #2931 ), #61646, .T. ) ;
#128394 = FACE_OUTER_BOUND ( 'NONE', #11685, .T. ) ;
#128395 = ORIENTED_EDGE ( 'NONE', *, *, #77926, .T. ) ;
#128396 = ADVANCED_FACE ( 'NONE', ( #93243 ), #5182, .T. ) ;
#128397 = ORIENTED_EDGE ( 'NONE', *, *, #105848, .F. ) ;
#128398 = ORIENTED_EDGE ( 'NONE', *, *, #122718, .T. ) ;
#128399 = EDGE_CURVE ( 'NONE', #116265, #123569, #61854, .T. ) ;
#128400 = CIRCLE ( 'NONE', #101272, 0.06509327318403745899 ) ;
#128401 = DIRECTION ( 'NONE',  ( 0.000000000000000000, 1.000000000000000000, 0.000000000000000000 ) ) ;
#128402 = AXIS2_PLACEMENT_3D ( 'NONE', #101179, #22634, #62554 ) ;
#128403 = CIRCLE ( 'NONE', #71955, 0.1000000000000002554 ) ;
#128404 = ORIENTED_EDGE ( 'NONE', *, *, #53733, .F. ) ;
#128405 = ORIENTED_EDGE ( 'NONE', *, *, #95683, .F. ) ;
#128406 = DIRECTION ( 'NONE',  ( -0.000000000000000000, 1.000000000000000000, -0.000000000000000000 ) ) ;
#128407 = EDGE_CURVE ( 'NONE', #129005, #52447, #60575, .T. ) ;
#128408 = AXIS2_PLACEMENT_3D ( 'NONE', #77409, #85919, #17836 ) ;
#128409 = CARTESIAN_POINT ( 'NONE',  ( 5.449999999999936229, 2.500000000000000000, -2.065063509461102065 ) ) ;
#128411 = CARTESIAN_POINT ( 'NONE',  ( 194.5000000000000000, 0.000000000000000000, 0.000000000000000000 ) ) ;
#128410 = VECTOR ( 'NONE', #10708, 1000.000000000000000 ) ;
#128412 = DIRECTION ( 'NONE',  ( -0.000000000000000000, -1.000000000000000000, -0.000000000000000000 ) ) ;
#128413 = CARTESIAN_POINT ( 'NONE',  ( 12.29999999999990479, 12.50000000000000000, -4.048810130592463530 ) ) ;
#128414 = ORIENTED_EDGE ( 'NONE', *, *, #66837, .F. ) ;
#128415 = DIRECTION ( 'NONE',  ( 0.000000000000000000, -0.000000000000000000, 1.000000000000000000 ) ) ;
#128416 = CIRCLE ( 'NONE', #126337, 0.1000000000000002554 ) ;
#128418 = ORIENTED_EDGE ( 'NONE', *, *, #102895, .T. ) ;
#128417 = CIRCLE ( 'NONE', #88679, 0.06509327318403745899 ) ;
#128419 = DIRECTION ( 'NONE',  ( 0.000000000000000000, 1.000000000000000000, 0.000000000000000000 ) ) ;
#128420 = CIRCLE ( 'NONE', #48988, 0.09999999999999982514 ) ;
#128421 = ORIENTED_EDGE ( 'NONE', *, *, #61078, .F. ) ;
#128422 = CARTESIAN_POINT ( 'NONE',  ( 7.499999999999923617, 12.50000000000000000, 0.7579135962115869374 ) ) ;
#128423 = ORIENTED_EDGE ( 'NONE', *, *, #16281, .T. ) ;
#128424 = CONICAL_SURFACE ( 'NONE', #115864, 0.1000000000000002554, 0.003490658503988666988 ) ;
#128425 = EDGE_CURVE ( 'NONE', #128215, #124558, #122292, .T. ) ;
#128426 = EDGE_LOOP ( 'NONE', ( #113174, #81407 ) ) ;
#128427 = CARTESIAN_POINT ( 'NONE',  ( -5.850000000000021849, 2.500000000000000000, -5.802370205355749988 ) ) ;
#128428 = DIRECTION ( 'NONE',  ( -0.000000000000000000, 1.000000000000000000, -0.000000000000000000 ) ) ;
#128429 = CARTESIAN_POINT ( 'NONE',  ( -2.300000000000033573, 12.50000000000000000, 4.741630453620009789 ) ) ;
#128430 = DIRECTION ( 'NONE',  ( -0.000000000000000000, 1.000000000000000000, -0.000000000000000000 ) ) ;
#128431 = LINE ( 'NONE', #98944, #74302 ) ;
#128432 = ORIENTED_EDGE ( 'NONE', *, *, #29635, .F. ) ;
#128433 = DIRECTION ( 'NONE',  ( 0.000000000000000000, 1.000000000000000000, 0.000000000000000000 ) ) ;
#128434 = FACE_OUTER_BOUND ( 'NONE', #81518, .T. ) ;
#128435 = FACE_OUTER_BOUND ( 'NONE', #127810, .T. ) ;
#128436 = CARTESIAN_POINT ( 'NONE',  ( -8.750000000000005329, 12.50000000000000000, 5.737276932171707422 ) ) ;
#128437 = AXIS2_PLACEMENT_3D ( 'NONE', #20269, #26013, #5701 ) ;
#128438 = LINE ( 'NONE', #110693, #58196 ) ;
#128439 = ORIENTED_EDGE ( 'NONE', *, *, #92153, .F. ) ;
#128440 = EDGE_CURVE ( 'NONE', #48843, #63643, #121400, .T. ) ;
#128441 = ORIENTED_EDGE ( 'NONE', *, *, #87055, .T. ) ;
#128442 = CARTESIAN_POINT ( 'NONE',  ( 13.94999999999989271, 12.50000000000000000, -1.753560074763288679 ) ) ;
#128443 = ORIENTED_EDGE ( 'NONE', *, *, #35200, .F. ) ;
#128444 = CIRCLE ( 'NONE', #109553, 0.09999999999999982514 ) ;
#128445 = CARTESIAN_POINT ( 'NONE',  ( 17.50000000000000000, -2.500000000000000000, 2.922290670089274567 ) ) ;
#128446 = CARTESIAN_POINT ( 'NONE',  ( 9.599999999999914380, 12.50000000000000000, 3.572213422710607489 ) ) ;
#128447 = AXIS2_PLACEMENT_3D ( 'NONE', #72605, #103995, #14303 ) ;
#128448 = VERTEX_POINT ( 'NONE', #21931 ) ;
#128449 = CARTESIAN_POINT ( 'NONE',  ( 186.2083333333333144, -4.445597072760115509, -7.700000000000001954 ) ) ;
#128450 = CARTESIAN_POINT ( 'NONE',  ( 13.94999999999989626, 2.500000000000000000, 2.411473670974873862 ) ) ;
#128451 = EDGE_CURVE ( 'NONE', #79468, #61045, #90974, .T. ) ;
#128452 = CARTESIAN_POINT ( 'NONE',  ( -10.85000000000000142, 12.50000000000000000, -1.537336459617583584 ) ) ;
#128453 = CARTESIAN_POINT ( 'NONE',  ( 7.049999999999926992, 12.50000000000000000, 2.165063509461097713 ) ) ;
#128454 = ORIENTED_EDGE ( 'NONE', *, *, #31536, .T. ) ;
#128455 = AXIS2_PLACEMENT_3D ( 'NONE', #127945, #48755, #6216 ) ;
#128456 = CARTESIAN_POINT ( 'NONE',  ( -13.14999999999999147, 2.500000000000000000, -2.411473670974875638 ) ) ;
#128457 = ORIENTED_EDGE ( 'NONE', *, *, #5063, .F. ) ;
#128458 = CARTESIAN_POINT ( 'NONE',  ( 26.61817589030699338, 2.722754549395931978, -4.358315860969328881 ) ) ;
#128459 = CARTESIAN_POINT ( 'NONE',  ( 9.349999999999919709, 2.500000000000000000, -6.248780366869526759 ) ) ;
#128460 = DIRECTION ( 'NONE',  ( 0.000000000000000000, 0.000000000000000000, -1.000000000000000000 ) ) ;
#128461 = ORIENTED_EDGE ( 'NONE', *, *, #105863, .F. ) ;
#128462 = AXIS2_PLACEMENT_3D ( 'NONE', #76623, #94309, #46501 ) ;
#128463 = CARTESIAN_POINT ( 'NONE',  ( -1.650000000000034328, 2.500000000000000000, -7.288010851410854585 ) ) ;
#128465 = VERTEX_POINT ( 'NONE', #112235 ) ;
#128464 = AXIS2_PLACEMENT_3D ( 'NONE', #85179, #4656, #114008 ) ;
#128466 = DIRECTION ( 'NONE',  ( -4.274815082592931898E-19, -0.9999939076577903929, -0.003490651415223739937 ) ) ;
#128467 = CARTESIAN_POINT ( 'NONE',  ( 184.5000000000000000, 6.368163355566236381E-16, 5.200000000000000178 ) ) ;
#128468 = DIRECTION ( 'NONE',  ( 0.000000000000000000, 1.000000000000000000, 0.000000000000000000 ) ) ;
#128469 = VECTOR ( 'NONE', #45565, 1000.000000000000000 ) ;
#128470 = ORIENTED_EDGE ( 'NONE', *, *, #46165, .T. ) ;
#128471 = DIRECTION ( 'NONE',  ( 0.000000000000000000, 1.000000000000000000, 0.000000000000000000 ) ) ;
#128472 = EDGE_CURVE ( 'NONE', #104829, #25799, #22589, .T. ) ;
#128473 = FACE_OUTER_BOUND ( 'NONE', #58685, .T. ) ;
#128474 = ORIENTED_EDGE ( 'NONE', *, *, #18242, .F. ) ;
#128475 = CARTESIAN_POINT ( 'NONE',  ( 12.04999999999990479, 2.500000000000000000, -6.495190528383302464 ) ) ;
#128476 = ORIENTED_EDGE ( 'NONE', *, *, #91738, .F. ) ;
#128477 = LINE ( 'NONE', #55842, #53676 ) ;
#128478 = EDGE_CURVE ( 'NONE', #19198, #113972, #30360, .T. ) ;
#128479 = CIRCLE ( 'NONE', #103336, 0.06509327318403745899 ) ;
#128480 = ORIENTED_EDGE ( 'NONE', *, *, #32835, .T. ) ;
#128481 = FACE_OUTER_BOUND ( 'NONE', #79441, .T. ) ;
#128482 = CARTESIAN_POINT ( 'NONE',  ( -1.650000000000035216, 12.50000000000000000, -1.472243186433550122 ) ) ;
#128483 = AXIS2_PLACEMENT_3D ( 'NONE', #50177, #88793, #88113 ) ;
#128484 = EDGE_CURVE ( 'NONE', #29292, #83964, #105639, .T. ) ;
#128485 = AXIS2_PLACEMENT_3D ( 'NONE', #86134, #126076, #58648 ) ;
#128486 = ORIENTED_EDGE ( 'NONE', *, *, #91360, .T. ) ;
#128487 = ADVANCED_FACE ( 'NONE', ( #55878 ), #36903, .T. ) ;
#128488 = ORIENTED_EDGE ( 'NONE', *, *, #112200, .T. ) ;
#128489 = ADVANCED_FACE ( 'NONE', ( #106276 ), #19882, .T. ) ;
#128490 = EDGE_CURVE ( 'NONE', #75076, #124980, #80524, .T. ) ;
#128491 = DIRECTION ( 'NONE',  ( -4.274815082592931898E-19, -0.9999939076577903929, -0.003490651415223739937 ) ) ;
#128492 = CARTESIAN_POINT ( 'NONE',  ( 3.749999999999942268, 2.500000000000000000, -5.902370205355750521 ) ) ;
#128493 = ORIENTED_EDGE ( 'NONE', *, *, #2679, .F. ) ;
#128494 = DIRECTION ( 'NONE',  ( 0.000000000000000000, 0.000000000000000000, 1.000000000000000000 ) ) ;
#128495 = DIRECTION ( 'NONE',  ( 0.000000000000000000, 0.000000000000000000, 1.000000000000000000 ) ) ;
#128496 = CIRCLE ( 'NONE', #113812, 0.06509327318403745899 ) ;
#128497 = VECTOR ( 'NONE', #101622, 1000.000000000000000 ) ;
#128498 = AXIS2_PLACEMENT_3D ( 'NONE', #23133, #33607, #73513 ) ;
#128499 = FACE_OUTER_BOUND ( 'NONE', #128582, .T. ) ;
#128500 = ADVANCED_FACE ( 'NONE', ( #75512 ), #125899, .T. ) ;
#128501 = LINE ( 'NONE', #59759, #1247 ) ;
#128502 = FACE_OUTER_BOUND ( 'NONE', #52095, .T. ) ;
#128504 = EDGE_CURVE ( 'NONE', #11437, #102844, #7429, .T. ) ;
#128503 = AXIS2_PLACEMENT_3D ( 'NONE', #36668, #47126, #76578 ) ;
#128505 = FACE_OUTER_BOUND ( 'NONE', #16696, .T. ) ;
#128506 = CARTESIAN_POINT ( 'NONE',  ( -10.65000000000000213, 12.50000000000000000, 6.776507416713035248 ) ) ;
#128507 = EDGE_CURVE ( 'NONE', #110767, #18837, #88923, .T. ) ;
#128508 = EDGE_CURVE ( 'NONE', #44931, #84059, #25130, .T. ) ;
#128509 = AXIS2_PLACEMENT_3D ( 'NONE', #29242, #88789, #46949 ) ;
#128510 = CIRCLE ( 'NONE', #109713, 0.1000000000000000472 ) ;
#128511 = ADVANCED_FACE ( 'NONE', ( #95170 ), #47157, .T. ) ;
#128512 = ORIENTED_EDGE ( 'NONE', *, *, #120509, .T. ) ;
#128513 = ORIENTED_EDGE ( 'NONE', *, *, #54147, .T. ) ;
#128514 = ORIENTED_EDGE ( 'NONE', *, *, #34396, .F. ) ;
#128515 = EDGE_LOOP ( 'NONE', ( #45200, #73996, #29661, #26920 ) ) ;
#128516 = FACE_OUTER_BOUND ( 'NONE', #46545, .T. ) ;
#128517 = CARTESIAN_POINT ( 'NONE',  ( 11.24999999999994493, 2.500000000000000000, -2.165063509461101710 ) ) ;
#128518 = AXIS2_PLACEMENT_3D ( 'NONE', #58694, #31187, #28595 ) ;
#128519 = DIRECTION ( 'NONE',  ( 0.000000000000000000, 0.000000000000000000, 1.000000000000000000 ) ) ;
#128520 = ORIENTED_EDGE ( 'NONE', *, *, #111281, .T. ) ;
#128521 = FACE_BOUND ( 'NONE', #11779, .T. ) ;
#128522 = ORIENTED_EDGE ( 'NONE', *, *, #21663, .T. ) ;
#128523 = EDGE_CURVE ( 'NONE', #100830, #18875, #116092, .T. ) ;
#128524 = CARTESIAN_POINT ( 'NONE',  ( 9.149999999999916866, 2.500000000000000000, 7.188010851410848723 ) ) ;
#128525 = DIRECTION ( 'NONE',  ( -0.000000000000000000, 1.000000000000000000, -0.000000000000000000 ) ) ;
#128526 = CARTESIAN_POINT ( 'NONE',  ( -10.84999999999999964, 12.50000000000000000, 1.472243186433545459 ) ) ;
#128527 = CARTESIAN_POINT ( 'NONE',  ( -8.150000000000014566, 2.500000000000000000, -6.841600689897073373 ) ) ;
#128528 = FACE_OUTER_BOUND ( 'NONE', #19329, .T. ) ;
#128529 = DIRECTION ( 'NONE',  ( 0.000000000000000000, -0.000000000000000000, 1.000000000000000000 ) ) ;
#128530 = DIRECTION ( 'NONE',  ( 0.000000000000000000, 1.000000000000000000, 0.000000000000000000 ) ) ;
#128531 = DIRECTION ( 'NONE',  ( 0.000000000000000000, 1.000000000000000000, 0.000000000000000000 ) ) ;
#128532 = FACE_OUTER_BOUND ( 'NONE', #109107, .T. ) ;
#128533 = VECTOR ( 'NONE', #24401, 1000.000000000000000 ) ;
#128534 = DIRECTION ( 'NONE',  ( 0.000000000000000000, 0.000000000000000000, 1.000000000000000000 ) ) ;
#128535 = ORIENTED_EDGE ( 'NONE', *, *, #81501, .T. ) ;
#128536 = ORIENTED_EDGE ( 'NONE', *, *, #111624, .T. ) ;
#128537 = VERTEX_POINT ( 'NONE', #14649 ) ;
#128538 = ORIENTED_EDGE ( 'NONE', *, *, #94147, .F. ) ;
#128539 = DIRECTION ( 'NONE',  ( 0.000000000000000000, -0.9999939076577903929, 0.003490651415223739937 ) ) ;
#128540 = DIRECTION ( 'NONE',  ( -0.000000000000000000, 1.000000000000000000, -0.000000000000000000 ) ) ;
#128542 = ORIENTED_EDGE ( 'NONE', *, *, #47318, .T. ) ;
#128541 = EDGE_LOOP ( 'NONE', ( #75432, #98630, #27824, #106390 ) ) ;
#128543 = EDGE_LOOP ( 'NONE', ( #61999, #64732 ) ) ;
#128544 = CARTESIAN_POINT ( 'NONE',  ( 185.2083333333333144, -4.445597072760163471, -7.699999999999919353 ) ) ;
#128545 = AXIS2_PLACEMENT_3D ( 'NONE', #106427, #16731, #7571 ) ;
#128546 = AXIS2_PLACEMENT_3D ( 'NONE', #115733, #96728, #7057 ) ;
#128547 = CARTESIAN_POINT ( 'NONE',  ( 13.74999999999989875, 2.500000000000000000, 1.472243186433545459 ) ) ;
#128548 = FACE_OUTER_BOUND ( 'NONE', #114032, .T. ) ;
#128549 = CARTESIAN_POINT ( 'NONE',  ( -10.85000000000000142, 2.500000000000000000, -2.757883832488650100 ) ) ;
#128550 = DIRECTION ( 'NONE',  ( 0.000000000000000000, 1.000000000000000000, 0.000000000000000000 ) ) ;
#128551 = FACE_OUTER_BOUND ( 'NONE', #78533, .T. ) ;
#128552 = LINE ( 'NONE', #19185, #63565 ) ;
#128553 = ORIENTED_EDGE ( 'NONE', *, *, #102488, .T. ) ;
#128554 = PLANE ( 'NONE',  #55942 ) ;
#128555 = VERTEX_POINT ( 'NONE', #35612 ) ;
#128556 = CIRCLE ( 'NONE', #983, 0.06509327318403745899 ) ;
#128557 = EDGE_CURVE ( 'NONE', #110134, #51506, #3244, .T. ) ;
#128558 = ORIENTED_EDGE ( 'NONE', *, *, #70904, .T. ) ;
#128559 = EDGE_LOOP ( 'NONE', ( #80572, #122542, #117462, #63304 ) ) ;
#128561 = EDGE_CURVE ( 'NONE', #868, #85577, #94513, .T. ) ;
#128560 = CONICAL_SURFACE ( 'NONE', #88810, 0.1000000000000002554, 0.003490658503988666988 ) ;
#128562 = FACE_OUTER_BOUND ( 'NONE', #10984, .T. ) ;
#128563 = ORIENTED_EDGE ( 'NONE', *, *, #97903, .T. ) ;
#128564 = ORIENTED_EDGE ( 'NONE', *, *, #35271, .T. ) ;
#128565 = CARTESIAN_POINT ( 'NONE',  ( 3.749999999999942268, 12.50000000000000000, -5.802370205355749988 ) ) ;
#128566 = EDGE_CURVE ( 'NONE', #128537, #16422, #114059, .T. ) ;
#128569 = ADVANCED_FACE ( 'NONE', ( #4832 ), #25776, .T. ) ;
#128568 = AXIS2_PLACEMENT_3D ( 'NONE', #25246, #16708, #127350 ) ;
#128567 = DIRECTION ( 'NONE',  ( 0.000000000000000000, 1.000000000000000000, 0.000000000000000000 ) ) ;
#128570 = CARTESIAN_POINT ( 'NONE',  ( 3.299999999999944755, 12.50000000000000000, -4.330127018922201643 ) ) ;
#128571 = AXIS2_PLACEMENT_3D ( 'NONE', #33674, #72319, #73578 ) ;
#128572 = LINE ( 'NONE', #17933, #14839 ) ;
#128573 = CARTESIAN_POINT ( 'NONE',  ( -6.650000000000015454, 12.50000000000000000, 7.122917578226811486 ) ) ;
#128574 = ORIENTED_EDGE ( 'NONE', *, *, #35369, .T. ) ;
#128575 = AXIS2_PLACEMENT_3D ( 'NONE', #90623, #2899, #101742 ) ;
#128576 = CARTESIAN_POINT ( 'NONE',  ( 13.74999999999993072, 2.500000000000000000, -2.265063509461101798 ) ) ;
#128577 = ORIENTED_EDGE ( 'NONE', *, *, #12865, .T. ) ;
#128578 = CARTESIAN_POINT ( 'NONE',  ( 16.56034315062901641, -0.8287392047036244991, 6.090234455234610600 ) ) ;
#128579 = ORIENTED_EDGE ( 'NONE', *, *, #119181, .T. ) ;
#128580 = DIRECTION ( 'NONE',  ( -0.000000000000000000, 1.000000000000000000, -0.000000000000000000 ) ) ;
#128581 = FACE_OUTER_BOUND ( 'NONE', #58378, .T. ) ;
#128582 = EDGE_LOOP ( 'NONE', ( #66541, #72841, #124338, #61079 ) ) ;
#128583 = CARTESIAN_POINT ( 'NONE',  ( 9.149999999999920419, 2.500000000000000000, 1.472243186433545459 ) ) ;
#128584 = DIRECTION ( 'NONE',  ( 0.000000000000000000, 0.000000000000000000, 1.000000000000000000 ) ) ;
#128585 = VERTEX_POINT ( 'NONE', #74889 ) ;
#128587 = FACE_OUTER_BOUND ( 'NONE', #67488, .T. ) ;
#128586 = VECTOR ( 'NONE', #2997, 1000.000000000000000 ) ;
#128588 = EDGE_LOOP ( 'NONE', ( #2052, #108065, #10818, #2446 ) ) ;
#128589 = AXIS2_PLACEMENT_3D ( 'NONE', #36766, #37407, #5344 ) ;
#128590 = EDGE_LOOP ( 'NONE', ( #60305, #91895 ) ) ;
#128591 = DIRECTION ( 'NONE',  ( 0.000000000000000000, 1.000000000000000000, 0.000000000000000000 ) ) ;
#128592 = CARTESIAN_POINT ( 'NONE',  ( 12.09999999999990550, 12.50000000000000000, 3.637306695894644726 ) ) ;
#128593 = CARTESIAN_POINT ( 'NONE',  ( 184.4218750003414016, 0.000000000000000000, 7.564683531250000925 ) ) ;
#128594 = DIRECTION ( 'NONE',  ( 0.000000000000000000, 0.000000000000000000, -1.000000000000000000 ) ) ;
#128595 = EDGE_CURVE ( 'NONE', #83042, #70566, #78478, .T. ) ;
#128596 = AXIS2_PLACEMENT_3D ( 'NONE', #91506, #102604, #32621 ) ;
#128597 = DIRECTION ( 'NONE',  ( -0.000000000000000000, 1.000000000000000000, -0.000000000000000000 ) ) ;
#128598 = CONICAL_SURFACE ( 'NONE', #57471, 0.09999999999999999167, 0.003490658503988666988 ) ;
#128599 = ORIENTED_EDGE ( 'NONE', *, *, #61256, .F. ) ;
#128600 = AXIS2_PLACEMENT_3D ( 'NONE', #54630, #65089, #4235 ) ;
#128601 = CARTESIAN_POINT ( 'NONE',  ( -10.60000000000000142, 2.500000000000000000, 3.983716857408420964 ) ) ;
#128602 = AXIS2_PLACEMENT_3D ( 'NONE', #118267, #28615, #46301 ) ;
#128603 = EDGE_LOOP ( 'NONE', ( #70471, #23873 ) ) ;
#128604 = CIRCLE ( 'NONE', #120170, 0.1000000000000000472 ) ;
#128605 = DIRECTION ( 'NONE',  ( 0.000000000000000000, 1.000000000000000000, 0.000000000000000000 ) ) ;
#128607 = AXIS2_PLACEMENT_3D ( 'NONE', #121399, #31740, #90651 ) ;
#128606 = CARTESIAN_POINT ( 'NONE',  ( 1.649999999999951505, 2.500000000000000000, -1.472243186433550122 ) ) ;
#128608 = ORIENTED_EDGE ( 'NONE', *, *, #81033, .F. ) ;
#128609 = CONICAL_SURFACE ( 'NONE', #17752, 0.1000000000000002554, 0.003490658503988666988 ) ;
#128610 = ADVANCED_FACE ( 'NONE', ( #104963 ), #109855, .T. ) ;
#128611 = DIRECTION ( 'NONE',  ( -0.000000000000000000, -1.000000000000000000, -0.000000000000000000 ) ) ;
#128612 = LINE ( 'NONE', #116813, #38520 ) ;
#128613 = CARTESIAN_POINT ( 'NONE',  ( 6.049999999999935874, 12.50000000000000000, -6.776507416713039689 ) ) ;
#128614 = ADVANCED_FACE ( 'NONE', ( #65702 ), #19968, .T. ) ;
#128615 = CARTESIAN_POINT ( 'NONE',  ( 10.39999999999991509, 2.500000000000000000, -0.5928203230275542746 ) ) ;
#128616 = DIRECTION ( 'NONE',  ( 0.000000000000000000, -0.000000000000000000, 1.000000000000000000 ) ) ;
#128617 = ORIENTED_EDGE ( 'NONE', *, *, #71108, .T. ) ;
#128618 = DIRECTION ( 'NONE',  ( 0.000000000000000000, 1.000000000000000000, 0.000000000000000000 ) ) ;
#128619 = DIRECTION ( 'NONE',  ( -0.000000000000000000, -1.000000000000000000, -0.000000000000000000 ) ) ;
#128620 = DIRECTION ( 'NONE',  ( 0.000000000000000000, -0.000000000000000000, 1.000000000000000000 ) ) ;
#128621 = EDGE_CURVE ( 'NONE', #59948, #112383, #108840, .T. ) ;
#128622 = CIRCLE ( 'NONE', #40792, 0.06509327318403745899 ) ;
#128623 = EDGE_LOOP ( 'NONE', ( #83903, #62938 ) ) ;
#128624 = FACE_OUTER_BOUND ( 'NONE', #1756, .T. ) ;
#128625 = ORIENTED_EDGE ( 'NONE', *, *, #104454, .F. ) ;
#128626 = ORIENTED_EDGE ( 'NONE', *, *, #122795, .T. ) ;
#128627 = DIRECTION ( 'NONE',  ( 0.000000000000000000, -0.9999939076577903929, 0.003490651415223739937 ) ) ;
#128628 = CONICAL_SURFACE ( 'NONE', #15712, 0.1000000000000002554, 0.003490658503988666988 ) ;
#128629 = ORIENTED_EDGE ( 'NONE', *, *, #93567, .F. ) ;
#128630 = PLANE ( 'NONE',  #59092 ) ;
#128631 = CARTESIAN_POINT ( 'NONE',  ( -8.550000000000007816, 2.500000000000000000, 6.048780366869520364 ) ) ;
#128632 = AXIS2_PLACEMENT_3D ( 'NONE', #1625, #42216, #51406 ) ;
#128633 = AXIS2_PLACEMENT_3D ( 'NONE', #54717, #67094, #85481 ) ;
#128634 = ORIENTED_EDGE ( 'NONE', *, *, #18494, .F. ) ;
#128635 = CARTESIAN_POINT ( 'NONE',  ( 13.94999999999989271, 12.50000000000000000, -1.883746621131363597 ) ) ;
#128637 = ORIENTED_EDGE ( 'NONE', *, *, #128930, .T. ) ;
#128636 = CARTESIAN_POINT ( 'NONE',  ( -14.99999999999998401, 2.500000000000000000, 0.6928203230275518099 ) ) ;
#128638 = DIRECTION ( 'NONE',  ( 1.000000000000000000, 0.000000000000000000, 0.000000000000000000 ) ) ;
#128639 = DIRECTION ( 'NONE',  ( 0.000000000000000000, 1.000000000000000000, 0.000000000000000000 ) ) ;
#128640 = ORIENTED_EDGE ( 'NONE', *, *, #96867, .F. ) ;
#128641 = CIRCLE ( 'NONE', #90964, 0.06509327318403745899 ) ;
#128642 = EDGE_CURVE ( 'NONE', #104109, #124072, #42978, .T. ) ;
#128643 = ORIENTED_EDGE ( 'NONE', *, *, #20621, .T. ) ;
#128644 = VECTOR ( 'NONE', #65360, 1000.000000000000000 ) ;
#128645 = EDGE_LOOP ( 'NONE', ( #36634, #81636 ) ) ;
#128646 = CARTESIAN_POINT ( 'NONE',  ( -6.850000000000017408, 2.500000000000000000, -2.511473670974877948 ) ) ;
#128647 = CARTESIAN_POINT ( 'NONE',  ( -0.4000000000000396572, 2.500000000000000000, 4.330127018922196314 ) ) ;
#128648 = CARTESIAN_POINT ( 'NONE',  ( 4.399999999999940847, 2.500000000000000000, -4.576537180435977348 ) ) ;
#128649 = EDGE_CURVE ( 'NONE', #58785, #11040, #29020, .T. ) ;
#128650 = FACE_BOUND ( 'NONE', #4634, .T. ) ;
#128651 = VERTEX_POINT ( 'NONE', #57827 ) ;
#128652 = EDGE_CURVE ( 'NONE', #81351, #47988, #47361, .T. ) ;
#128653 = EDGE_CURVE ( 'NONE', #43124, #8732, #5277, .T. ) ;
#128654 = CARTESIAN_POINT ( 'NONE',  ( 7.499999999999961808, 12.50000000000000000, 4.395220292106234439 ) ) ;
#128655 = CARTESIAN_POINT ( 'NONE',  ( 3.299999999999942979, 2.500000000000000000, 4.330127018922196314 ) ) ;
#128656 = ORIENTED_EDGE ( 'NONE', *, *, #75293, .T. ) ;
#128657 = LINE ( 'NONE', #78901, #61226 ) ;
#128658 = CARTESIAN_POINT ( 'NONE',  ( -11.25000000000000178, 2.500000000000000000, -5.802370205355746435 ) ) ;
#128659 = AXIS2_PLACEMENT_3D ( 'NONE', #56521, #65037, #26435 ) ;
#128660 = EDGE_CURVE ( 'NONE', #113932, #50402, #70148, .T. ) ;
#128661 = FACE_OUTER_BOUND ( 'NONE', #49472, .T. ) ;
#128662 = CARTESIAN_POINT ( 'NONE',  ( 3.299999999999944755, 12.50000000000000000, -2.385244779468109755E-15 ) ) ;
#128663 = CARTESIAN_POINT ( 'NONE',  ( 8.099999999999923261, 2.500000000000000000, 3.983716857408420076 ) ) ;
#128664 = EDGE_CURVE ( 'NONE', #128960, #73467, #34656, .T. ) ;
#128665 = CARTESIAN_POINT ( 'NONE',  ( 1.899999999999951283, 2.500000000000000000, -4.776537180435977525 ) ) ;
#128666 = CARTESIAN_POINT ( 'NONE',  ( -1.900000000000034550, 2.500000000000000000, 4.576537180435972019 ) ) ;
#128667 = EDGE_CURVE ( 'NONE', #29752, #12644, #119306, .T. ) ;
#128668 = VERTEX_POINT ( 'NONE', #78770 ) ;
#128669 = ORIENTED_EDGE ( 'NONE', *, *, #78524, .T. ) ;
#128670 = EDGE_LOOP ( 'NONE', ( #68526, #34813 ) ) ;
#128671 = CIRCLE ( 'NONE', #82689, 0.06509327318403745899 ) ;
#128672 = VERTEX_POINT ( 'NONE', #38185 ) ;
#128673 = ORIENTED_EDGE ( 'NONE', *, *, #45469, .T. ) ;
#128674 = CARTESIAN_POINT ( 'NONE',  ( 9.999999999999952038, 2.500000000000000000, 0.09999999999999772959 ) ) ;
#128675 = FACE_OUTER_BOUND ( 'NONE', #79021, .T. ) ;
#128676 = ORIENTED_EDGE ( 'NONE', *, *, #58885, .T. ) ;
#128677 = ADVANCED_FACE ( 'NONE', ( #168 ), #28287, .T. ) ;
#128678 = FACE_BOUND ( 'NONE', #5864, .T. ) ;
#128679 = AXIS2_PLACEMENT_3D ( 'NONE', #104062, #74601, #3921 ) ;
#128680 = ADVANCED_FACE ( 'NONE', ( #118022 ), #101440, .T. ) ;
#128681 = FACE_OUTER_BOUND ( 'NONE', #47861, .T. ) ;
#128682 = CONICAL_SURFACE ( 'NONE', #53350, 0.1000000000000000472, 0.003490658503988666988 ) ;
#128683 = DIRECTION ( 'NONE',  ( 0.000000000000000000, 0.000000000000000000, 1.000000000000000000 ) ) ;
#128684 = AXIS2_PLACEMENT_3D ( 'NONE', #72239, #11365, #93166 ) ;
#128685 = DIRECTION ( 'NONE',  ( 0.000000000000000000, 0.000000000000000000, 1.000000000000000000 ) ) ;
#128686 = DIRECTION ( 'NONE',  ( 0.000000000000000000, 0.000000000000000000, 1.000000000000000000 ) ) ;
#128687 = CARTESIAN_POINT ( 'NONE',  ( 12.49999999999993605, 2.500000000000000000, 0.09999999999999772959 ) ) ;
#128688 = ORIENTED_EDGE ( 'NONE', *, *, #31536, .F. ) ;
#128689 = AXIS2_PLACEMENT_3D ( 'NONE', #44034, #93138, #54480 ) ;
#128690 = ORIENTED_EDGE ( 'NONE', *, *, #34551, .F. ) ;
#128691 = AXIS2_PLACEMENT_3D ( 'NONE', #12261, #41757, #63305 ) ;
#128692 = AXIS2_PLACEMENT_3D ( 'NONE', #85241, #6019, #34877 ) ;
#128693 = VERTEX_POINT ( 'NONE', #57170 ) ;
#128694 = ORIENTED_EDGE ( 'NONE', *, *, #92352, .F. ) ;
#128695 = CARTESIAN_POINT ( 'NONE',  ( 12.04999999999990479, 2.500000000000000000, -6.395190528383301931 ) ) ;
#128696 = VECTOR ( 'NONE', #84133, 1000.000000000000000 ) ;
#128697 = CARTESIAN_POINT ( 'NONE',  ( 6.049999999999935874, 12.50000000000000000, -6.841600689897077814 ) ) ;
#128698 = DIRECTION ( 'NONE',  ( 0.000000000000000000, 0.000000000000000000, 1.000000000000000000 ) ) ;
#128699 = ORIENTED_EDGE ( 'NONE', *, *, #103761, .T. ) ;
#128700 = DIRECTION ( 'NONE',  ( 0.000000000000000000, 0.000000000000000000, 1.000000000000000000 ) ) ;
#128701 = AXIS2_PLACEMENT_3D ( 'NONE', #31180, #129390, #1049 ) ;
#128702 = CIRCLE ( 'NONE', #88961, 0.06509327318403745899 ) ;
#128703 = FACE_OUTER_BOUND ( 'NONE', #16746, .T. ) ;
#128704 = AXIS2_PLACEMENT_3D ( 'NONE', #62371, #22456, #14523 ) ;
#128705 = DIRECTION ( 'NONE',  ( 0.000000000000000000, 0.000000000000000000, 1.000000000000000000 ) ) ;
#128706 = CARTESIAN_POINT ( 'NONE',  ( 184.8177083336747160, 4.367472073101515306, 7.564683531250000925 ) ) ;
#128707 = DIRECTION ( 'NONE',  ( -0.000000000000000000, -1.000000000000000000, -0.000000000000000000 ) ) ;
#128709 = VECTOR ( 'NONE', #37461, 1000.000000000000000 ) ;
#128708 = DIRECTION ( 'NONE',  ( -4.274815082592931898E-19, -0.9999939076577903929, -0.003490651415223739937 ) ) ;
#128710 = DIRECTION ( 'NONE',  ( 0.000000000000000000, 0.000000000000000000, 1.000000000000000000 ) ) ;
#128711 = ORIENTED_EDGE ( 'NONE', *, *, #98321, .F. ) ;
#128712 = FACE_OUTER_BOUND ( 'NONE', #23204, .T. ) ;
#128713 = ORIENTED_EDGE ( 'NONE', *, *, #100673, .T. ) ;
#128714 = EDGE_CURVE ( 'NONE', #14057, #127872, #95182, .T. ) ;
#128715 = VERTEX_POINT ( 'NONE', #19839 ) ;
#128716 = PLANE ( 'NONE',  #109516 ) ;
#128717 = EDGE_CURVE ( 'NONE', #4956, #117143, #116102, .T. ) ;
#128718 = CARTESIAN_POINT ( 'NONE',  ( 2.899999999999944844, 12.50000000000000000, 5.088040615133786027 ) ) ;
#128719 = DIRECTION ( 'NONE',  ( 0.000000000000000000, 0.000000000000000000, 1.000000000000000000 ) ) ;
#128720 = CIRCLE ( 'NONE', #107754, 0.06509327318403741736 ) ;
#128721 = EDGE_LOOP ( 'NONE', ( #3826, #34119, #12043, #31449 ) ) ;
#128722 = VERTEX_POINT ( 'NONE', #118665 ) ;
#128723 = CARTESIAN_POINT ( 'NONE',  ( -7.500000000000016875, 2.500000000000000000, 0.6928203230275494784 ) ) ;
#128724 = DIRECTION ( 'NONE',  ( -0.000000000000000000, 1.000000000000000000, -0.000000000000000000 ) ) ;
#128725 = DIRECTION ( 'NONE',  ( 0.000000000000000000, -0.9999939076577903929, 0.003490651415223739937 ) ) ;
#128726 = ORIENTED_EDGE ( 'NONE', *, *, #60362, .T. ) ;
#128727 = CARTESIAN_POINT ( 'NONE',  ( 4.199999999999938005, 2.500000000000000000, 4.230127018922196669 ) ) ;
#128728 = CIRCLE ( 'NONE', #38840, 0.1000000000000000472 ) ;
#128729 = ORIENTED_EDGE ( 'NONE', *, *, #15820, .F. ) ;
#128731 = CIRCLE ( 'NONE', #20045, 0.06509327318403745899 ) ;
#128730 = DIRECTION ( 'NONE',  ( -0.000000000000000000, 1.000000000000000000, -0.000000000000000000 ) ) ;
#128732 = ORIENTED_EDGE ( 'NONE', *, *, #21194, .T. ) ;
#128733 = CARTESIAN_POINT ( 'NONE',  ( -9.350000000000006750, 12.50000000000000000, 2.511473670974873507 ) ) ;
#128734 = CARTESIAN_POINT ( 'NONE',  ( 0.3999999999999568345, 12.50000000000000000, -3.702399969078687292 ) ) ;
#128735 = DIRECTION ( 'NONE',  ( 0.000000000000000000, 0.000000000000000000, 1.000000000000000000 ) ) ;
#128736 = CARTESIAN_POINT ( 'NONE',  ( -9.600000000000008527, 2.500000000000000000, -5.022947341949749678 ) ) ;
#128737 = EDGE_LOOP ( 'NONE', ( #27019, #9034 ) ) ;
#128738 = AXIS2_PLACEMENT_3D ( 'NONE', #56308, #127004, #77252 ) ;
#128739 = DIRECTION ( 'NONE',  ( -0.000000000000000000, 1.000000000000000000, -0.000000000000000000 ) ) ;
#128740 = CIRCLE ( 'NONE', #72285, 0.1000000000000000472 ) ;
#128741 = VERTEX_POINT ( 'NONE', #129169 ) ;
#128742 = ORIENTED_EDGE ( 'NONE', *, *, #4797, .F. ) ;
#128743 = DIRECTION ( 'NONE',  ( 0.000000000000000000, 0.000000000000000000, 1.000000000000000000 ) ) ;
#128744 = FACE_OUTER_BOUND ( 'NONE', #97070, .T. ) ;
#128745 = FACE_OUTER_BOUND ( 'NONE', #58875, .T. ) ;
#128746 = CARTESIAN_POINT ( 'NONE',  ( 11.89999999999990798, 2.500000000000000000, 4.776537180435972196 ) ) ;
#128747 = CARTESIAN_POINT ( 'NONE',  ( -6.250000000000019540, 2.500000000000000000, -7.088010851410853519 ) ) ;
#128748 = DIRECTION ( 'NONE',  ( 0.000000000000000000, 0.000000000000000000, 1.000000000000000000 ) ) ;
#128749 = EDGE_CURVE ( 'NONE', #118039, #36428, #80613, .T. ) ;
#128750 = CIRCLE ( 'NONE', #53418, 0.09999999999999982514 ) ;
#128751 = CONICAL_SURFACE ( 'NONE', #95273, 0.1000000000000002554, 0.003490658503988666988 ) ;
#128752 = FACE_OUTER_BOUND ( 'NONE', #114335, .T. ) ;
#128753 = CARTESIAN_POINT ( 'NONE',  ( -0.2000000000000412836, 12.50000000000000000, 4.676537180435972552 ) ) ;
#128754 = CARTESIAN_POINT ( 'NONE',  ( 1.849999999999949019, 2.500000000000000000, 6.841600689897072485 ) ) ;
#128755 = ADVANCED_FACE ( 'NONE', ( #109499 ), #45015, .T. ) ;
#128756 = VERTEX_POINT ( 'NONE', #40119 ) ;
#128757 = DIRECTION ( 'NONE',  ( 0.000000000000000000, -0.000000000000000000, 1.000000000000000000 ) ) ;
#128758 = EDGE_CURVE ( 'NONE', #8842, #45024, #1178, .T. ) ;
#128759 = DIRECTION ( 'NONE',  ( 0.000000000000000000, 1.000000000000000000, 0.000000000000000000 ) ) ;
#128761 = EDGE_CURVE ( 'NONE', #92171, #57040, #91065, .T. ) ;
#128760 = DIRECTION ( 'NONE',  ( 0.000000000000000000, 0.000000000000000000, -1.000000000000000000 ) ) ;
#128762 = CARTESIAN_POINT ( 'NONE',  ( 2.099999999999947686, 2.500000000000000000, 5.022947341949748790 ) ) ;
#128763 = DIRECTION ( 'NONE',  ( 0.000000000000000000, 0.000000000000000000, 1.000000000000000000 ) ) ;
#128764 = EDGE_LOOP ( 'NONE', ( #44471, #119545, #71517, #33322 ) ) ;
#128765 = CARTESIAN_POINT ( 'NONE',  ( -11.05000000000000071, 12.50000000000000000, -6.776507416713037912 ) ) ;
#128766 = AXIS2_PLACEMENT_3D ( 'NONE', #83429, #123342, #107570 ) ;
#128767 = CIRCLE ( 'NONE', #93244, 0.1000000000000002554 ) ;
#128768 = CARTESIAN_POINT ( 'NONE',  ( 6.249999999999930722, 12.50000000000000000, 7.122917578226811486 ) ) ;
#128770 = ORIENTED_EDGE ( 'NONE', *, *, #27216, .T. ) ;
#128769 = CARTESIAN_POINT ( 'NONE',  ( -2.900000000000029221, 2.500000000000000000, -0.7928203230275542301 ) ) ;
#128771 = ADVANCED_FACE ( 'NONE', ( #10011 ), #36702, .T. ) ;
#128772 = ORIENTED_EDGE ( 'NONE', *, *, #45253, .T. ) ;
#128773 = CARTESIAN_POINT ( 'NONE',  ( 14.34999999999989662, 2.500000000000000000, 1.818653347947321475 ) ) ;
#128774 = ORIENTED_EDGE ( 'NONE', *, *, #102033, .T. ) ;
#128775 = ORIENTED_EDGE ( 'NONE', *, *, #22980, .T. ) ;
#128776 = ORIENTED_EDGE ( 'NONE', *, *, #75812, .T. ) ;
#128777 = DIRECTION ( 'NONE',  ( -0.000000000000000000, -1.000000000000000000, -0.000000000000000000 ) ) ;
#128778 = AXIS2_PLACEMENT_3D ( 'NONE', #60513, #263, #69662 ) ;
#128779 = DIRECTION ( 'NONE',  ( -0.000000000000000000, -1.000000000000000000, -0.000000000000000000 ) ) ;
#128780 = DIRECTION ( 'NONE',  ( 0.000000000000000000, -0.000000000000000000, 1.000000000000000000 ) ) ;
#128781 = AXIS2_PLACEMENT_3D ( 'NONE', #81410, #109571, #51314 ) ;
#128782 = DIRECTION ( 'NONE',  ( 0.000000000000000000, -0.9999939076577903929, 0.003490651415223739937 ) ) ;
#128783 = AXIS2_PLACEMENT_3D ( 'NONE', #89061, #87750, #22 ) ;
#128784 = ORIENTED_EDGE ( 'NONE', *, *, #50168, .T. ) ;
#128785 = AXIS2_PLACEMENT_3D ( 'NONE', #16455, #96309, #86496 ) ;
#128787 = AXIS2_PLACEMENT_3D ( 'NONE', #87666, #9120, #37938 ) ;
#128786 = DIRECTION ( 'NONE',  ( 0.000000000000000000, 1.000000000000000000, 0.000000000000000000 ) ) ;
#128788 = VERTEX_POINT ( 'NONE', #97100 ) ;
#128789 = CARTESIAN_POINT ( 'NONE',  ( -2.500000000000032863, 12.50000000000000000, 5.022947341949748790 ) ) ;
#128790 = CARTESIAN_POINT ( 'NONE',  ( 18.37149739118984471, -2.540880845001673105, -2.596776292463405245 ) ) ;
#128791 = CARTESIAN_POINT ( 'NONE',  ( 16.58100817950494843, 2.557139044001653261, 6.067820687733449958 ) ) ;
#128792 = DIRECTION ( 'NONE',  ( 0.000000000000000000, 0.000000000000000000, -1.000000000000000000 ) ) ;
#128793 = CARTESIAN_POINT ( 'NONE',  ( 3.549999999999943867, 2.500000000000000000, -1.818653347947326138 ) ) ;
#128794 = VERTEX_POINT ( 'NONE', #30959 ) ;
#128795 = EDGE_CURVE ( 'NONE', #110378, #117106, #75395, .T. ) ;
#128796 = EDGE_LOOP ( 'NONE', ( #128563, #2347, #12991, #110244 ) ) ;
#128797 = EDGE_LOOP ( 'NONE', ( #51414, #25883 ) ) ;
#128798 = ORIENTED_EDGE ( 'NONE', *, *, #72385, .F. ) ;
#128799 = ORIENTED_EDGE ( 'NONE', *, *, #63764, .T. ) ;
#128800 = DIRECTION ( 'NONE',  ( 0.000000000000000000, 1.000000000000000000, 0.000000000000000000 ) ) ;
#128801 = DIRECTION ( 'NONE',  ( 0.000000000000000000, 0.000000000000000000, -1.000000000000000000 ) ) ;
#128802 = CARTESIAN_POINT ( 'NONE',  ( -7.500000000000015099, 2.500000000000000000, -4.922947341949753586 ) ) ;
#128803 = EDGE_CURVE ( 'NONE', #39135, #384, #32893, .T. ) ;
#128804 = FACE_BOUND ( 'NONE', #12895, .T. ) ;
#128805 = DIRECTION ( 'NONE',  ( 0.000000000000000000, 1.000000000000000000, 0.000000000000000000 ) ) ;
#128806 = AXIS2_PLACEMENT_3D ( 'NONE', #16890, #104651, #35298 ) ;
#128807 = DIRECTION ( 'NONE',  ( -0.000000000000000000, -1.000000000000000000, -0.000000000000000000 ) ) ;
#128808 = ADVANCED_FACE ( 'NONE', ( #30317 ), #118158, .T. ) ;
#128809 = DIRECTION ( 'NONE',  ( 0.000000000000000000, 0.000000000000000000, -1.000000000000000000 ) ) ;
#128810 = DIRECTION ( 'NONE',  ( 0.000000000000000000, 1.000000000000000000, 0.000000000000000000 ) ) ;
#128811 = EDGE_CURVE ( 'NONE', #28513, #17110, #110777, .T. ) ;
#128812 = CARTESIAN_POINT ( 'NONE',  ( 10.84999999999990905, 12.50000000000000000, -6.560283801567339701 ) ) ;
#128813 = EDGE_CURVE ( 'NONE', #127159, #109486, #62346, .T. ) ;
#128814 = CONICAL_SURFACE ( 'NONE', #1330, 0.1000000000000002554, 0.003490658503988666988 ) ;
#128815 = DIRECTION ( 'NONE',  ( -0.000000000000000000, 1.000000000000000000, -0.000000000000000000 ) ) ;
#128816 = ADVANCED_FACE ( 'NONE', ( #21111 ), #70224, .T. ) ;
#128817 = DIRECTION ( 'NONE',  ( -0.000000000000000000, 1.000000000000000000, -0.000000000000000000 ) ) ;
#128818 = AXIS2_PLACEMENT_3D ( 'NONE', #74868, #114774, #25111 ) ;
#128819 = ADVANCED_FACE ( 'NONE', ( #92432 ), #41425, .T. ) ;
#128820 = AXIS2_PLACEMENT_3D ( 'NONE', #3546, #43487, #81472 ) ;
#128821 = CARTESIAN_POINT ( 'NONE',  ( 4.149999999999941735, 12.50000000000000000, -1.472243186433550122 ) ) ;
#128822 = CONICAL_SURFACE ( 'NONE', #80680, 0.1000000000000002554, 0.003490658503988666988 ) ;
#128823 = ADVANCED_FACE ( 'NONE', ( #120609 ), #82768, .T. ) ;
#128824 = ORIENTED_EDGE ( 'NONE', *, *, #4, .T. ) ;
#128825 = ORIENTED_EDGE ( 'NONE', *, *, #67455, .T. ) ;
#128826 = ORIENTED_EDGE ( 'NONE', *, *, #87183, .F. ) ;
#128827 = ORIENTED_EDGE ( 'NONE', *, *, #103073, .T. ) ;
#128828 = DIRECTION ( 'NONE',  ( 0.000000000000000000, 0.000000000000000000, 1.000000000000000000 ) ) ;
#128829 = DIRECTION ( 'NONE',  ( -0.000000000000000000, 1.000000000000000000, -0.000000000000000000 ) ) ;
#128830 = FACE_BOUND ( 'NONE', #47527, .T. ) ;
#128831 = ADVANCED_FACE ( 'NONE', ( #91794 ), #9594, .T. ) ;
#128833 = CARTESIAN_POINT ( 'NONE',  ( 10.19999999999991225, 2.500000000000000000, -4.776537180435978414 ) ) ;
#128832 = AXIS2_PLACEMENT_3D ( 'NONE', #48285, #88175, #78407 ) ;
#128835 = VECTOR ( 'NONE', #10623, 1000.000000000000000 ) ;
#128834 = CIRCLE ( 'NONE', #95355, 0.1000000000000000472 ) ;
#128836 = EDGE_LOOP ( 'NONE', ( #62443, #82864 ) ) ;
#128837 = DIRECTION ( 'NONE',  ( 0.000000000000000000, 0.000000000000000000, 1.000000000000000000 ) ) ;
#128838 = DIRECTION ( 'NONE',  ( -4.274815082592931898E-19, -0.9999939076577903929, -0.003490651415223739937 ) ) ;
#128839 = CARTESIAN_POINT ( 'NONE',  ( -0.6500000000000394351, 12.50000000000000000, 6.841600689897072485 ) ) ;
#128840 = DIRECTION ( 'NONE',  ( 0.000000000000000000, 0.000000000000000000, -1.000000000000000000 ) ) ;
#128841 = DIRECTION ( 'NONE',  ( 0.000000000000000000, -0.000000000000000000, 1.000000000000000000 ) ) ;
#128842 = VERTEX_POINT ( 'NONE', #121254 ) ;
#128843 = CARTESIAN_POINT ( 'NONE',  ( 6.849999999999927702, 2.500000000000000000, 2.511473670974873507 ) ) ;
#128844 = VERTEX_POINT ( 'NONE', #11289 ) ;
#128845 = ORIENTED_EDGE ( 'NONE', *, *, #73747, .F. ) ;
#128846 = CARTESIAN_POINT ( 'NONE',  ( 9.599999999999914380, 2.500000000000000000, -5.022947341949754119 ) ) ;
#128847 = CARTESIAN_POINT ( 'NONE',  ( 179.5000000000000000, -0.6250000000000025535, -6.000000000000000888 ) ) ;
#128848 = ORIENTED_EDGE ( 'NONE', *, *, #28583, .F. ) ;
#128849 = DIRECTION ( 'NONE',  ( 0.000000000000000000, 0.000000000000000000, -1.000000000000000000 ) ) ;
#128850 = CARTESIAN_POINT ( 'NONE',  ( 2.099999999999949463, 12.50000000000000000, 0.7579135962115869374 ) ) ;
#128851 = EDGE_LOOP ( 'NONE', ( #10842, #101063 ) ) ;
#128852 = DIRECTION ( 'NONE',  ( -0.000000000000000000, -1.000000000000000000, -0.000000000000000000 ) ) ;
#128853 = ORIENTED_EDGE ( 'NONE', *, *, #53719, .T. ) ;
#128854 = DIRECTION ( 'NONE',  ( 0.000000000000000000, 1.000000000000000000, 0.000000000000000000 ) ) ;
#128855 = ORIENTED_EDGE ( 'NONE', *, *, #126795, .F. ) ;
#128856 = DIRECTION ( 'NONE',  ( 0.000000000000000000, -0.000000000000000000, 1.000000000000000000 ) ) ;
#128857 = FACE_BOUND ( 'NONE', #106640, .T. ) ;
#128858 = AXIS2_PLACEMENT_3D ( 'NONE', #13871, #4051, #44001 ) ;
#128859 = ORIENTED_EDGE ( 'NONE', *, *, #6973, .T. ) ;
#128860 = EDGE_CURVE ( 'NONE', #16485, #59989, #28381, .T. ) ;
#128861 = CARTESIAN_POINT ( 'NONE',  ( 108.1697673669222581, 5.855766388782916110, 5.000000000000030198 ) ) ;
#128862 = EDGE_LOOP ( 'NONE', ( #13314, #121822 ) ) ;
#128863 = LINE ( 'NONE', #21452, #65930 ) ;
#128864 = DIRECTION ( 'NONE',  ( 0.000000000000000000, 0.000000000000000000, 1.000000000000000000 ) ) ;
#128865 = FACE_OUTER_BOUND ( 'NONE', #46862, .T. ) ;
#128866 = CARTESIAN_POINT ( 'NONE',  ( -8.300000000000009592, 2.500000000000000000, 4.430127018922196847 ) ) ;
#128867 = DIRECTION ( 'NONE',  ( 0.000000000000000000, 1.000000000000000000, 0.000000000000000000 ) ) ;
#128868 = EDGE_LOOP ( 'NONE', ( #120402, #96814, #12455, #10062 ) ) ;
#128871 = VERTEX_POINT ( 'NONE', #1466 ) ;
#128870 = CIRCLE ( 'NONE', #61948, 0.06509327318403745899 ) ;
#128869 = AXIS2_PLACEMENT_3D ( 'NONE', #2040, #60966, #121179 ) ;
#128872 = EDGE_CURVE ( 'NONE', #2945, #88713, #116182, .T. ) ;
#128873 = ORIENTED_EDGE ( 'NONE', *, *, #5355, .F. ) ;
#128874 = CARTESIAN_POINT ( 'NONE',  ( 8.149999999999920419, 12.50000000000000000, 6.148780366869520897 ) ) ;
#128875 = DIRECTION ( 'NONE',  ( 0.000000000000000000, 0.000000000000000000, 1.000000000000000000 ) ) ;
#128876 = DIRECTION ( 'NONE',  ( -0.000000000000000000, 1.000000000000000000, -0.000000000000000000 ) ) ;
#128878 = VERTEX_POINT ( 'NONE', #71501 ) ;
#128877 = EDGE_LOOP ( 'NONE', ( #138, #99904, #64537, #119606 ) ) ;
#128879 = ORIENTED_EDGE ( 'NONE', *, *, #112106, .F. ) ;
#128880 = CARTESIAN_POINT ( 'NONE',  ( -12.69999999999999218, 12.50000000000000000, -4.676537180435975216 ) ) ;
#128881 = CONICAL_SURFACE ( 'NONE', #116221, 0.1000000000000000472, 0.003490658503988666988 ) ;
#128882 = DIRECTION ( 'NONE',  ( 0.000000000000000000, 0.000000000000000000, 1.000000000000000000 ) ) ;
#128883 = AXIS2_PLACEMENT_3D ( 'NONE', #86335, #106629, #77176 ) ;
#128884 = DIRECTION ( 'NONE',  ( 0.000000000000000000, 0.000000000000000000, -1.000000000000000000 ) ) ;
#128885 = DIRECTION ( 'NONE',  ( 0.000000000000000000, 0.000000000000000000, 1.000000000000000000 ) ) ;
#128886 = DIRECTION ( 'NONE',  ( -0.000000000000000000, 1.000000000000000000, -0.000000000000000000 ) ) ;
#128887 = CARTESIAN_POINT ( 'NONE',  ( 1.649999999999951505, 2.500000000000000000, -2.857883832488653741 ) ) ;
#128888 = DIRECTION ( 'NONE',  ( 0.000000000000000000, 0.000000000000000000, 1.000000000000000000 ) ) ;
#128889 = LINE ( 'NONE', #18255, #129415 ) ;
#128890 = ORIENTED_EDGE ( 'NONE', *, *, #48222, .T. ) ;
#128891 = ORIENTED_EDGE ( 'NONE', *, *, #87419, .T. ) ;
#128892 = DIRECTION ( 'NONE',  ( -0.000000000000000000, 1.000000000000000000, -0.000000000000000000 ) ) ;
#128893 = DIRECTION ( 'NONE',  ( -0.000000000000000000, 1.000000000000000000, -0.000000000000000000 ) ) ;
#128894 = ORIENTED_EDGE ( 'NONE', *, *, #79004, .T. ) ;
#128895 = VERTEX_POINT ( 'NONE', #42055 ) ;
#128896 = CARTESIAN_POINT ( 'NONE',  ( -9.150000000000005684, 12.50000000000000000, 5.802370205355744659 ) ) ;
#128897 = DIRECTION ( 'NONE',  ( 0.000000000000000000, 1.000000000000000000, 0.000000000000000000 ) ) ;
#128898 = AXIS2_PLACEMENT_3D ( 'NONE', #129496, #79721, #90159 ) ;
#128899 = CARTESIAN_POINT ( 'NONE',  ( 3.749999999999940492, 2.500000000000000000, 2.957883832488649389 ) ) ;
#128900 = DIRECTION ( 'NONE',  ( 0.000000000000000000, 0.000000000000000000, -1.000000000000000000 ) ) ;
#128901 = EDGE_CURVE ( 'NONE', #106998, #24838, #111414, .T. ) ;
#128902 = DIRECTION ( 'NONE',  ( 0.000000000000000000, -0.9999939076577903929, 0.003490651415223739937 ) ) ;
#128903 = CIRCLE ( 'NONE', #53656, 0.1000000000000000472 ) ;
#128904 = LINE ( 'NONE', #120991, #69907 ) ;
#128905 = DIRECTION ( 'NONE',  ( 0.000000000000000000, 0.000000000000000000, 1.000000000000000000 ) ) ;
#128906 = CONICAL_SURFACE ( 'NONE', #59862, 0.1000000000000002554, 0.003490658503988666988 ) ;
#128907 = CIRCLE ( 'NONE', #72449, 0.1000000000000002554 ) ;
#128908 = AXIS2_PLACEMENT_3D ( 'NONE', #58463, #19820, #28350 ) ;
#128909 = CARTESIAN_POINT ( 'NONE',  ( -0.4000000000000401013, 12.50000000000000000, -3.637306695894650055 ) ) ;
#128910 = EDGE_CURVE ( 'NONE', #129385, #98295, #61705, .T. ) ;
#128911 = EDGE_LOOP ( 'NONE', ( #98741, #20546 ) ) ;
#128912 = AXIS2_PLACEMENT_3D ( 'NONE', #129100, #66910, #77394 ) ;
#128913 = ORIENTED_EDGE ( 'NONE', *, *, #78247, .F. ) ;
#128914 = ADVANCED_FACE ( 'NONE', ( #51878 ), #76496, .T. ) ;
#128915 = ORIENTED_EDGE ( 'NONE', *, *, #100524, .F. ) ;
#128916 = ORIENTED_EDGE ( 'NONE', *, *, #66593, .T. ) ;
#128917 = EDGE_CURVE ( 'NONE', #54589, #24400, #101535, .T. ) ;
#128918 = DIRECTION ( 'NONE',  ( -4.274815082592931898E-19, -0.9999939076577903929, -0.003490651415223739937 ) ) ;
#128919 = FACE_OUTER_BOUND ( 'NONE', #63410, .T. ) ;
#128920 = CIRCLE ( 'NONE', #93388, 0.06509327318403745899 ) ;
#128921 = ORIENTED_EDGE ( 'NONE', *, *, #101024, .T. ) ;
#128922 = DIRECTION ( 'NONE',  ( 0.000000000000000000, 0.000000000000000000, -1.000000000000000000 ) ) ;
#128923 = CARTESIAN_POINT ( 'NONE',  ( 0.6499999999999561684, 2.500000000000000000, 1.718653347947321386 ) ) ;
#128925 = CONICAL_SURFACE ( 'NONE', #78738, 0.1000000000000002554, 0.003490658503988666988 ) ;
#128924 = CIRCLE ( 'NONE', #97499, 0.1000000000000000472 ) ;
#128926 = ADVANCED_FACE ( 'NONE', ( #43353 ), #5333, .T. ) ;
#128927 = CARTESIAN_POINT ( 'NONE',  ( -6.850000000000013856, 12.50000000000000000, 6.148780366869520897 ) ) ;
#128929 = ORIENTED_EDGE ( 'NONE', *, *, #7205, .T. ) ;
#128928 = CARTESIAN_POINT ( 'NONE',  ( -12.09999999999999609, 2.500000000000000000, -4.230127018922199333 ) ) ;
#128930 = EDGE_CURVE ( 'NONE', #70003, #527, #103689, .T. ) ;
#128931 = DIRECTION ( 'NONE',  ( 0.000000000000000000, 1.000000000000000000, 0.000000000000000000 ) ) ;
#128932 = CARTESIAN_POINT ( 'NONE',  ( 4.999999999999973355, 2.500000000000000000, -4.330127018922201643 ) ) ;
#128933 = ORIENTED_EDGE ( 'NONE', *, *, #24452, .T. ) ;
#128934 = EDGE_LOOP ( 'NONE', ( #43152, #48373 ) ) ;
#128935 = ORIENTED_EDGE ( 'NONE', *, *, #230, .F. ) ;
#128936 = VERTEX_POINT ( 'NONE', #23699 ) ;
#128937 = CARTESIAN_POINT ( 'NONE',  ( -8.150000000000014566, 2.500000000000000000, -6.048780366869521252 ) ) ;
#128938 = PLANE ( 'NONE',  #32018 ) ;
#128939 = PLANE ( 'NONE',  #62865 ) ;
#128940 = ORIENTED_EDGE ( 'NONE', *, *, #42036, .F. ) ;
#128941 = FACE_OUTER_BOUND ( 'NONE', #9615, .T. ) ;
#128942 = CARTESIAN_POINT ( 'NONE',  ( 6.049999999999930544, 2.500000000000000000, 2.511473670974873507 ) ) ;
#128943 = FACE_OUTER_BOUND ( 'NONE', #30216, .T. ) ;
#128944 = DIRECTION ( 'NONE',  ( -0.000000000000000000, 1.000000000000000000, -0.000000000000000000 ) ) ;
#128945 = ORIENTED_EDGE ( 'NONE', *, *, #96960, .F. ) ;
#128946 = AXIS2_PLACEMENT_3D ( 'NONE', #11787, #51093, #72017 ) ;
#128947 = DIRECTION ( 'NONE',  ( 0.000000000000000000, -0.9999939076577903929, 0.003490651415223739937 ) ) ;
#128948 = AXIS2_PLACEMENT_3D ( 'NONE', #107322, #57593, #97504 ) ;
#128949 = ORIENTED_EDGE ( 'NONE', *, *, #126600, .F. ) ;
#128950 = ORIENTED_EDGE ( 'NONE', *, *, #85932, .F. ) ;
#128951 = DIRECTION ( 'NONE',  ( 0.000000000000000000, -0.000000000000000000, 1.000000000000000000 ) ) ;
#128952 = DIRECTION ( 'NONE',  ( 0.000000000000000000, 1.000000000000000000, 0.000000000000000000 ) ) ;
#128953 = FACE_BOUND ( 'NONE', #15829, .T. ) ;
#128954 = DIRECTION ( 'NONE',  ( -4.274815082592931898E-19, -0.9999939076577903929, -0.003490651415223739937 ) ) ;
#128955 = FACE_OUTER_BOUND ( 'NONE', #114194, .T. ) ;
#128957 = CONICAL_SURFACE ( 'NONE', #66227, 0.09999999999999982514, 0.003490658503988666988 ) ;
#128956 = AXIS2_PLACEMENT_3D ( 'NONE', #116506, #87043, #126985 ) ;
#128958 = CARTESIAN_POINT ( 'NONE',  ( 8.349999999999923261, 12.50000000000000000, -7.188010851410854052 ) ) ;
#128959 = EDGE_CURVE ( 'NONE', #96953, #83685, #83273, .T. ) ;
#128960 = VERTEX_POINT ( 'NONE', #15137 ) ;
#128961 = EDGE_CURVE ( 'NONE', #18164, #11592, #66019, .T. ) ;
#128962 = DIRECTION ( 'NONE',  ( 0.000000000000000000, 0.000000000000000000, 1.000000000000000000 ) ) ;
#128963 = DIRECTION ( 'NONE',  ( 0.000000000000000000, 0.000000000000000000, -1.000000000000000000 ) ) ;
#128964 = AXIS2_PLACEMENT_3D ( 'NONE', #93733, #94361, #115943 ) ;
#128965 = DIRECTION ( 'NONE',  ( 0.000000000000000000, -0.9999939076577903929, 0.003490651415223739937 ) ) ;
#128966 = EDGE_CURVE ( 'NONE', #116101, #58516, #123198, .T. ) ;
#128967 = CARTESIAN_POINT ( 'NONE',  ( 186.2812500006828031, 0.000000000000000000, 7.700000000000000178 ) ) ;
#128968 = VERTEX_POINT ( 'NONE', #93728 ) ;
#128971 = ADVANCED_FACE ( 'NONE', ( #94358 ), #128751, .T. ) ;
#128970 = CIRCLE ( 'NONE', #57854, 0.06509327318403745899 ) ;
#128969 = CIRCLE ( 'NONE', #16044, 0.06509327318403745899 ) ;
#128972 = DIRECTION ( 'NONE',  ( -4.274815082592931898E-19, -0.9999939076577903929, -0.003490651415223739937 ) ) ;
#128973 = AXIS2_PLACEMENT_3D ( 'NONE', #61847, #42868, #82779 ) ;
#128974 = CARTESIAN_POINT ( 'NONE',  ( -8.150000000000012790, 2.500000000000000000, -2.511473670974877948 ) ) ;
#128975 = EDGE_CURVE ( 'NONE', #12077, #79693, #65550, .T. ) ;
#128976 = VERTEX_POINT ( 'NONE', #5969 ) ;
#128977 = VERTEX_POINT ( 'NONE', #124480 ) ;
#128978 = CARTESIAN_POINT ( 'NONE',  ( -11.89999999999999503, 2.500000000000000000, 4.676537180435972552 ) ) ;
#128979 = CARTESIAN_POINT ( 'NONE',  ( 127.5000000000000000, -1.500000000000000000, 2.598076211353316900 ) ) ;
#128980 = FACE_BOUND ( 'NONE', #22373, .T. ) ;
#128981 = DIRECTION ( 'NONE',  ( 0.000000000000000000, 1.000000000000000000, 0.000000000000000000 ) ) ;
#128982 = EDGE_CURVE ( 'NONE', #92222, #72461, #41014, .T. ) ;
#128983 = EDGE_CURVE ( 'NONE', #30750, #8254, #15840, .T. ) ;
#128984 = DIRECTION ( 'NONE',  ( 0.000000000000000000, -0.9999939076577903929, 0.003490651415223739937 ) ) ;
#128985 = ORIENTED_EDGE ( 'NONE', *, *, #127668, .T. ) ;
#128986 = FACE_OUTER_BOUND ( 'NONE', #82402, .T. ) ;
#128987 = CARTESIAN_POINT ( 'NONE',  ( 184.8333333333333144, 6.668395609140177704, -3.849999999999998312 ) ) ;
#128988 = AXIS2_PLACEMENT_3D ( 'NONE', #78939, #69746, #8237 ) ;
#128990 = EDGE_CURVE ( 'NONE', #30644, #3252, #32608, .T. ) ;
#128989 = AXIS2_PLACEMENT_3D ( 'NONE', #117861, #128367, #9860 ) ;
#128991 = VERTEX_POINT ( 'NONE', #85823 ) ;
#128992 = DIRECTION ( 'NONE',  ( 0.000000000000000000, -0.9999939076577903929, 0.003490651415223739937 ) ) ;
#128993 = CIRCLE ( 'NONE', #72545, 8.699999999999999289 ) ;
#128994 = FACE_OUTER_BOUND ( 'NONE', #28264, .T. ) ;
#128995 = CONICAL_SURFACE ( 'NONE', #66263, 0.1000000000000000472, 0.003490658503988666988 ) ;
#128996 = CARTESIAN_POINT ( 'NONE',  ( 6.649999999999930189, 2.500000000000000000, 5.802370205355744659 ) ) ;
#128997 = LINE ( 'NONE', #39329, #78191 ) ;
#128998 = AXIS2_PLACEMENT_3D ( 'NONE', #37061, #78280, #18688 ) ;
#128999 = EDGE_LOOP ( 'NONE', ( #78827, #8125 ) ) ;
#129000 = CIRCLE ( 'NONE', #13945, 0.06509327318403745899 ) ;
#129001 = PRESENTATION_STYLE_ASSIGNMENT (( #38010 ) ) ;
#129002 = DIRECTION ( 'NONE',  ( 0.000000000000000000, -0.000000000000000000, 1.000000000000000000 ) ) ;
#129003 = DIRECTION ( 'NONE',  ( 0.000000000000000000, 1.000000000000000000, 0.000000000000000000 ) ) ;
#129004 = CARTESIAN_POINT ( 'NONE',  ( 7.299999999999926104, 2.500000000000000000, -4.083716857408426826 ) ) ;
#129005 = VERTEX_POINT ( 'NONE', #105482 ) ;
#129006 = ORIENTED_EDGE ( 'NONE', *, *, #94480, .F. ) ;
#129007 = AXIS2_PLACEMENT_3D ( 'NONE', #25463, #106612, #86319 ) ;
#129008 = CARTESIAN_POINT ( 'NONE',  ( 16.98389447545206821, 2.499999999999373390, 5.627887033857345678 ) ) ;
#129009 = AXIS2_PLACEMENT_3D ( 'NONE', #43316, #83235, #73392 ) ;
#129010 = ORIENTED_EDGE ( 'NONE', *, *, #120544, .T. ) ;
#129011 = PLANE ( 'NONE',  #91102 ) ;
#129012 = DIRECTION ( 'NONE',  ( 0.000000000000000000, -0.000000000000000000, 1.000000000000000000 ) ) ;
#129013 = CARTESIAN_POINT ( 'NONE',  ( 1.049999999999952083, 12.50000000000000000, 6.841600689897072485 ) ) ;
#129015 = CONICAL_SURFACE ( 'NONE', #11901, 0.09999999999999982514, 0.003490658503988666988 ) ;
#129014 = CIRCLE ( 'NONE', #82933, 0.1000000000000002554 ) ;
#129016 = CARTESIAN_POINT ( 'NONE',  ( -8.150000000000014566, 2.500000000000000000, -6.741600689897072840 ) ) ;
#129017 = ORIENTED_EDGE ( 'NONE', *, *, #65670, .F. ) ;
#129018 = DIRECTION ( 'NONE',  ( 0.000000000000000000, 0.000000000000000000, -1.000000000000000000 ) ) ;
#129019 = CARTESIAN_POINT ( 'NONE',  ( -3.950000000000026379, 2.500000000000000000, 6.941600689897073018 ) ) ;
#129020 = DIRECTION ( 'NONE',  ( 0.000000000000000000, -0.9999939076577903929, 0.003490651415223739937 ) ) ;
#129021 = CARTESIAN_POINT ( 'NONE',  ( 184.8177083336747160, 4.367472073101515306, 7.564683531250000925 ) ) ;
#129022 = DIRECTION ( 'NONE',  ( 0.000000000000000000, 1.000000000000000000, 0.000000000000000000 ) ) ;
#129023 = DIRECTION ( 'NONE',  ( -0.000000000000000000, -1.000000000000000000, -0.000000000000000000 ) ) ;
#129024 = ORIENTED_EDGE ( 'NONE', *, *, #79971, .T. ) ;
#129025 = ADVANCED_FACE ( 'NONE', ( #95021 ), #74439, .T. ) ;
#129026 = ORIENTED_EDGE ( 'NONE', *, *, #95623, .F. ) ;
#129027 = DIRECTION ( 'NONE',  ( -0.000000000000000000, 1.000000000000000000, -0.000000000000000000 ) ) ;
#129028 = ORIENTED_EDGE ( 'NONE', *, *, #11308, .F. ) ;
#129029 = DIRECTION ( 'NONE',  ( -4.274815082592931898E-19, -0.9999939076577903929, -0.003490651415223739937 ) ) ;
#129031 = ORIENTED_EDGE ( 'NONE', *, *, #109950, .F. ) ;
#129030 = ORIENTED_EDGE ( 'NONE', *, *, #33184, .T. ) ;
#129032 = ORIENTED_EDGE ( 'NONE', *, *, #63273, .F. ) ;
#129033 = CONICAL_SURFACE ( 'NONE', #36973, 0.1000000000000002554, 0.003490658503988666988 ) ;
#129034 = CARTESIAN_POINT ( 'NONE',  ( 11.24999999999994316, 12.50000000000000000, 2.165063509461097713 ) ) ;
#129035 = DIRECTION ( 'NONE',  ( 0.000000000000000000, 1.000000000000000000, 0.000000000000000000 ) ) ;
#129036 = DIRECTION ( 'NONE',  ( -0.000000000000000000, 1.000000000000000000, -0.000000000000000000 ) ) ;
#129037 = FACE_OUTER_BOUND ( 'NONE', #32838, .T. ) ;
#129038 = LINE ( 'NONE', #89727, #81452 ) ;
#129039 = CARTESIAN_POINT ( 'NONE',  ( 179.5000000000000000, 0.6250000000000000000, 7.634788798650556707 ) ) ;
#129040 = DIRECTION ( 'NONE',  ( -0.000000000000000000, -1.000000000000000000, -0.000000000000000000 ) ) ;
#129041 = CARTESIAN_POINT ( 'NONE',  ( 3.549999999999943867, 2.500000000000000000, -6.148780366869526226 ) ) ;
#129042 = ORIENTED_EDGE ( 'NONE', *, *, #63273, .T. ) ;
#129044 = ORIENTED_EDGE ( 'NONE', *, *, #58939, .F. ) ;
#129043 = VECTOR ( 'NONE', #68619, 1000.000000000000000 ) ;
#129045 = CIRCLE ( 'NONE', #108078, 0.06509327318403745899 ) ;
#129046 = DIRECTION ( 'NONE',  ( -0.000000000000000000, 1.000000000000000000, -0.000000000000000000 ) ) ;
#129047 = EDGE_LOOP ( 'NONE', ( #52585, #16791 ) ) ;
#129048 = ORIENTED_EDGE ( 'NONE', *, *, #73101, .T. ) ;
#129049 = DIRECTION ( 'NONE',  ( 0.000000000000000000, 1.000000000000000000, 0.000000000000000000 ) ) ;
#129051 = AXIS2_PLACEMENT_3D ( 'NONE', #2082, #81932, #13186 ) ;
#129050 = CIRCLE ( 'NONE', #3633, 0.06509327318403745899 ) ;
#129052 = CARTESIAN_POINT ( 'NONE',  ( -1.250000000000001110, 2.500000000000000000, -6.495190528383302464 ) ) ;
#129053 = DIRECTION ( 'NONE',  ( 0.000000000000000000, 0.000000000000000000, 1.000000000000000000 ) ) ;
#129054 = CARTESIAN_POINT ( 'NONE',  ( 9.799999999999913669, 2.500000000000000000, 4.776537180435972196 ) ) ;
#129055 = FACE_OUTER_BOUND ( 'NONE', #84531, .T. ) ;
#129056 = ORIENTED_EDGE ( 'NONE', *, *, #45277, .T. ) ;
#129058 = VECTOR ( 'NONE', #70664, 1000.000000000000000 ) ;
#129057 = AXIS2_PLACEMENT_3D ( 'NONE', #68513, #67868, #105390 ) ;
#129059 = VERTEX_POINT ( 'NONE', #15795 ) ;
#129060 = CARTESIAN_POINT ( 'NONE',  ( 8.349999999999923261, 12.50000000000000000, -7.253104124594891289 ) ) ;
#129062 = EDGE_CURVE ( 'NONE', #27571, #942, #3329, .T. ) ;
#129061 = AXIS2_PLACEMENT_3D ( 'NONE', #157, #29638, #19827 ) ;
#129063 = ORIENTED_EDGE ( 'NONE', *, *, #59570, .T. ) ;
#129064 = DIRECTION ( 'NONE',  ( 0.000000000000000000, 0.000000000000000000, 1.000000000000000000 ) ) ;
#129065 = VERTEX_POINT ( 'NONE', #114643 ) ;
#129066 = ADVANCED_FACE ( 'NONE', ( #66187 ), #49327, .T. ) ;
#129067 = ORIENTED_EDGE ( 'NONE', *, *, #68678, .F. ) ;
#129068 = ADVANCED_FACE ( 'NONE', ( #106121 ), #14499, .T. ) ;
#129069 = FACE_OUTER_BOUND ( 'NONE', #73189, .T. ) ;
#129070 = FACE_OUTER_BOUND ( 'NONE', #28331, .T. ) ;
#129071 = AXIS2_PLACEMENT_3D ( 'NONE', #31747, #101775, #13380 ) ;
#129072 = DIRECTION ( 'NONE',  ( -0.000000000000000000, 1.000000000000000000, -0.000000000000000000 ) ) ;
#129073 = CARTESIAN_POINT ( 'NONE',  ( -14.34999999999998543, 2.500000000000000000, -1.918653347947323784 ) ) ;
#129074 = EDGE_CURVE ( 'NONE', #68346, #115529, #26327, .T. ) ;
#129075 = DIRECTION ( 'NONE',  ( 0.000000000000000000, 0.000000000000000000, 1.000000000000000000 ) ) ;
#129077 = ORIENTED_EDGE ( 'NONE', *, *, #96681, .F. ) ;
#129076 = EDGE_CURVE ( 'NONE', #118978, #16932, #7517, .T. ) ;
#129078 = DIRECTION ( 'NONE',  ( 0.000000000000000000, 0.000000000000000000, 1.000000000000000000 ) ) ;
#129079 = CARTESIAN_POINT ( 'NONE',  ( 8.349999999999919709, 12.50000000000000000, 7.122917578226811486 ) ) ;
#129080 = EDGE_CURVE ( 'NONE', #40491, #66554, #39342, .T. ) ;
#129081 = DIRECTION ( 'NONE',  ( 0.000000000000000000, 1.000000000000000000, 0.000000000000000000 ) ) ;
#129082 = EDGE_CURVE ( 'NONE', #46559, #47762, #59798, .T. ) ;
#129083 = EDGE_CURVE ( 'NONE', #98725, #83167, #57720, .T. ) ;
#129084 = CARTESIAN_POINT ( 'NONE',  ( 12.89999999999990088, 2.500000000000000000, -4.230127018922201998 ) ) ;
#129085 = CONICAL_SURFACE ( 'NONE', #72624, 0.09999999999999982514, 0.003490658503988666988 ) ;
#129086 = CIRCLE ( 'NONE', #9924, 0.06509327318403745899 ) ;
#129087 = DIRECTION ( 'NONE',  ( 0.000000000000000000, -0.9999939076577903929, 0.003490651415223739937 ) ) ;
#129088 = ORIENTED_EDGE ( 'NONE', *, *, #33726, .T. ) ;
#129089 = AXIS2_PLACEMENT_3D ( 'NONE', #29743, #69012, #17983 ) ;
#129090 = ORIENTED_EDGE ( 'NONE', *, *, #69895, .T. ) ;
#129091 = FACE_OUTER_BOUND ( 'NONE', #84712, .T. ) ;
#129092 = EDGE_CURVE ( 'NONE', #27226, #41372, #84795, .T. ) ;
#129093 = AXIS2_PLACEMENT_3D ( 'NONE', #53961, #23864, #103046 ) ;
#129094 = ORIENTED_EDGE ( 'NONE', *, *, #50634, .F. ) ;
#129095 = CARTESIAN_POINT ( 'NONE',  ( 17.50000000000000000, -2.499999999999960476, 3.093175630837758483 ) ) ;
#129096 = CYLINDRICAL_SURFACE ( 'NONE', #62691, 7.699999999999999289 ) ;
#129097 = AXIS2_PLACEMENT_3D ( 'NONE', #77234, #37956, #27468 ) ;
#129098 = ORIENTED_EDGE ( 'NONE', *, *, #24648, .F. ) ;
#129099 = DIRECTION ( 'NONE',  ( 0.000000000000000000, 0.000000000000000000, -1.000000000000000000 ) ) ;
#129101 = AXIS2_PLACEMENT_3D ( 'NONE', #18233, #118370, #69925 ) ;
#129100 = CARTESIAN_POINT ( 'NONE',  ( -11.24999999999999822, 2.500000000000000000, 1.472243186433545459 ) ) ;
#129102 = PLANE ( 'NONE',  #98393 ) ;
#129103 = DIRECTION ( 'NONE',  ( 0.000000000000000000, 1.000000000000000000, 0.000000000000000000 ) ) ;
#129104 = VERTEX_POINT ( 'NONE', #57004 ) ;
#129106 = CIRCLE ( 'NONE', #24527, 0.06509327318403745899 ) ;
#129105 = CIRCLE ( 'NONE', #74695, 0.1000000000000002554 ) ;
#129107 = LINE ( 'NONE', #39440, #35260 ) ;
#129108 = ORIENTED_EDGE ( 'NONE', *, *, #108538, .F. ) ;
#129109 = CARTESIAN_POINT ( 'NONE',  ( 8.349999999999919709, 2.500000000000000000, 6.495190528383297135 ) ) ;
#129110 = DIRECTION ( 'NONE',  ( -0.000000000000000000, -1.000000000000000000, -0.000000000000000000 ) ) ;
#129111 = CARTESIAN_POINT ( 'NONE',  ( 2.699999999999947331, 2.500000000000000000, -4.576537180435978236 ) ) ;
#129112 = ORIENTED_EDGE ( 'NONE', *, *, #24278, .T. ) ;
#129113 = DIRECTION ( 'NONE',  ( -0.000000000000000000, -1.000000000000000000, -0.000000000000000000 ) ) ;
#129114 = ORIENTED_EDGE ( 'NONE', *, *, #92293, .F. ) ;
#129115 = EDGE_CURVE ( 'NONE', #32550, #29908, #22546, .T. ) ;
#129116 = DIRECTION ( 'NONE',  ( 0.000000000000000000, 1.000000000000000000, 0.000000000000000000 ) ) ;
#129117 = CARTESIAN_POINT ( 'NONE',  ( -0.6000000000000388356, 2.500000000000000000, 4.676537180435972552 ) ) ;
#129118 = CIRCLE ( 'NONE', #47533, 0.06509327318403745899 ) ;
#129119 = CARTESIAN_POINT ( 'NONE',  ( 4.149999999999939959, 12.50000000000000000, -2.165063509461101710 ) ) ;
#129120 = ADVANCED_FACE ( 'NONE', ( #96936 ), #68492, .T. ) ;
#129121 = ORIENTED_EDGE ( 'NONE', *, *, #78405, .T. ) ;
#129122 = DIRECTION ( 'NONE',  ( 0.000000000000000000, 0.000000000000000000, 1.000000000000000000 ) ) ;
#129123 = EDGE_CURVE ( 'NONE', #2269, #118223, #16240, .T. ) ;
#129124 = CARTESIAN_POINT ( 'NONE',  ( 9.399999999999915090, 12.50000000000000000, -3.983716857408426293 ) ) ;
#129125 = ORIENTED_EDGE ( 'NONE', *, *, #125520, .F. ) ;
#129126 = FACE_OUTER_BOUND ( 'NONE', #44189, .T. ) ;
#129127 = ADVANCED_FACE ( 'NONE', ( #37394 ), #126993, .T. ) ;
#129128 = ORIENTED_EDGE ( 'NONE', *, *, #122856, .T. ) ;
#129129 = CARTESIAN_POINT ( 'NONE',  ( -11.25000000000000000, 2.500000000000000000, -7.188010851410850499 ) ) ;
#129130 = EDGE_CURVE ( 'NONE', #11303, #72411, #77304, .T. ) ;
#129132 = ADVANCED_FACE ( 'NONE', ( #120929 ), #111087, .T. ) ;
#129131 = CIRCLE ( 'NONE', #41296, 2.000000000000000000 ) ;
#129133 = ADVANCED_FACE ( 'NONE', ( #27538 ), #116513, .T. ) ;
#129134 = VERTEX_POINT ( 'NONE', #127689 ) ;
#129135 = DIRECTION ( 'NONE',  ( 1.000000000000000000, 0.000000000000000000, 0.000000000000000000 ) ) ;
#129136 = DIRECTION ( 'NONE',  ( 0.000000000000000000, 0.000000000000000000, 1.000000000000000000 ) ) ;
#129137 = VERTEX_POINT ( 'NONE', #76665 ) ;
#129138 = ORIENTED_EDGE ( 'NONE', *, *, #113835, .F. ) ;
#129139 = CARTESIAN_POINT ( 'NONE',  ( -10.84999999999999964, 2.500000000000000000, 1.472243186433545459 ) ) ;
#129140 = DIRECTION ( 'NONE',  ( -0.000000000000000000, -1.000000000000000000, -0.000000000000000000 ) ) ;
#129141 = ORIENTED_EDGE ( 'NONE', *, *, #111965, .F. ) ;
#129142 = ADVANCED_FACE ( 'NONE', ( #46543 ), #128364, .F. ) ;
#129143 = AXIS2_PLACEMENT_3D ( 'NONE', #106321, #58529, #15987 ) ;
#129144 = CARTESIAN_POINT ( 'NONE',  ( 185.7083333333333428, -4.445597072760163471, -7.699999999999919353 ) ) ;
#129145 = CARTESIAN_POINT ( 'NONE',  ( 186.7343750003414016, 8.734944146203032389, 5.348610694689227483E-16 ) ) ;
#129146 = CIRCLE ( 'NONE', #72692, 0.06509327318403745899 ) ;
#129147 = DIRECTION ( 'NONE',  ( 0.000000000000000000, -0.000000000000000000, 1.000000000000000000 ) ) ;
#129148 = DIRECTION ( 'NONE',  ( 0.000000000000000000, 0.000000000000000000, 1.000000000000000000 ) ) ;
#129149 = FACE_OUTER_BOUND ( 'NONE', #103391, .T. ) ;
#129150 = DIRECTION ( 'NONE',  ( 0.000000000000000000, 0.000000000000000000, -1.000000000000000000 ) ) ;
#129151 = CARTESIAN_POINT ( 'NONE',  ( -12.49999999999999289, 12.50000000000000000, 5.022947341949748790 ) ) ;
#129152 = VECTOR ( 'NONE', #17040, 1000.000000000000000 ) ;
#129153 = ORIENTED_EDGE ( 'NONE', *, *, #86447, .F. ) ;
#129154 = ORIENTED_EDGE ( 'NONE', *, *, #15380, .F. ) ;
#129155 = ORIENTED_EDGE ( 'NONE', *, *, #73708, .F. ) ;
#129156 = ORIENTED_EDGE ( 'NONE', *, *, #76603, .T. ) ;
#129157 = DIRECTION ( 'NONE',  ( 0.000000000000000000, 1.000000000000000000, 0.000000000000000000 ) ) ;
#129158 = CARTESIAN_POINT ( 'NONE',  ( -8.550000000000013145, 12.50000000000000000, 2.576566944158910744 ) ) ;
#129159 = CIRCLE ( 'NONE', #116602, 0.06509327318403745899 ) ;
#129160 = CARTESIAN_POINT ( 'NONE',  ( -1.850000000000033840, 12.50000000000000000, 6.841600689897072485 ) ) ;
#129161 = VERTEX_POINT ( 'NONE', #86472 ) ;
#129162 = FACE_BOUND ( 'NONE', #26915, .T. ) ;
#129163 = ORIENTED_EDGE ( 'NONE', *, *, #99674, .T. ) ;
#129164 = EDGE_CURVE ( 'NONE', #6313, #89626, #93540, .T. ) ;
#129165 = DIRECTION ( 'NONE',  ( 0.000000000000000000, 0.000000000000000000, 1.000000000000000000 ) ) ;
#129166 = LINE ( 'NONE', #100953, #12248 ) ;
#129167 = CARTESIAN_POINT ( 'NONE',  ( -8.350000000000012079, 12.50000000000000000, 2.792790559304612064 ) ) ;
#129168 = CIRCLE ( 'NONE', #104096, 0.06509327318403745899 ) ;
#129169 = CARTESIAN_POINT ( 'NONE',  ( -8.950000000000009948, 2.500000000000000000, -1.718653347947326049 ) ) ;
#129170 = CARTESIAN_POINT ( 'NONE',  ( -13.34999999999999076, 2.500000000000000000, 2.757883832488653209 ) ) ;
#129171 = CONICAL_SURFACE ( 'NONE', #30867, 0.09999999999999982514, 0.003490658503988666988 ) ;
#129172 = DIRECTION ( 'NONE',  ( -4.274815082592931898E-19, -0.9999939076577903929, -0.003490651415223739937 ) ) ;
#129173 = ORIENTED_EDGE ( 'NONE', *, *, #93672, .T. ) ;
#129174 = CARTESIAN_POINT ( 'NONE',  ( 10.79999999999991012, 2.500000000000000000, 4.330127018922196314 ) ) ;
#129175 = CARTESIAN_POINT ( 'NONE',  ( 1.449999999999952216, 2.500000000000000000, 1.918653347947321564 ) ) ;
#129176 = CONICAL_SURFACE ( 'NONE', #47588, 0.09999999999999982514, 0.003490658503988666988 ) ;
#129177 = CIRCLE ( 'NONE', #85316, 0.06509327318403745899 ) ;
#129178 = CARTESIAN_POINT ( 'NONE',  ( -6.700000000000019718, 12.50000000000000000, -4.330127018922201643 ) ) ;
#129179 = ORIENTED_EDGE ( 'NONE', *, *, #79714, .F. ) ;
#129181 = ORIENTED_EDGE ( 'NONE', *, *, #52377, .T. ) ;
#129180 = VECTOR ( 'NONE', #32353, 1000.000000000000000 ) ;
#129182 = EDGE_CURVE ( 'NONE', #92915, #104745, #108046, .T. ) ;
#129183 = EDGE_LOOP ( 'NONE', ( #107860, #21727, #15972, #63592 ) ) ;
#129184 = VERTEX_POINT ( 'NONE', #116573 ) ;
#129185 = FACE_OUTER_BOUND ( 'NONE', #46274, .T. ) ;
#129186 = CARTESIAN_POINT ( 'NONE',  ( -5.600000000000020073, 2.500000000000000000, 4.576537180435972019 ) ) ;
#129187 = UNCERTAINTY_MEASURE_WITH_UNIT (LENGTH_MEASURE( 1.000000000000000082E-05 ), #57700, 'distance_accuracy_value', 'NONE');
#129189 = EDGE_LOOP ( 'NONE', ( #65343, #115600, #113816, #121964 ) ) ;
#129188 = ORIENTED_EDGE ( 'NONE', *, *, #107753, .T. ) ;
#129191 = VERTEX_POINT ( 'NONE', #49155 ) ;
#129190 = CONICAL_SURFACE ( 'NONE', #120742, 0.09999999999999982514, 0.003490658503988666988 ) ;
#129192 = CARTESIAN_POINT ( 'NONE',  ( 5.799999999999934985, 12.50000000000000000, -4.265033745738164406 ) ) ;
#129193 = AXIS2_PLACEMENT_3D ( 'NONE', #38467, #65314, #96707 ) ;
#129194 = FACE_OUTER_BOUND ( 'NONE', #106079, .T. ) ;
#129195 = DIRECTION ( 'NONE',  ( 0.000000000000000000, 0.000000000000000000, 1.000000000000000000 ) ) ;
#129196 = PLANE ( 'NONE',  #56346 ) ;
#129197 = CARTESIAN_POINT ( 'NONE',  ( 179.5000000000000000, -1.375000000000000000, 7.634788798650553154 ) ) ;
#129198 = DIRECTION ( 'NONE',  ( 0.000000000000000000, 0.000000000000000000, 1.000000000000000000 ) ) ;
#129199 = CARTESIAN_POINT ( 'NONE',  ( 186.2812500006828031, 0.000000000000000000, 7.700000000000000178 ) ) ;
#129200 = AXIS2_PLACEMENT_3D ( 'NONE', #65890, #14204, #24693 ) ;
#129201 = ADVANCED_FACE ( 'NONE', ( #18376 ), #58327, .T. ) ;
#129202 = EDGE_LOOP ( 'NONE', ( #83003, #111553 ) ) ;
#129203 = CARTESIAN_POINT ( 'NONE',  ( -8.350000000000012079, 2.500000000000000000, 1.572243186433545548 ) ) ;
#129204 = VERTEX_POINT ( 'NONE', #68765 ) ;
#129206 = VECTOR ( 'NONE', #27633, 1000.000000000000000 ) ;
#129205 = VECTOR ( 'NONE', #33570, 1000.000000000000000 ) ;
#129207 = ORIENTED_EDGE ( 'NONE', *, *, #70681, .T. ) ;
#129208 = VERTEX_POINT ( 'NONE', #108695 ) ;
#129209 = FACE_OUTER_BOUND ( 'NONE', #61513, .T. ) ;
#129210 = ORIENTED_EDGE ( 'NONE', *, *, #65421, .T. ) ;
#129211 = ORIENTED_EDGE ( 'NONE', *, *, #66525, .F. ) ;
#129212 =( NAMED_UNIT ( * ) PLANE_ANGLE_UNIT ( ) SI_UNIT ( $, .RADIAN. ) );
#129213 = CARTESIAN_POINT ( 'NONE',  ( 4.599999999999936584, 12.50000000000000000, 4.330127018922196314 ) ) ;
#129214 = DIRECTION ( 'NONE',  ( 0.000000000000000000, 0.000000000000000000, 1.000000000000000000 ) ) ;
#129215 = DIRECTION ( 'NONE',  ( 0.000000000000000000, 1.000000000000000000, 0.000000000000000000 ) ) ;
#129216 = DIRECTION ( 'NONE',  ( -0.000000000000000000, -1.000000000000000000, -0.000000000000000000 ) ) ;
#129217 = ORIENTED_EDGE ( 'NONE', *, *, #38369, .F. ) ;
#129218 = CARTESIAN_POINT ( 'NONE',  ( -4.350000000000023626, 2.500000000000000000, 6.841600689897072485 ) ) ;
#129219 = EDGE_LOOP ( 'NONE', ( #16767, #59514 ) ) ;
#129220 = CARTESIAN_POINT ( 'NONE',  ( 18.46077503349216187, -0.2574728941692127626, 4.048716373199397367 ) ) ;
#129221 = ADVANCED_FACE ( 'NONE', ( #19010 ), #108200, .T. ) ;
#129222 = ORIENTED_EDGE ( 'NONE', *, *, #83512, .F. ) ;
#129223 = CARTESIAN_POINT ( 'NONE',  ( 9.999999999999952038, 2.500000000000000000, -0.1000000000000022815 ) ) ;
#129224 = DIRECTION ( 'NONE',  ( 0.000000000000000000, 1.000000000000000000, 0.000000000000000000 ) ) ;
#129225 = ORIENTED_EDGE ( 'NONE', *, *, #74349, .T. ) ;
#129227 = AXIS2_PLACEMENT_3D ( 'NONE', #29339, #39811, #77760 ) ;
#129226 = DIRECTION ( 'NONE',  ( -0.000000000000000000, 1.000000000000000000, -0.000000000000000000 ) ) ;
#129228 = DIRECTION ( 'NONE',  ( -0.000000000000000000, 1.000000000000000000, -0.000000000000000000 ) ) ;
#129229 = ORIENTED_EDGE ( 'NONE', *, *, #53015, .T. ) ;
#129230 = AXIS2_PLACEMENT_3D ( 'NONE', #19039, #77975, #77333 ) ;
#129231 = CARTESIAN_POINT ( 'NONE',  ( -8.749999999999975131, 2.500000000000000000, -2.165063509461101710 ) ) ;
#129232 = EDGE_LOOP ( 'NONE', ( #54131, #43768, #4057, #32733 ) ) ;
#129233 = ADVANCED_FACE ( 'NONE', ( #114331 ), #73127, .T. ) ;
#129235 = ORIENTED_EDGE ( 'NONE', *, *, #95818, .T. ) ;
#129234 = ADVANCED_FACE ( 'NONE', ( #84218 ), #24672, .T. ) ;
#129236 = CARTESIAN_POINT ( 'NONE',  ( -4.600000000000028066, 12.50000000000000000, -3.637306695894650055 ) ) ;
#129237 = CARTESIAN_POINT ( 'NONE',  ( -2.900000000000029221, 12.50000000000000000, -5.088040615133791356 ) ) ;
#129238 = EDGE_CURVE ( 'NONE', #61247, #91045, #82954, .T. ) ;
#129239 = CARTESIAN_POINT ( 'NONE',  ( 10.19999999999991225, 2.500000000000000000, 3.883716857408420431 ) ) ;
#129240 = ADVANCED_FACE ( 'NONE', ( #63300 ), #44439, .F. ) ;
#129241 = CARTESIAN_POINT ( 'NONE',  ( -12.09999999999999609, 2.500000000000000000, 0.5928203230275536084 ) ) ;
#129242 = CARTESIAN_POINT ( 'NONE',  ( 3.349999999999945466, 2.500000000000000000, -6.395190528383301931 ) ) ;
#129243 = CIRCLE ( 'NONE', #79054, 0.06509327318403745899 ) ;
#129244 = VERTEX_POINT ( 'NONE', #27888 ) ;
#129245 = CARTESIAN_POINT ( 'NONE',  ( 2.899999999999946620, 12.50000000000000000, 0.6928203230275494784 ) ) ;
#129246 = EDGE_CURVE ( 'NONE', #94085, #122392, #37119, .T. ) ;
#129247 = ORIENTED_EDGE ( 'NONE', *, *, #72595, .T. ) ;
#129248 = ADVANCED_FACE ( 'NONE', ( #8239 ), #11469, .T. ) ;
#129249 = DIRECTION ( 'NONE',  ( 0.000000000000000000, -0.9999939076577903929, 0.003490651415223739937 ) ) ;
#129251 = AXIS2_PLACEMENT_3D ( 'NONE', #66025, #55570, #98062 ) ;
#129250 = CARTESIAN_POINT ( 'NONE',  ( -3.100000000000028511, 2.500000000000000000, -4.576537180435977348 ) ) ;
#129252 = EDGE_CURVE ( 'NONE', #75374, #24991, #97740, .T. ) ;
#129253 = VECTOR ( 'NONE', #68183, 1000.000000000000000 ) ;
#129254 = CARTESIAN_POINT ( 'NONE',  ( 186.8802083336747444, 4.367472073101515306, 7.564683531250000925 ) ) ;
#129255 = DIRECTION ( 'NONE',  ( 0.000000000000000000, 0.000000000000000000, -1.000000000000000000 ) ) ;
#129256 = DIRECTION ( 'NONE',  ( -0.000000000000000000, -1.000000000000000000, -0.000000000000000000 ) ) ;
#129257 = DIRECTION ( 'NONE',  ( 0.000000000000000000, 0.000000000000000000, 1.000000000000000000 ) ) ;
#129258 = DIRECTION ( 'NONE',  ( 0.000000000000000000, 0.000000000000000000, 1.000000000000000000 ) ) ;
#129259 = VERTEX_POINT ( 'NONE', #51422 ) ;
#129260 = CIRCLE ( 'NONE', #110439, 0.06509327318403745899 ) ;
#129261 = PLANE ( 'NONE',  #94050 ) ;
#129262 = DIRECTION ( 'NONE',  ( 0.000000000000000000, 0.000000000000000000, 1.000000000000000000 ) ) ;
#129263 =( GEOMETRIC_REPRESENTATION_CONTEXT ( 3 ) GLOBAL_UNCERTAINTY_ASSIGNED_CONTEXT ( ( #112372 ) ) GLOBAL_UNIT_ASSIGNED_CONTEXT ( ( #104838, #116597, #26943 ) ) REPRESENTATION_CONTEXT ( 'NONE', 'WORKASPACE' ) );
#129264 = CIRCLE ( 'NONE', #108297, 0.06509327318403745899 ) ;
#129265 = ORIENTED_EDGE ( 'NONE', *, *, #54070, .F. ) ;
#129266 = AXIS2_PLACEMENT_3D ( 'NONE', #91339, #89412, #29849 ) ;
#129267 = FACE_OUTER_BOUND ( 'NONE', #106618, .T. ) ;
#129268 = CONICAL_SURFACE ( 'NONE', #72815, 0.1000000000000002554, 0.003490658503988666988 ) ;
#129269 = ORIENTED_EDGE ( 'NONE', *, *, #26374, .T. ) ;
#129270 = VERTEX_POINT ( 'NONE', #101797 ) ;
#129271 = CARTESIAN_POINT ( 'NONE',  ( 4.599999999999937472, 12.50000000000000000, 0.6928203230275494784 ) ) ;
#129272 = ORIENTED_EDGE ( 'NONE', *, *, #87837, .F. ) ;
#129273 = CARTESIAN_POINT ( 'NONE',  ( -7.300000000000016698, 12.50000000000000000, -4.741630453620016006 ) ) ;
#129274 = CARTESIAN_POINT ( 'NONE',  ( -4.350000000000027178, 2.500000000000000000, -6.048780366869526581 ) ) ;
#129275 = ORIENTED_EDGE ( 'NONE', *, *, #110709, .T. ) ;
#129276 = CARTESIAN_POINT ( 'NONE',  ( -7.700000000000016165, 12.50000000000000000, 0.2813168883297361700 ) ) ;
#129278 = ORIENTED_EDGE ( 'NONE', *, *, #103796, .T. ) ;
#129277 = DIRECTION ( 'NONE',  ( -0.000000000000000000, -1.000000000000000000, -0.000000000000000000 ) ) ;
#129279 = DIRECTION ( 'NONE',  ( 0.000000000000000000, 0.000000000000000000, 1.000000000000000000 ) ) ;
#129280 = AXIS2_PLACEMENT_3D ( 'NONE', #11599, #89515, #9668 ) ;
#129281 = DIRECTION ( 'NONE',  ( -0.000000000000000000, 1.000000000000000000, -0.000000000000000000 ) ) ;
#129282 = EDGE_LOOP ( 'NONE', ( #20683, #68483 ) ) ;
#129283 = EDGE_CURVE ( 'NONE', #36770, #84687, #85224, .T. ) ;
#129285 = AXIS2_PLACEMENT_3D ( 'NONE', #70168, #9954, #70800 ) ;
#129284 = CONICAL_SURFACE ( 'NONE', #64412, 0.1000000000000000472, 0.003490658503988666988 ) ;
#129286 = VERTEX_POINT ( 'NONE', #42235 ) ;
#129287 = EDGE_CURVE ( 'NONE', #4055, #51156, #89428, .T. ) ;
#129288 = VERTEX_POINT ( 'NONE', #112900 ) ;
#129289 = DIRECTION ( 'NONE',  ( -0.000000000000000000, 1.000000000000000000, -0.000000000000000000 ) ) ;
#129290 = DIRECTION ( 'NONE',  ( 0.000000000000000000, 0.000000000000000000, -1.000000000000000000 ) ) ;
#129291 = DIRECTION ( 'NONE',  ( -0.000000000000000000, -1.000000000000000000, -0.000000000000000000 ) ) ;
#129292 = FACE_BOUND ( 'NONE', #21275, .T. ) ;
#129293 = ORIENTED_EDGE ( 'NONE', *, *, #58006, .F. ) ;
#129294 = DIRECTION ( 'NONE',  ( 0.000000000000000000, 0.000000000000000000, 1.000000000000000000 ) ) ;
#129295 = DIRECTION ( 'NONE',  ( 0.000000000000000000, 0.000000000000000000, -1.000000000000000000 ) ) ;
#129296 = ORIENTED_EDGE ( 'NONE', *, *, #121965, .T. ) ;
#129297 = ADVANCED_FACE ( 'NONE', ( #12739 ), #82809, .T. ) ;
#129298 = CARTESIAN_POINT ( 'NONE',  ( -4.600000000000028955, 12.50000000000000000, -4.395220292106239768 ) ) ;
#129299 = DIRECTION ( 'NONE',  ( 0.000000000000000000, -0.000000000000000000, 1.000000000000000000 ) ) ;
#129300 = LINE ( 'NONE', #21242, #42337 ) ;
#129301 = DIRECTION ( 'NONE',  ( 0.000000000000000000, 0.000000000000000000, -1.000000000000000000 ) ) ;
#129302 = CARTESIAN_POINT ( 'NONE',  ( -4.400000000000028777, 2.500000000000000000, -4.676537180435978769 ) ) ;
#129303 = DIRECTION ( 'NONE',  ( -4.274815082592931898E-19, -0.9999939076577903929, -0.003490651415223739937 ) ) ;
#129304 = CARTESIAN_POINT ( 'NONE',  ( 0.8499999999999553468, 2.500000000000000000, -2.265063509461101798 ) ) ;
#129305 = CONICAL_SURFACE ( 'NONE', #51930, 0.09999999999999982514, 0.003490658503988666988 ) ;
#129306 = CIRCLE ( 'NONE', #8275, 0.09999999999999999167 ) ;
#129307 = ORIENTED_EDGE ( 'NONE', *, *, #58044, .T. ) ;
#129308 = ORIENTED_EDGE ( 'NONE', *, *, #91409, .T. ) ;
#129309 = EDGE_LOOP ( 'NONE', ( #76691, #44499, #110491, #119022 ) ) ;
#129310 = AXIS2_PLACEMENT_3D ( 'NONE', #71875, #92134, #42414 ) ;
#129311 = ORIENTED_EDGE ( 'NONE', *, *, #66525, .T. ) ;
#129312 = VERTEX_POINT ( 'NONE', #31137 ) ;
#129313 = DIRECTION ( 'NONE',  ( 0.000000000000000000, -0.000000000000000000, 1.000000000000000000 ) ) ;
#129314 = DIRECTION ( 'NONE',  ( 0.000000000000000000, -0.000000000000000000, 1.000000000000000000 ) ) ;
#129315 = ORIENTED_EDGE ( 'NONE', *, *, #27662, .T. ) ;
#129316 = FACE_BOUND ( 'NONE', #101264, .T. ) ;
#129317 = CARTESIAN_POINT ( 'NONE',  ( -12.09999999999999432, 12.50000000000000000, 3.637306695894644726 ) ) ;
#129318 = AXIS2_PLACEMENT_3D ( 'NONE', #95678, #57018, #97599 ) ;
#129319 = VECTOR ( 'NONE', #15660, 1000.000000000000000 ) ;
#129320 = AXIS2_PLACEMENT_3D ( 'NONE', #61633, #11862, #41988 ) ;
#129321 = DIRECTION ( 'NONE',  ( 0.000000000000000000, 1.000000000000000000, 0.000000000000000000 ) ) ;
#129322 = CARTESIAN_POINT ( 'NONE',  ( 12.89999999999989910, 2.500000000000000000, 0.6928203230275494784 ) ) ;
#129323 = PLANE ( 'NONE',  #45457 ) ;
#129324 = DIRECTION ( 'NONE',  ( -0.000000000000000000, 1.000000000000000000, -0.000000000000000000 ) ) ;
#129325 = CARTESIAN_POINT ( 'NONE',  ( 3.349999999999942801, 12.50000000000000000, 2.792790559304612064 ) ) ;
#129326 = ORIENTED_EDGE ( 'NONE', *, *, #54680, .T. ) ;
#129327 = AXIS2_PLACEMENT_3D ( 'NONE', #27327, #17514, #10897 ) ;
#129328 = ORIENTED_EDGE ( 'NONE', *, *, #94049, .T. ) ;
#129329 = AXIS2_PLACEMENT_3D ( 'NONE', #56902, #64805, #104718 ) ;
#129330 = EDGE_CURVE ( 'NONE', #86526, #74427, #62253, .T. ) ;
#129331 = ORIENTED_EDGE ( 'NONE', *, *, #89783, .T. ) ;
#129332 = VERTEX_POINT ( 'NONE', #63149 ) ;
#129333 = CARTESIAN_POINT ( 'NONE',  ( 10.63722763359408319, 2.500000000000000444, 8.014330155125131583 ) ) ;
#129334 = DIRECTION ( 'NONE',  ( 0.000000000000000000, 0.000000000000000000, 1.000000000000000000 ) ) ;
#129335 = EDGE_LOOP ( 'NONE', ( #91163, #73307 ) ) ;
#129336 = LINE ( 'NONE', #119474, #62281 ) ;
#129337 = CONICAL_SURFACE ( 'NONE', #54092, 0.1000000000000002554, 0.003490658503988666988 ) ;
#129338 = CARTESIAN_POINT ( 'NONE',  ( -1.250000000000037970, 2.500000000000000000, 2.857883832488649301 ) ) ;
#129339 = DIRECTION ( 'NONE',  ( 0.000000000000000000, 0.000000000000000000, 1.000000000000000000 ) ) ;
#129340 = CIRCLE ( 'NONE', #85400, 0.06509327318403741736 ) ;
#129341 = CARTESIAN_POINT ( 'NONE',  ( 5.599999999999933031, 2.500000000000000000, -0.3464101615137783474 ) ) ;
#129342 = CARTESIAN_POINT ( 'NONE',  ( 6.649999999999931966, 2.500000000000000000, -5.902370205355750521 ) ) ;
#129343 = DIRECTION ( 'NONE',  ( -4.274815082592931898E-19, -0.9999939076577903929, -0.003490651415223739937 ) ) ;
#129344 = EDGE_CURVE ( 'NONE', #59339, #80261, #82152, .T. ) ;
#129345 = AXIS2_PLACEMENT_3D ( 'NONE', #56737, #96671, #7652 ) ;
#129346 = FACE_OUTER_BOUND ( 'NONE', #71273, .T. ) ;
#129347 = ADVANCED_FACE ( 'NONE', ( #52687 ), #54606, .T. ) ;
#129348 = VERTEX_POINT ( 'NONE', #114189 ) ;
#129349 = CARTESIAN_POINT ( 'NONE',  ( 3.949999999999942446, 2.500000000000000000, -6.741600689897078169 ) ) ;
#129350 = CONICAL_SURFACE ( 'NONE', #112606, 0.1000000000000002554, 0.003490658503988666988 ) ;
#129351 = ORIENTED_EDGE ( 'NONE', *, *, #59304, .T. ) ;
#129352 = VERTEX_POINT ( 'NONE', #85366 ) ;
#129353 = MECHANICAL_DESIGN_GEOMETRIC_PRESENTATION_REPRESENTATION (  '', ( #35248 ), #16423 ) ;
#129354 = CARTESIAN_POINT ( 'NONE',  ( -8.750000000000008882, 2.500000000000000000, -2.857883832488653741 ) ) ;
#129355 = CARTESIAN_POINT ( 'NONE',  ( 3.299999999999944755, 2.500000000000000000, -2.385244779468109755E-15 ) ) ;
#129357 = EDGE_CURVE ( 'NONE', #127183, #114003, #84720, .T. ) ;
#129356 = CARTESIAN_POINT ( 'NONE',  ( -3.749999999999994671, 12.50000000000000000, -6.495190528383302464 ) ) ;
#129358 = ORIENTED_EDGE ( 'NONE', *, *, #57135, .F. ) ;
#129359 = AXIS2_PLACEMENT_3D ( 'NONE', #44170, #42918, #124676 ) ;
#129360 = VERTEX_POINT ( 'NONE', #124659 ) ;
#129361 = DIRECTION ( 'NONE',  ( -0.000000000000000000, 1.000000000000000000, -0.000000000000000000 ) ) ;
#129362 = CONICAL_SURFACE ( 'NONE', #45721, 0.1000000000000002554, 0.003490658503988666988 ) ;
#129363 = CARTESIAN_POINT ( 'NONE',  ( -3.950000000000024603, 12.50000000000000000, 1.818653347947321475 ) ) ;
#129364 = CARTESIAN_POINT ( 'NONE',  ( 0.5999999999999560130, 2.500000000000000000, -4.083716857408426826 ) ) ;
#129365 = CARTESIAN_POINT ( 'NONE',  ( -11.89999999999999680, 12.50000000000000000, -0.3464101615137741841 ) ) ;
#129366 = ORIENTED_EDGE ( 'NONE', *, *, #58252, .F. ) ;
#129367 = CARTESIAN_POINT ( 'NONE',  ( 139.9358549477330200, 0.5000000000000000000, -3.576063159858998475 ) ) ;
#129368 = AXIS2_PLACEMENT_3D ( 'NONE', #3405, #62341, #13859 ) ;
#129369 = ORIENTED_EDGE ( 'NONE', *, *, #911, .T. ) ;
#129370 = CARTESIAN_POINT ( 'NONE',  ( -5.650000000000019895, 2.500000000000000000, 1.718653347947321386 ) ) ;
#129371 = ORIENTED_EDGE ( 'NONE', *, *, #25247, .T. ) ;
#129372 = CARTESIAN_POINT ( 'NONE',  ( 3.149999999999944400, 2.500000000000000000, 1.718653347947321386 ) ) ;
#129373 = ADVANCED_FACE ( 'NONE', ( #35006 ), #55967, .T. ) ;
#129375 = CIRCLE ( 'NONE', #64584, 0.06509327318403741736 ) ;
#129374 = CIRCLE ( 'NONE', #108495, 0.1000000000000000056 ) ;
#129376 = DIRECTION ( 'NONE',  ( 0.000000000000000000, 0.000000000000000000, 1.000000000000000000 ) ) ;
#129377 = FACE_OUTER_BOUND ( 'NONE', #98995, .T. ) ;
#129378 = CONICAL_SURFACE ( 'NONE', #3948, 0.09999999999999982514, 0.003490658503988666988 ) ;
#129379 = CARTESIAN_POINT ( 'NONE',  ( -1.900000000000034550, 2.500000000000000000, 4.776537180435972196 ) ) ;
#129380 = ORIENTED_EDGE ( 'NONE', *, *, #53007, .T. ) ;
#129381 = ADVANCED_FACE ( 'NONE', ( #74265 ), #53832, .T. ) ;
#129382 = DIRECTION ( 'NONE',  ( 0.000000000000000000, 1.000000000000000000, 0.000000000000000000 ) ) ;
#129384 = CIRCLE ( 'NONE', #89646, 0.06509327318403745899 ) ;
#129383 = CONICAL_SURFACE ( 'NONE', #72915, 0.09999999999999982514, 0.003490658503988666988 ) ;
#129385 = VERTEX_POINT ( 'NONE', #74909 ) ;
#129386 = ORIENTED_EDGE ( 'NONE', *, *, #111349, .T. ) ;
#129387 = ADVANCED_FACE ( 'NONE', ( #84070 ), #39290, .T. ) ;
#129388 = ADVANCED_FACE ( 'NONE', ( #114815 ), #129171, .T. ) ;
#129389 = DIRECTION ( 'NONE',  ( -0.000000000000000000, 1.000000000000000000, -0.000000000000000000 ) ) ;
#129390 = DIRECTION ( 'NONE',  ( 0.000000000000000000, 1.000000000000000000, 0.000000000000000000 ) ) ;
#129391 = DIRECTION ( 'NONE',  ( 0.000000000000000000, 1.000000000000000000, 0.000000000000000000 ) ) ;
#129392 = EDGE_CURVE ( 'NONE', #118832, #45708, #55272, .T. ) ;
#129393 =( LENGTH_UNIT ( ) NAMED_UNIT ( * ) SI_UNIT ( .MILLI., .METRE. ) );
#129394 = ADVANCED_FACE ( 'NONE', ( #65722 ), #99804, .T. ) ;
#129395 = DIRECTION ( 'NONE',  ( 0.000000000000000000, 0.000000000000000000, 1.000000000000000000 ) ) ;
#129396 = CARTESIAN_POINT ( 'NONE',  ( -6.249999999999984901, 12.50000000000000000, -2.165063509461101710 ) ) ;
#129397 = PLANE ( 'NONE',  #19725 ) ;
#129398 = CARTESIAN_POINT ( 'NONE',  ( -2.300000000000032685, 2.500000000000000000, -0.4464101615137783252 ) ) ;
#129399 = CARTESIAN_POINT ( 'NONE',  ( 9.199999999999915801, 12.50000000000000000, 4.330127018922196314 ) ) ;
#129400 = EDGE_CURVE ( 'NONE', #47255, #62375, #85988, .T. ) ;
#129401 = VECTOR ( 'NONE', #117661, 1000.000000000000000 ) ;
#129402 = EDGE_CURVE ( 'NONE', #61169, #53570, #81025, .T. ) ;
#129403 = EDGE_CURVE ( 'NONE', #92009, #35838, #59146, .T. ) ;
#129404 = ADVANCED_FACE ( 'NONE', ( #29673 ), #74768, .T. ) ;
#129405 = AXIS2_PLACEMENT_3D ( 'NONE', #78830, #40842, #33428 ) ;
#129406 = EDGE_LOOP ( 'NONE', ( #68758, #34405 ) ) ;
#129407 = CARTESIAN_POINT ( 'NONE',  ( 6.049999999999932321, 12.50000000000000000, -1.883746621131363597 ) ) ;
#129408 = CARTESIAN_POINT ( 'NONE',  ( 15.19999999999989093, 2.500000000000000000, 0.4464101615137735513 ) ) ;
#129409 = CARTESIAN_POINT ( 'NONE',  ( 1.849999999999949685, 12.50000000000000000, -2.511473670974877948 ) ) ;
#129410 = CARTESIAN_POINT ( 'NONE',  ( 9.399999999999918643, 12.50000000000000000, -0.3464101615137782364 ) ) ;
#129411 = DIRECTION ( 'NONE',  ( -0.000000000000000000, -1.000000000000000000, -0.000000000000000000 ) ) ;
#129412 = ADVANCED_FACE ( 'NONE', ( #17907 ), #127098, .T. ) ;
#129413 = AXIS2_PLACEMENT_3D ( 'NONE', #68351, #70936, #60494 ) ;
#129414 = ORIENTED_EDGE ( 'NONE', *, *, #25571, .F. ) ;
#129415 = VECTOR ( 'NONE', #39224, 1000.000000000000000 ) ;
#129416 = LINE ( 'NONE', #409, #86332 ) ;
#129417 = AXIS2_PLACEMENT_3D ( 'NONE', #54162, #15504, #55445 ) ;
#129418 = DIRECTION ( 'NONE',  ( 0.000000000000000000, 0.000000000000000000, 1.000000000000000000 ) ) ;
#129420 = VERTEX_POINT ( 'NONE', #99713 ) ;
#129419 = DIRECTION ( 'NONE',  ( 0.000000000000000000, -0.000000000000000000, 1.000000000000000000 ) ) ;
#129421 = CONICAL_SURFACE ( 'NONE', #52039, 0.1000000000000000472, 0.003490658503988666988 ) ;
#129422 = ORIENTED_EDGE ( 'NONE', *, *, #14070, .F. ) ;
#129423 = CARTESIAN_POINT ( 'NONE',  ( 3.099999999999945022, 12.50000000000000000, -4.676537180435978769 ) ) ;
#129424 = VECTOR ( 'NONE', #94119, 1000.000000000000000 ) ;
#129425 = ORIENTED_EDGE ( 'NONE', *, *, #39476, .F. ) ;
#129426 = EDGE_LOOP ( 'NONE', ( #1322, #73390, #28052, #94179 ) ) ;
#129427 = EDGE_LOOP ( 'NONE', ( #40312, #127132 ) ) ;
#129428 = FACE_OUTER_BOUND ( 'NONE', #125582, .T. ) ;
#129429 = CARTESIAN_POINT ( 'NONE',  ( 6.649999999999928413, 2.500000000000000000, 2.857883832488649301 ) ) ;
#129430 = DIRECTION ( 'NONE',  ( 0.000000000000000000, 1.000000000000000000, 0.000000000000000000 ) ) ;
#129431 = DIRECTION ( 'NONE',  ( -0.000000000000000000, 1.000000000000000000, -0.000000000000000000 ) ) ;
#129432 = AXIS2_PLACEMENT_3D ( 'NONE', #120622, #9148, #98810 ) ;
#129433 = ORIENTED_EDGE ( 'NONE', *, *, #95685, .F. ) ;
#129434 = FACE_OUTER_BOUND ( 'NONE', #99920, .T. ) ;
#129435 = EDGE_LOOP ( 'NONE', ( #129010, #12628 ) ) ;
#129436 = CIRCLE ( 'NONE', #22900, 0.06509327318403741736 ) ;
#129437 = DIRECTION ( 'NONE',  ( 0.000000000000000000, -0.000000000000000000, 1.000000000000000000 ) ) ;
#129438 = CARTESIAN_POINT ( 'NONE',  ( 14.34999999999989306, 2.500000000000000000, -2.511473670974877948 ) ) ;
#129439 = DIRECTION ( 'NONE',  ( 0.000000000000000000, 1.000000000000000000, 0.000000000000000000 ) ) ;
#129440 = LINE ( 'NONE', #40402, #12063 ) ;
#129441 = EDGE_LOOP ( 'NONE', ( #10723, #50857 ) ) ;
#129442 = EDGE_CURVE ( 'NONE', #123754, #16842, #3743, .T. ) ;
#129443 = AXIS2_PLACEMENT_3D ( 'NONE', #18104, #27931, #50170 ) ;
#129444 = ORIENTED_EDGE ( 'NONE', *, *, #51468, .T. ) ;
#129445 = ORIENTED_EDGE ( 'NONE', *, *, #83225, .T. ) ;
#129447 = ADVANCED_FACE ( 'NONE', ( #8715 ), #57856, .T. ) ;
#129446 = EDGE_LOOP ( 'NONE', ( #101991, #67164 ) ) ;
#129448 = ORIENTED_EDGE ( 'NONE', *, *, #80019, .F. ) ;
#129449 = DIRECTION ( 'NONE',  ( 0.000000000000000000, 0.000000000000000000, 1.000000000000000000 ) ) ;
#129450 = DIRECTION ( 'NONE',  ( 0.000000000000000000, 0.000000000000000000, -1.000000000000000000 ) ) ;
#129451 = DIRECTION ( 'NONE',  ( -0.000000000000000000, 1.000000000000000000, -0.000000000000000000 ) ) ;
#129452 = FACE_BOUND ( 'NONE', #111433, .T. ) ;
#129453 = CARTESIAN_POINT ( 'NONE',  ( -2.100000000000033396, 2.500000000000000000, -0.5928203230275542746 ) ) ;
#129454 = FACE_OUTER_BOUND ( 'NONE', #20043, .T. ) ;
#129455 = CIRCLE ( 'NONE', #29186, 0.1000000000000000472 ) ;
#129456 = DIRECTION ( 'NONE',  ( 0.000000000000000000, 1.000000000000000000, 0.000000000000000000 ) ) ;
#129457 = DIRECTION ( 'NONE',  ( -0.000000000000000000, -1.000000000000000000, -0.000000000000000000 ) ) ;
#129458 = AXIS2_PLACEMENT_3D ( 'NONE', #36379, #35716, #124738 ) ;
#129459 = CARTESIAN_POINT ( 'NONE',  ( 105.5000000000000142, 2.449293598294706414E-16, -2.000000000000000000 ) ) ;
#129460 = DIRECTION ( 'NONE',  ( 0.000000000000000000, 1.000000000000000000, 0.000000000000000000 ) ) ;
#129461 = VECTOR ( 'NONE', #71043, 1000.000000000000000 ) ;
#129462 = CARTESIAN_POINT ( 'NONE',  ( 7.499999999999927169, 12.50000000000000000, -4.957854068765716882 ) ) ;
#129463 = DIRECTION ( 'NONE',  ( 0.000000000000000000, 0.000000000000000000, 1.000000000000000000 ) ) ;
#129465 = AXIS2_PLACEMENT_3D ( 'NONE', #89656, #21558, #81753 ) ;
#129464 = AXIS2_PLACEMENT_3D ( 'NONE', #41667, #61938, #101853 ) ;
#129466 = EDGE_LOOP ( 'NONE', ( #27494, #5909 ) ) ;
#129467 = ORIENTED_EDGE ( 'NONE', *, *, #5337, .T. ) ;
#129468 = ORIENTED_EDGE ( 'NONE', *, *, #29029, .T. ) ;
#129469 = ORIENTED_EDGE ( 'NONE', *, *, #58127, .F. ) ;
#129470 = DIRECTION ( 'NONE',  ( 0.000000000000000000, 1.000000000000000000, 0.000000000000000000 ) ) ;
#129471 = AXIS2_PLACEMENT_3D ( 'NONE', #61852, #90650, #59931 ) ;
#129472 = CARTESIAN_POINT ( 'NONE',  ( 14.14999999999989733, 2.500000000000000000, 2.757883832488649656 ) ) ;
#129473 = FACE_BOUND ( 'NONE', #16841, .T. ) ;
#129474 = PLANE ( 'NONE',  #49951 ) ;
#129476 = CIRCLE ( 'NONE', #54138, 0.09999999999999982514 ) ;
#129475 = CONICAL_SURFACE ( 'NONE', #73011, 0.1000000000000002554, 0.003490658503988666988 ) ;
#129477 = VERTEX_POINT ( 'NONE', #40142 ) ;
#129478 = DIRECTION ( 'NONE',  ( 0.000000000000000000, 0.000000000000000000, 1.000000000000000000 ) ) ;
#129479 = CARTESIAN_POINT ( 'NONE',  ( -3.550000000000031797, 12.50000000000000000, -6.148780366869526226 ) ) ;
#129480 = LINE ( 'NONE', #1140, #15532 ) ;
#129481 = CARTESIAN_POINT ( 'NONE',  ( 11.24999999999994493, 2.500000000000000000, 6.595190528383296780 ) ) ;
#129482 = ORIENTED_EDGE ( 'NONE', *, *, #56071, .T. ) ;
#129483 = LINE ( 'NONE', #58782, #61821 ) ;
#129484 = ADVANCED_FACE ( 'NONE', ( #8087 ), #51880, .T. ) ;
#129485 = EDGE_LOOP ( 'NONE', ( #23737, #54616, #42714, #73466 ) ) ;
#129486 = VERTEX_POINT ( 'NONE', #98395 ) ;
#129487 = AXIS2_PLACEMENT_3D ( 'NONE', #24491, #96433, #84039 ) ;
#129488 = DIRECTION ( 'NONE',  ( -4.274815082592931898E-19, -0.9999939076577903929, -0.003490651415223739937 ) ) ;
#129489 = DIRECTION ( 'NONE',  ( -0.000000000000000000, -1.000000000000000000, -0.000000000000000000 ) ) ;
#129490 = ORIENTED_EDGE ( 'NONE', *, *, #105107, .F. ) ;
#129491 = CIRCLE ( 'NONE', #50068, 0.06509327318403745899 ) ;
#129492 = CARTESIAN_POINT ( 'NONE',  ( -6.250000000000015987, 2.500000000000000000, 5.702370205355745014 ) ) ;
#129493 = AXIS2_PLACEMENT_3D ( 'NONE', #34061, #5227, #45177 ) ;
#129494 = CARTESIAN_POINT ( 'NONE',  ( 1.649999999999951950, 2.500000000000000000, -5.902370205355750521 ) ) ;
#129495 = EDGE_LOOP ( 'NONE', ( #96275, #2717, #55887, #118037 ) ) ;
#129496 = CARTESIAN_POINT ( 'NONE',  ( 7.899999999999924860, 2.500000000000000000, -3.637306695894650055 ) ) ;
#129497 = ORIENTED_EDGE ( 'NONE', *, *, #112519, .F. ) ;
#129498 = EDGE_CURVE ( 'NONE', #109985, #84685, #119332, .T. ) ;
#129499 = EDGE_CURVE ( 'NONE', #88412, #61414, #93637, .T. ) ;
#129500 = CARTESIAN_POINT ( 'NONE',  ( -12.09999999999999609, 2.500000000000000000, 4.330127018922196314 ) ) ;
#129501 = EDGE_LOOP ( 'NONE', ( #122885, #61958 ) ) ;
#129502 = DIRECTION ( 'NONE',  ( 0.000000000000000000, 0.000000000000000000, 1.000000000000000000 ) ) ;
#129503 = FACE_BOUND ( 'NONE', #42834, .T. ) ;
#129504 = CIRCLE ( 'NONE', #121063, 0.1000000000000002554 ) ;
#129505 = ORIENTED_EDGE ( 'NONE', *, *, #64542, .F. ) ;
#129506 = CARTESIAN_POINT ( 'NONE',  ( 107.9999999999992895, 5.855766388783293586, 5.000000000000080824 ) ) ;
#129507 = ORIENTED_EDGE ( 'NONE', *, *, #13405, .T. ) ;
#129508 = DIRECTION ( 'NONE',  ( -0.000000000000000000, -1.000000000000000000, -0.000000000000000000 ) ) ;
#129509 = DIRECTION ( 'NONE',  ( -0.000000000000000000, -1.000000000000000000, -0.000000000000000000 ) ) ;
#129510 = DIRECTION ( 'NONE',  ( 0.000000000000000000, 0.000000000000000000, 1.000000000000000000 ) ) ;
#129512 = ADVANCED_FACE ( 'NONE', ( #109528 ), #67651, .T. ) ;
#129511 = FACE_OUTER_BOUND ( 'NONE', #87949, .T. ) ;
#129513 = CARTESIAN_POINT ( 'NONE',  ( -10.00000000000000355, 12.50000000000000000, 3.572213422710607489 ) ) ;
#129514 = AXIS2_PLACEMENT_3D ( 'NONE', #112849, #34944, #4801 ) ;
#129515 = VERTEX_POINT ( 'NONE', #87922 ) ;
#129516 = ORIENTED_EDGE ( 'NONE', *, *, #93320, .F. ) ;
#129518 = ORIENTED_EDGE ( 'NONE', *, *, #56074, .F. ) ;
#129517 = AXIS2_PLACEMENT_3D ( 'NONE', #3492, #22510, #53883 ) ;
#129519 = DIRECTION ( 'NONE',  ( 0.000000000000000000, -0.000000000000000000, 1.000000000000000000 ) ) ;
#129520 = DIRECTION ( 'NONE',  ( -0.000000000000000000, 1.000000000000000000, 1.846105847067148022E-16 ) ) ;
#129521 = DIRECTION ( 'NONE',  ( 0.000000000000000000, 0.000000000000000000, 1.000000000000000000 ) ) ;
#129523 = ORIENTED_EDGE ( 'NONE', *, *, #17031, .F. ) ;
#129522 = VERTEX_POINT ( 'NONE', #19861 ) ;
#129524 = ORIENTED_EDGE ( 'NONE', *, *, #73107, .F. ) ;
#129525 = CARTESIAN_POINT ( 'NONE',  ( -10.85000000000000142, 12.50000000000000000, -2.922977105672687426 ) ) ;
#129526 = VERTEX_POINT ( 'NONE', #97765 ) ;
#129527 = FACE_OUTER_BOUND ( 'NONE', #71863, .T. ) ;
#129528 = CONTEXT_DEPENDENT_SHAPE_REPRESENTATION ( #26352, #13744 ) ;
#129529 = PLANE ( 'NONE',  #28131 ) ;
#129530 = DIRECTION ( 'NONE',  ( -4.274815082592931898E-19, -0.9999939076577903929, -0.003490651415223739937 ) ) ;
#129531 = DIRECTION ( 'NONE',  ( -0.000000000000000000, -1.000000000000000000, -0.000000000000000000 ) ) ;
#129532 = CARTESIAN_POINT ( 'NONE',  ( 185.7500000000000000, 9.429780353434619030E-16, -7.700000000000000178 ) ) ;
#129533 = AXIS2_PLACEMENT_3D ( 'NONE', #93114, #103576, #71518 ) ;
#129534 = CARTESIAN_POINT ( 'NONE',  ( -4.150000000000027889, 2.500000000000000000, -7.088010851410853519 ) ) ;
#129535 = DIRECTION ( 'NONE',  ( 0.000000000000000000, 1.000000000000000000, 0.000000000000000000 ) ) ;
#129536 = VERTEX_POINT ( 'NONE', #48675 ) ;
#129537 = VERTEX_POINT ( 'NONE', #78140 ) ;
#129538 = EDGE_CURVE ( 'NONE', #95183, #43428, #76908, .T. ) ;
#129539 = DIRECTION ( 'NONE',  ( -0.000000000000000000, -1.000000000000000000, -0.000000000000000000 ) ) ;
#129540 = ORIENTED_EDGE ( 'NONE', *, *, #61817, .F. ) ;
#129541 = VERTEX_POINT ( 'NONE', #68296 ) ;
#129542 = EDGE_CURVE ( 'NONE', #120092, #92046, #48036, .T. ) ;
#129543 = CARTESIAN_POINT ( 'NONE',  ( 186.7343750003414300, 8.734944146203032389, 5.348610694689227483E-16 ) ) ;
#129544 = CARTESIAN_POINT ( 'NONE',  ( 9.149999999999915090, 12.50000000000000000, -2.230156782645139391 ) ) ;
#129545 = CARTESIAN_POINT ( 'NONE',  ( -11.64999999999999680, 12.50000000000000000, -7.188010851410850499 ) ) ;
#129546 = ADVANCED_FACE ( 'NONE', ( #70246 ), #102046, .T. ) ;
#129547 = DIRECTION ( 'NONE',  ( -0.000000000000000000, 1.000000000000000000, -0.000000000000000000 ) ) ;
#129548 = DIRECTION ( 'NONE',  ( 0.000000000000000000, 0.000000000000000000, 1.000000000000000000 ) ) ;
#129549 = DIRECTION ( 'NONE',  ( -0.000000000000000000, 1.000000000000000000, -0.000000000000000000 ) ) ;
#129550 = PLANE ( 'NONE',  #87448 ) ;
#129551 = EDGE_CURVE ( 'NONE', #117178, #97440, #14229, .T. ) ;
#129552 = ADVANCED_FACE ( 'NONE', ( #128548 ), #78794, .T. ) ;
#129553 = AXIS2_PLACEMENT_3D ( 'NONE', #31614, #40808, #51903 ) ;
#129554 = EDGE_CURVE ( 'NONE', #113501, #94166, #62999, .T. ) ;
#129555 = DIRECTION ( 'NONE',  ( -0.000000000000000000, 1.000000000000000000, -0.000000000000000000 ) ) ;
#129556 = ORIENTED_EDGE ( 'NONE', *, *, #119415, .T. ) ;
#129559 = EDGE_CURVE ( 'NONE', #90845, #48001, #45623, .T. ) ;
#129558 = AXIS2_PLACEMENT_3D ( 'NONE', #126854, #37192, #98024 ) ;
#129557 = AXIS2_PLACEMENT_3D ( 'NONE', #57423, #18773, #97338 ) ;
#129560 = ORIENTED_EDGE ( 'NONE', *, *, #112312, .T. ) ;
#129561 = AXIS2_PLACEMENT_3D ( 'NONE', #74884, #44129, #63782 ) ;
#129562 = ORIENTED_EDGE ( 'NONE', *, *, #41038, .F. ) ;
#129563 = ORIENTED_EDGE ( 'NONE', *, *, #103474, .T. ) ;
#129564 = CARTESIAN_POINT ( 'NONE',  ( -5.450000000000019718, 2.500000000000000000, 2.165063509461097713 ) ) ;
#129565 = CARTESIAN_POINT ( 'NONE',  ( -11.84999999999999609, 2.500000000000000000, 2.411473670974873862 ) ) ;
#129566 = EDGE_CURVE ( 'NONE', #74274, #91624, #41427, .T. ) ;
#129569 = EDGE_LOOP ( 'NONE', ( #31833, #88252 ) ) ;
#129568 = AXIS2_PLACEMENT_3D ( 'NONE', #35713, #67741, #107676 ) ;
#129567 = CIRCLE ( 'NONE', #1988, 0.1000000000000002554 ) ;
#129570 = DIRECTION ( 'NONE',  ( 0.000000000000000000, -0.000000000000000000, 1.000000000000000000 ) ) ;
#129571 = DIRECTION ( 'NONE',  ( 0.000000000000000000, 0.000000000000000000, 1.000000000000000000 ) ) ;
#129572 = LINE ( 'NONE', #20235, #32651 ) ;
#129574 = EDGE_LOOP ( 'NONE', ( #129497, #67311, #60689, #108216 ) ) ;
#129573 = CARTESIAN_POINT ( 'NONE',  ( 11.04999999999991012, 12.50000000000000000, 6.776507416713035248 ) ) ;
#129575 = DIRECTION ( 'NONE',  ( -0.000000000000000000, 1.000000000000000000, -0.000000000000000000 ) ) ;
#129576 = CARTESIAN_POINT ( 'NONE',  ( 4.599999999999936584, 2.500000000000000000, 4.430127018922196847 ) ) ;
#129577 = VERTEX_POINT ( 'NONE', #856 ) ;
#129578 = ORIENTED_EDGE ( 'NONE', *, *, #93946, .F. ) ;
#129579 = ORIENTED_EDGE ( 'NONE', *, *, #40904, .T. ) ;
#129580 = ORIENTED_EDGE ( 'NONE', *, *, #35816, .T. ) ;
#129581 = CARTESIAN_POINT ( 'NONE',  ( 5.599999999999931255, 2.500000000000000000, 3.883716857408420431 ) ) ;
#129582 = CARTESIAN_POINT ( 'NONE',  ( 8.749999999999920064, 2.500000000000000000, 5.702370205355745014 ) ) ;
#129583 = DIRECTION ( 'NONE',  ( -0.000000000000000000, -1.000000000000000000, -0.000000000000000000 ) ) ;
#129584 = AXIS2_PLACEMENT_3D ( 'NONE', #101059, #90586, #40878 ) ;
#129585 = AXIS2_PLACEMENT_3D ( 'NONE', #16805, #126798, #107797 ) ;
#129586 = EDGE_LOOP ( 'NONE', ( #45447, #107380 ) ) ;
#129587 = DIRECTION ( 'NONE',  ( 0.000000000000000000, -0.000000000000000000, 1.000000000000000000 ) ) ;
#129588 = CARTESIAN_POINT ( 'NONE',  ( 21.24754738303276724, -0.7337760880902383098, -4.182111650399352953 ) ) ;
#129589 = PLANE ( 'NONE',  #369 ) ;
#129590 = LINE ( 'NONE', #30743, #44237 ) ;
#129592 = AXIS2_PLACEMENT_3D ( 'NONE', #115288, #25641, #65572 ) ;
#129591 = AXIS2_PLACEMENT_3D ( 'NONE', #101826, #59345, #9578 ) ;
#129593 = ORIENTED_EDGE ( 'NONE', *, *, #1694, .F. ) ;
#129594 = LINE ( 'NONE', #39289, #12340 ) ;
#129595 = EDGE_CURVE ( 'NONE', #33637, #62109, #68581, .T. ) ;
#129596 = ORIENTED_EDGE ( 'NONE', *, *, #80926, .F. ) ;
#129597 = VERTEX_POINT ( 'NONE', #91171 ) ;
#129598 = DIRECTION ( 'NONE',  ( 0.000000000000000000, -0.000000000000000000, 1.000000000000000000 ) ) ;
#129599 = CARTESIAN_POINT ( 'NONE',  ( 13.54999999999990123, 12.50000000000000000, 1.883746621131358934 ) ) ;
#129600 = FACE_BOUND ( 'NONE', #13872, .T. ) ;
#129601 = VECTOR ( 'NONE', #64863, 1000.000000000000000 ) ;
#129602 = CARTESIAN_POINT ( 'NONE',  ( -8.749999999999975131, 2.500000000000000000, -2.065063509461102065 ) ) ;
#129603 = CARTESIAN_POINT ( 'NONE',  ( 11.44999999999990692, 2.500000000000000000, 1.718653347947321386 ) ) ;
#129604 = CARTESIAN_POINT ( 'NONE',  ( 5.449999999999937117, 12.50000000000000000, -6.495190528383302464 ) ) ;
#129605 = EDGE_CURVE ( 'NONE', #118548, #56615, #81123, .T. ) ;
#129606 = AXIS2_PLACEMENT_3D ( 'NONE', #98301, #48580, #10560 ) ;
#129607 = DIRECTION ( 'NONE',  ( -0.000000000000000000, 1.000000000000000000, -0.000000000000000000 ) ) ;
#129608 = CARTESIAN_POINT ( 'NONE',  ( 184.5000000000000000, 0.000000000000000000, -7.699999999999999289 ) ) ;
#129609 = DIRECTION ( 'NONE',  ( 0.000000000000000000, 0.000000000000000000, 1.000000000000000000 ) ) ;
#129610 = DIRECTION ( 'NONE',  ( 0.000000000000000000, -0.9999939076577903929, 0.003490651415223739937 ) ) ;
#129611 = ORIENTED_EDGE ( 'NONE', *, *, #7416, .F. ) ;
#129612 = VECTOR ( 'NONE', #54208, 1000.000000000000000 ) ;
#129613 = DIRECTION ( 'NONE',  ( 0.000000000000000000, 1.000000000000000000, 0.000000000000000000 ) ) ;
#129614 = CARTESIAN_POINT ( 'NONE',  ( 11.64999999999990266, 2.500000000000000000, 2.065063509461097624 ) ) ;
#129615 = AXIS2_PLACEMENT_3D ( 'NONE', #63588, #94313, #125077 ) ;
#129616 = VERTEX_POINT ( 'NONE', #52536 ) ;
#129617 = CARTESIAN_POINT ( 'NONE',  ( 184.5000000000000000, 0.000000000000000000, 7.700000000000000178 ) ) ;
#129618 = NEXT_ASSEMBLY_USAGE_OCCURRENCE ( 'NAUO1', ' ', ' ', #28456, #65974, $ ) ;
#129619 = NEXT_ASSEMBLY_USAGE_OCCURRENCE ( 'NAUO2', ' ', ' ', #28456, #98771, $ ) ;
#129620 = NEXT_ASSEMBLY_USAGE_OCCURRENCE ( 'NAUO3', ' ', ' ', #28456, #92424, $ ) ;
#129621 = NEXT_ASSEMBLY_USAGE_OCCURRENCE ( 'NAUO4', ' ', ' ', #28456, #88428, $ ) ;
#129622 = NEXT_ASSEMBLY_USAGE_OCCURRENCE ( 'NAUO5', ' ', ' ', #28456, #98041, $ ) ;
#129623 = NEXT_ASSEMBLY_USAGE_OCCURRENCE ( 'NAUO6', ' ', ' ', #28456, #14818, $ ) ;
#129624 = NEXT_ASSEMBLY_USAGE_OCCURRENCE ( 'NAUO7', ' ', ' ', #28456, #61261, $ ) ;
#129625 = NEXT_ASSEMBLY_USAGE_OCCURRENCE ( 'NAUO8', ' ', ' ', #28456, #5236, $ ) ;
ENDSEC;
END-ISO-10303-21;
